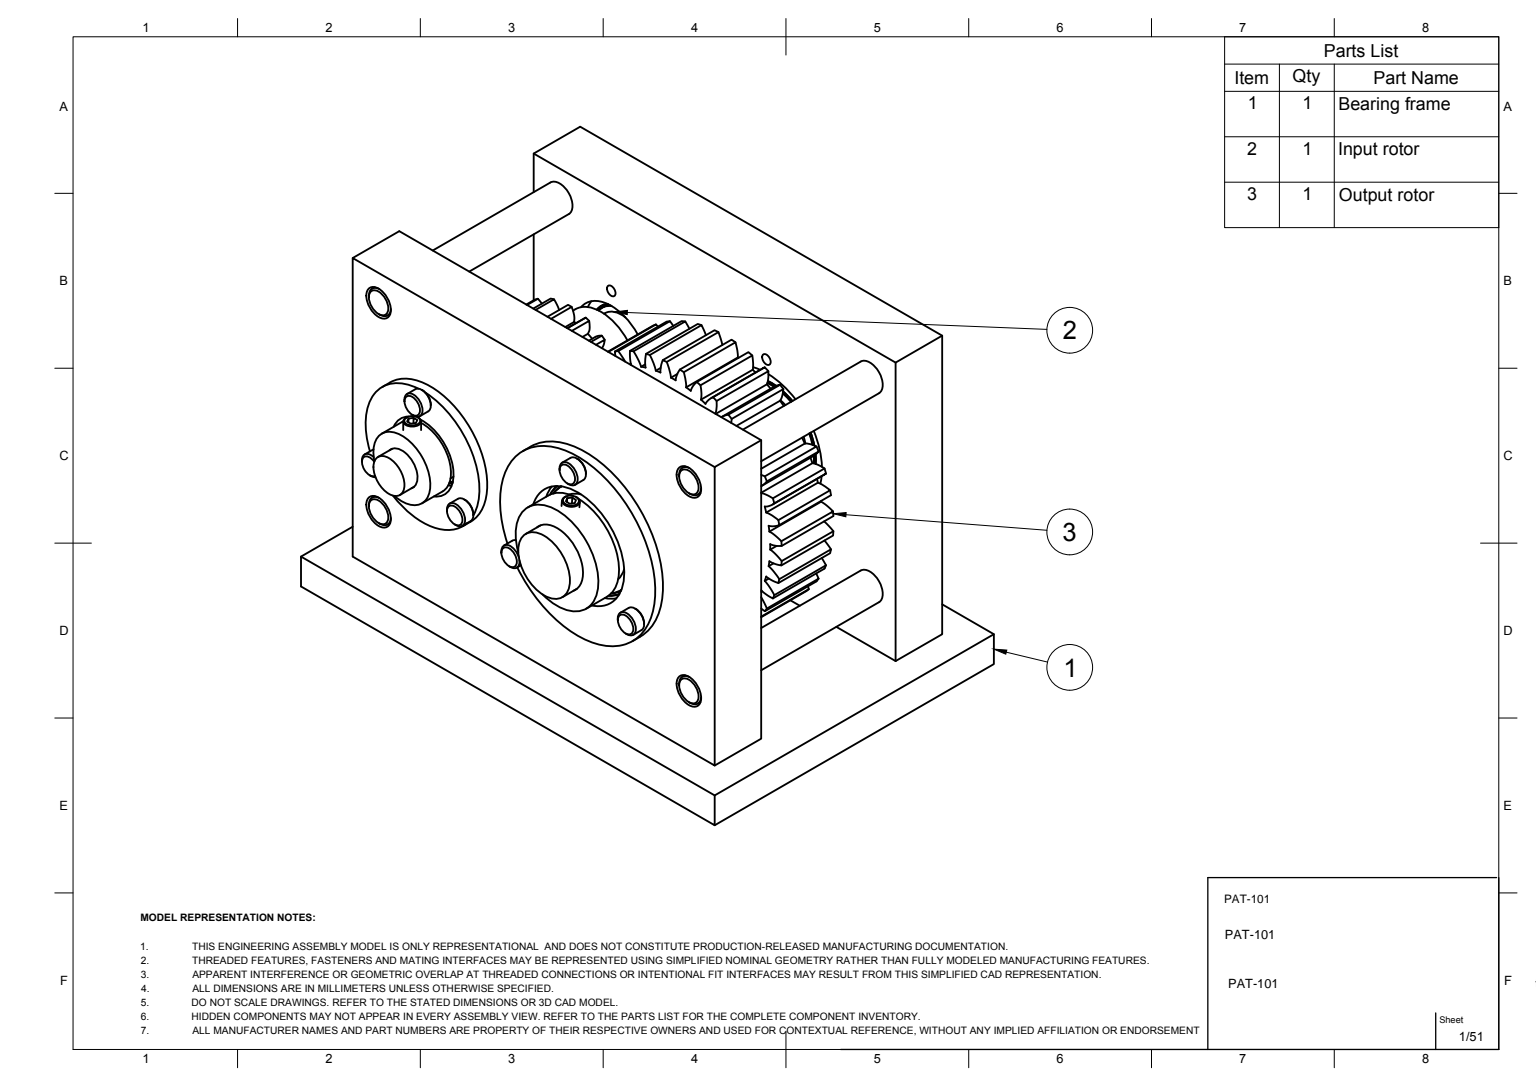
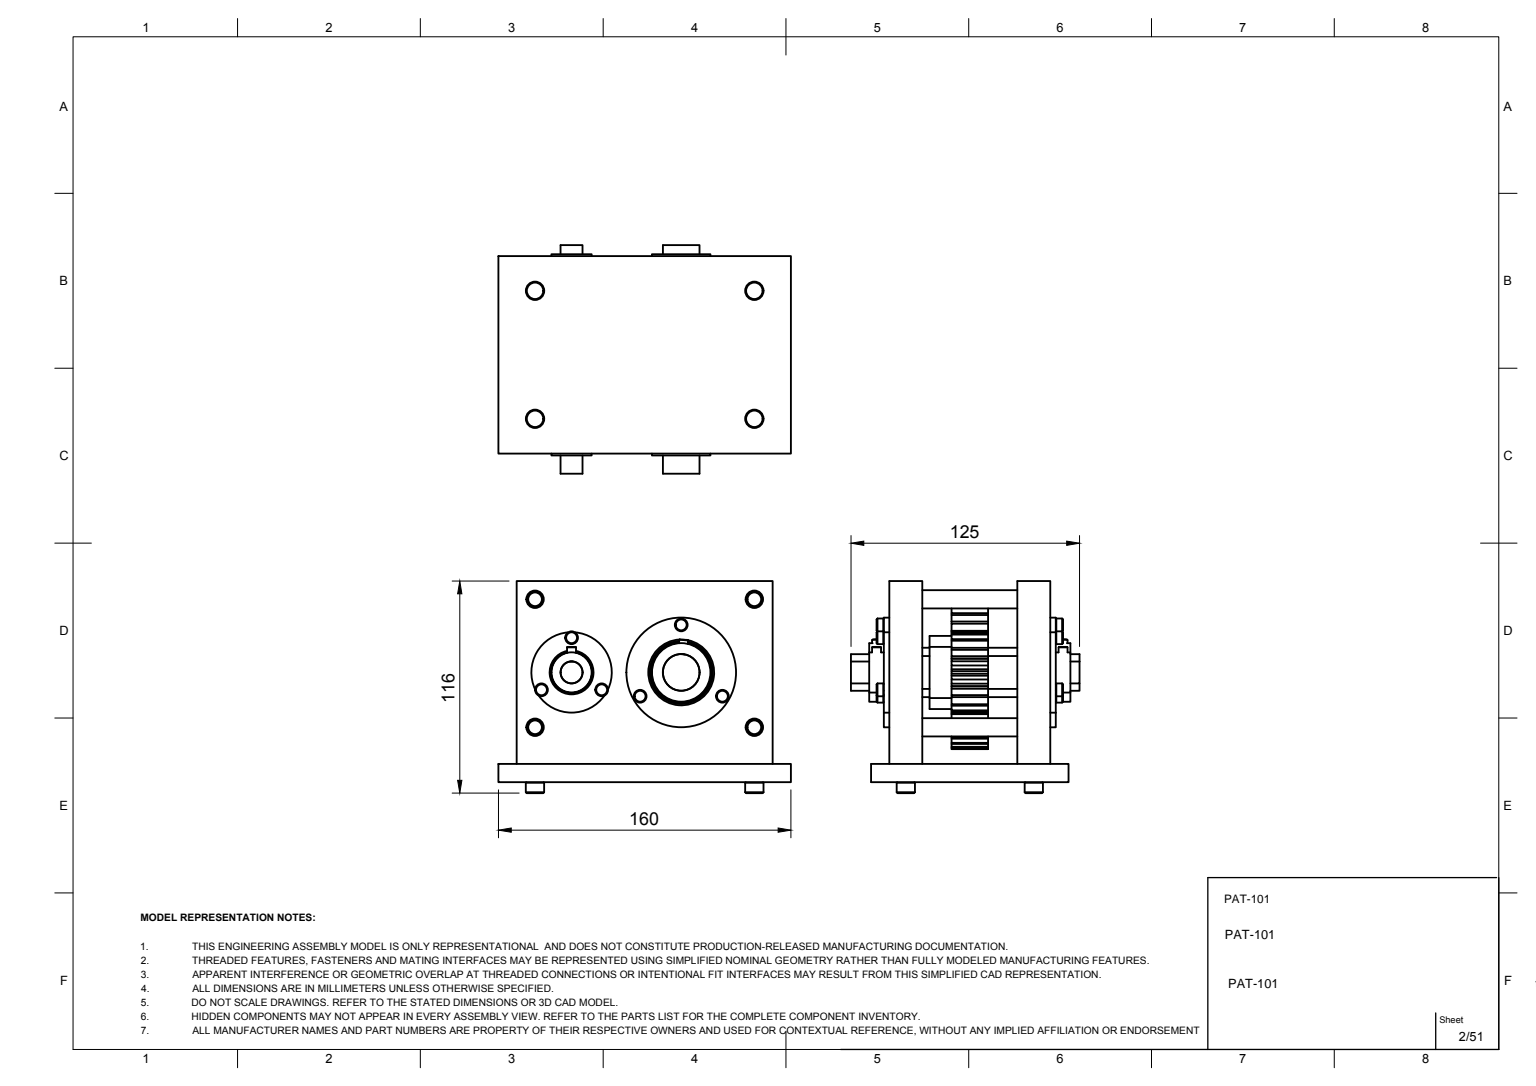
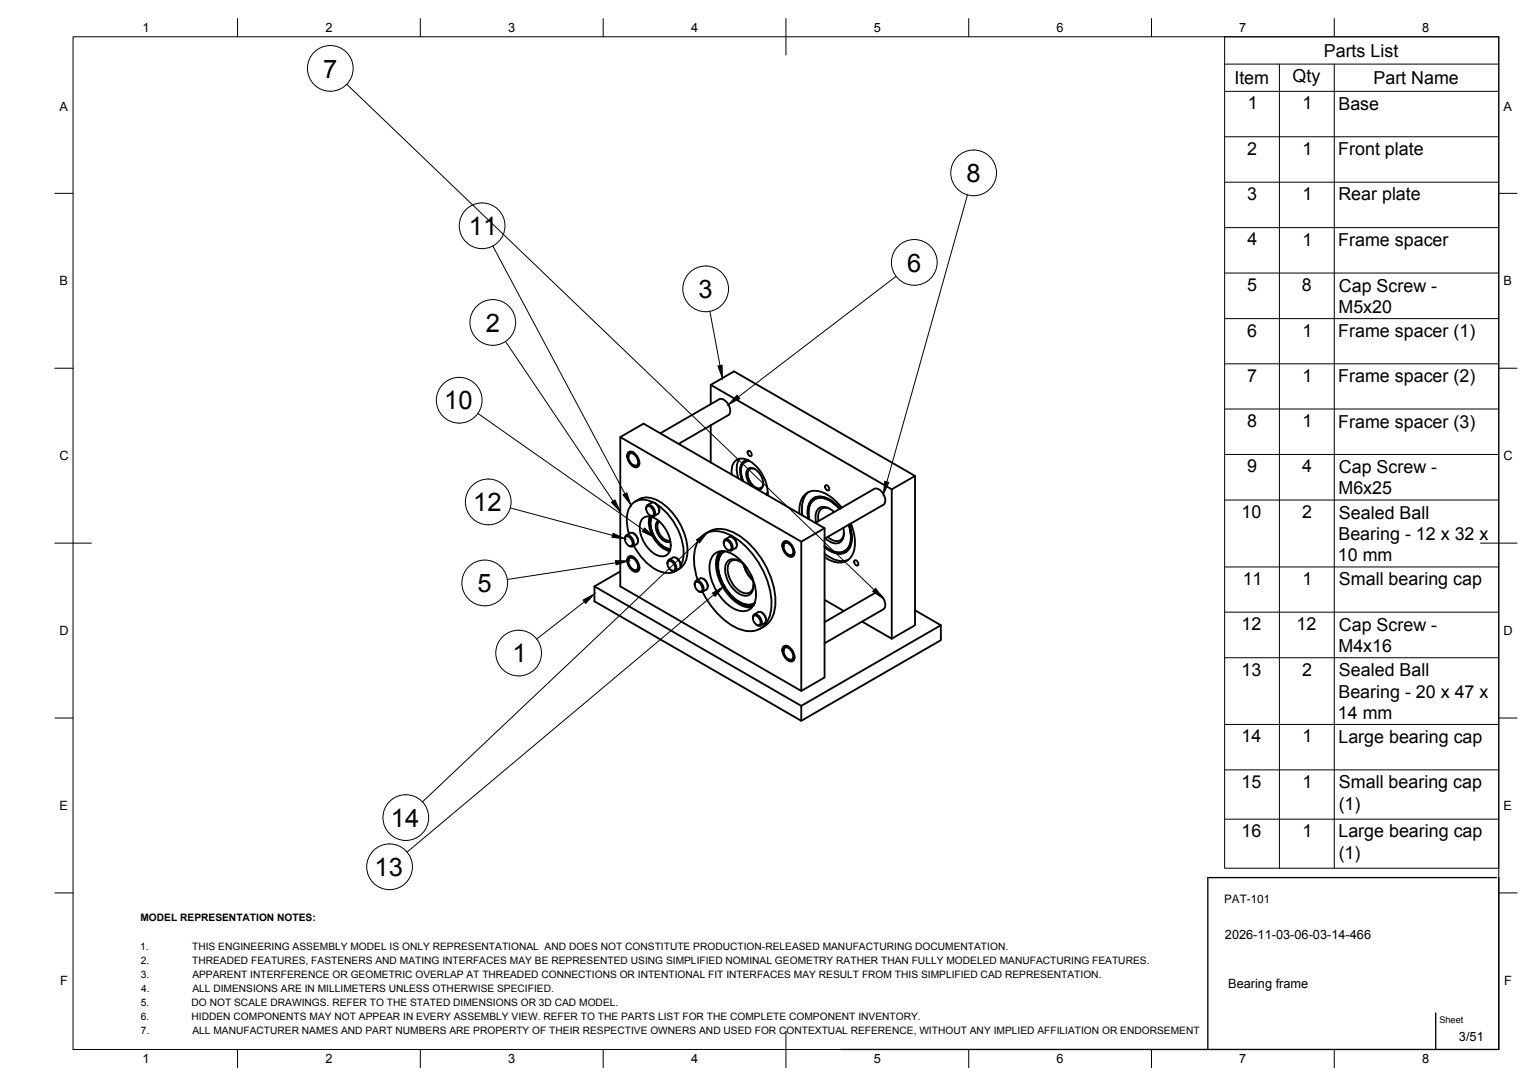
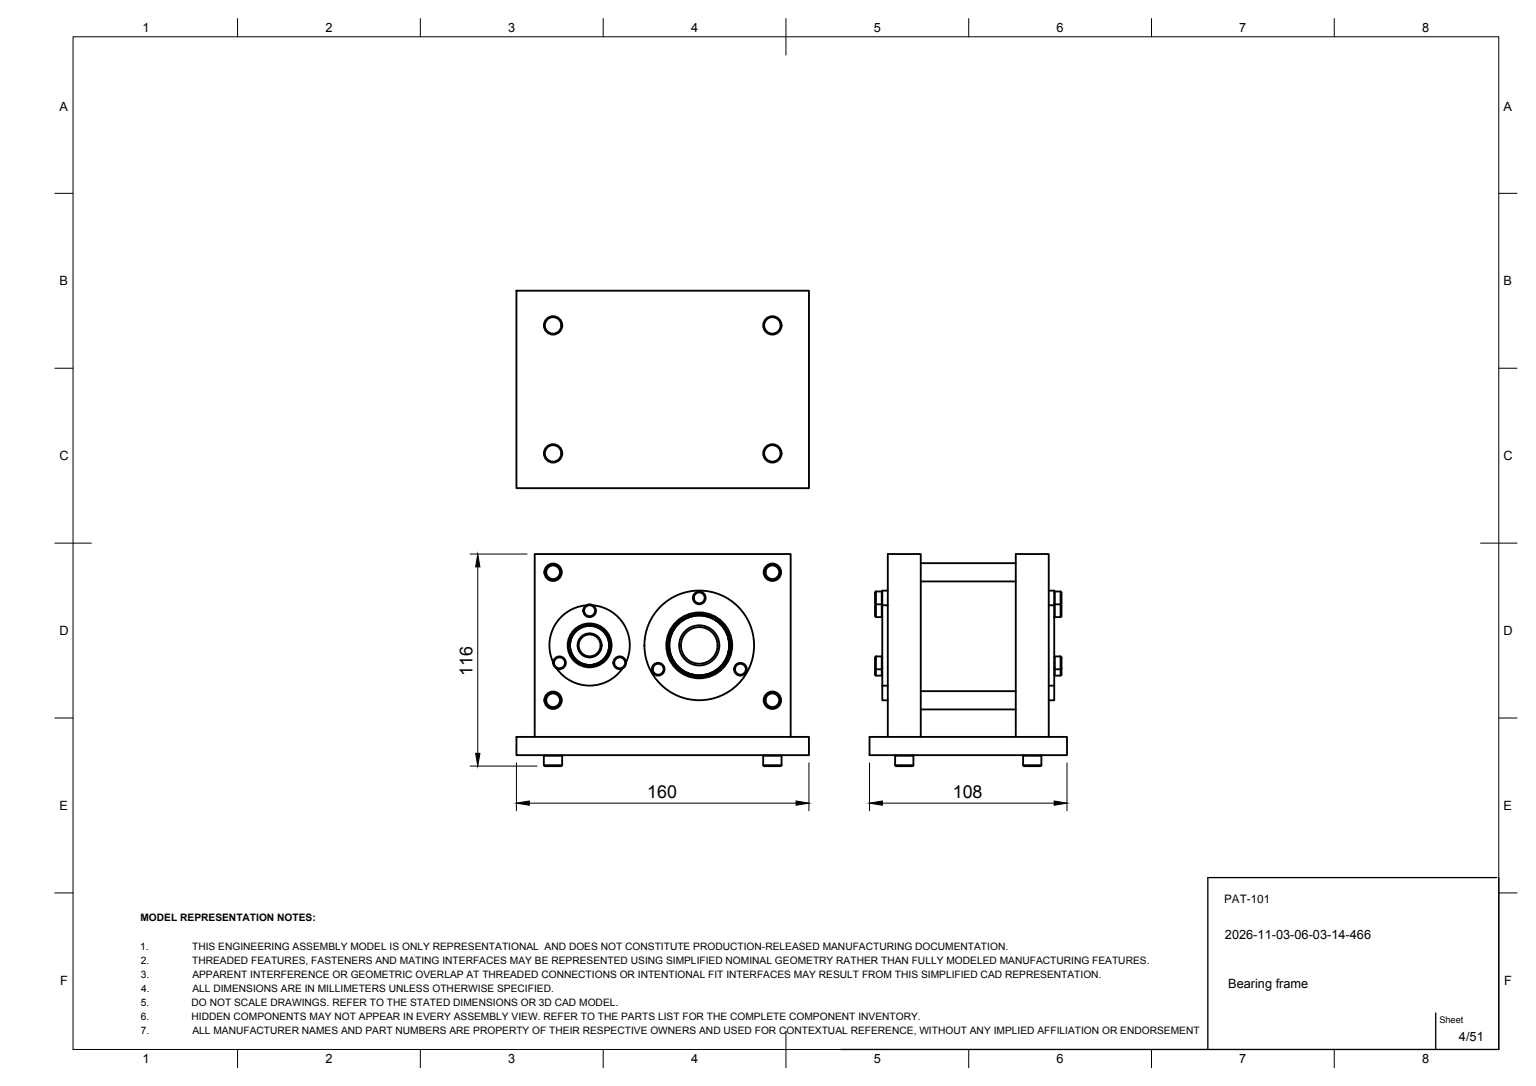
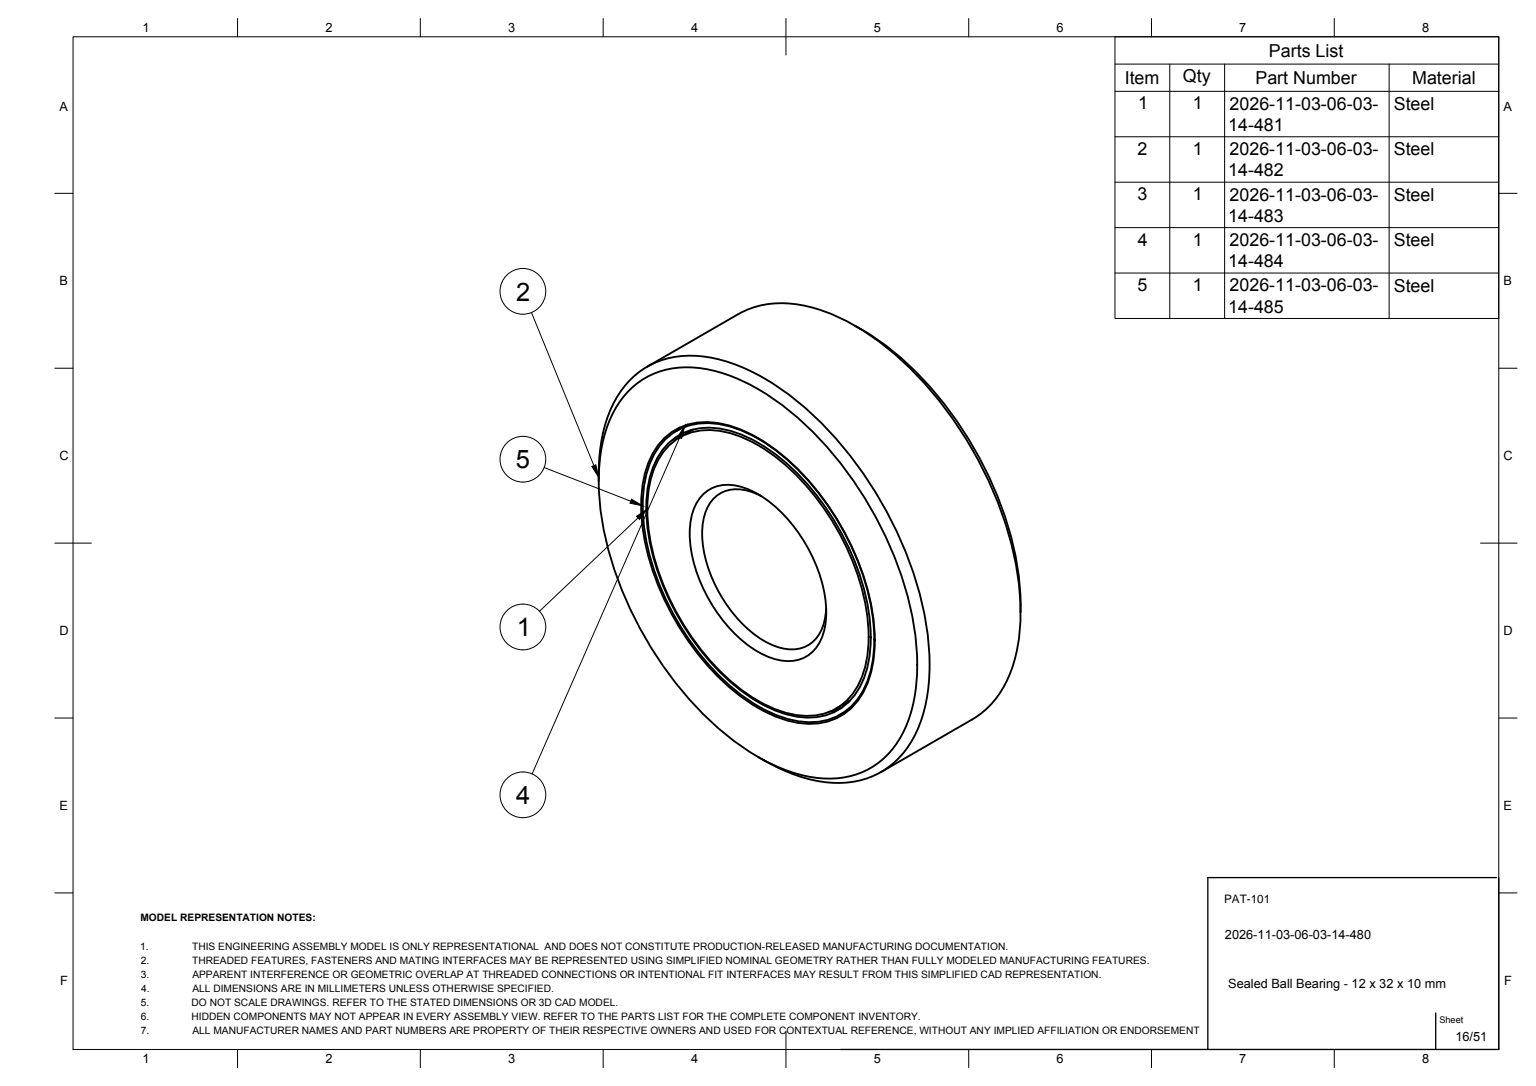
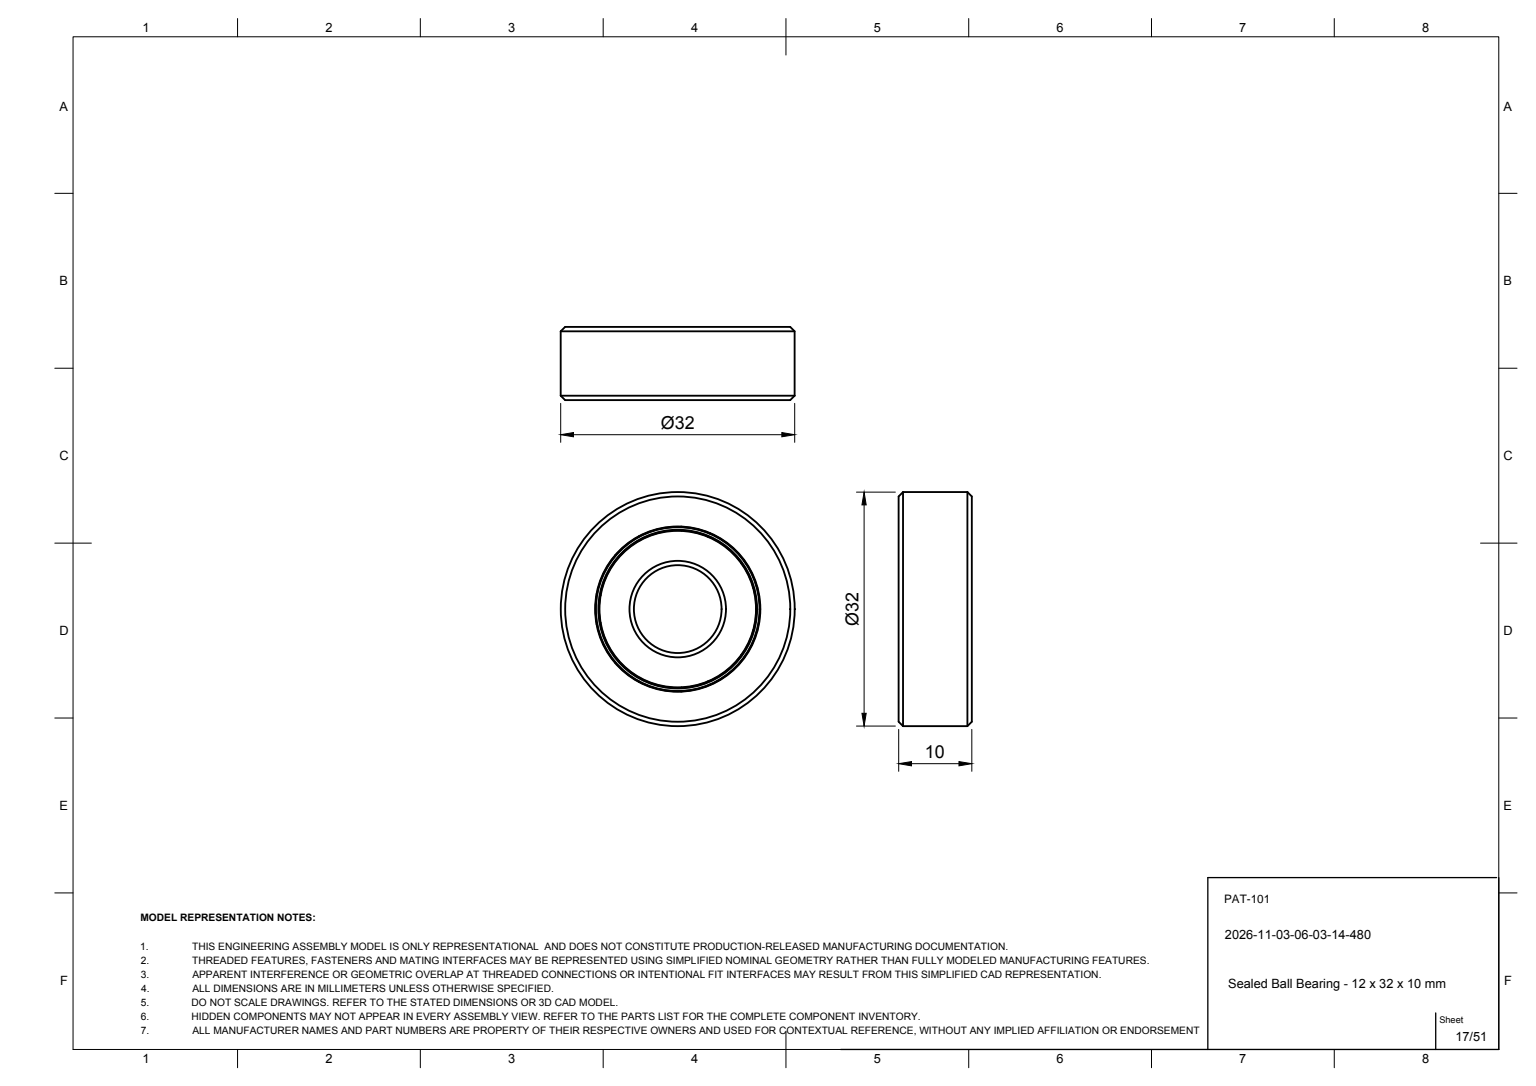
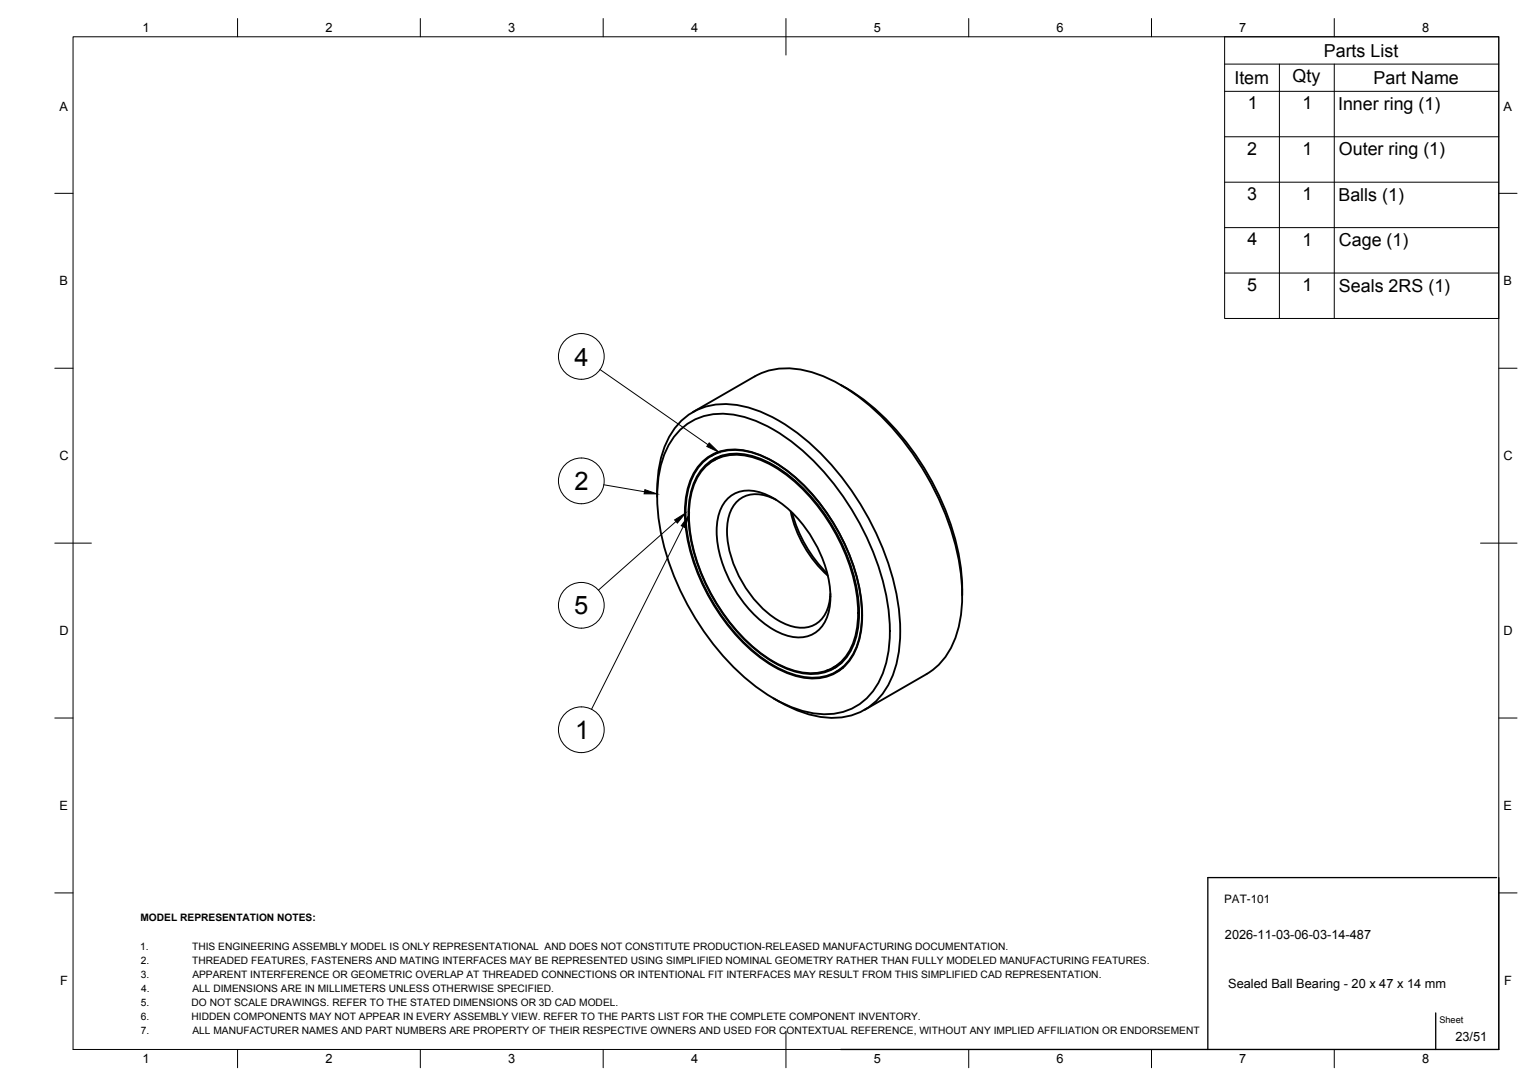
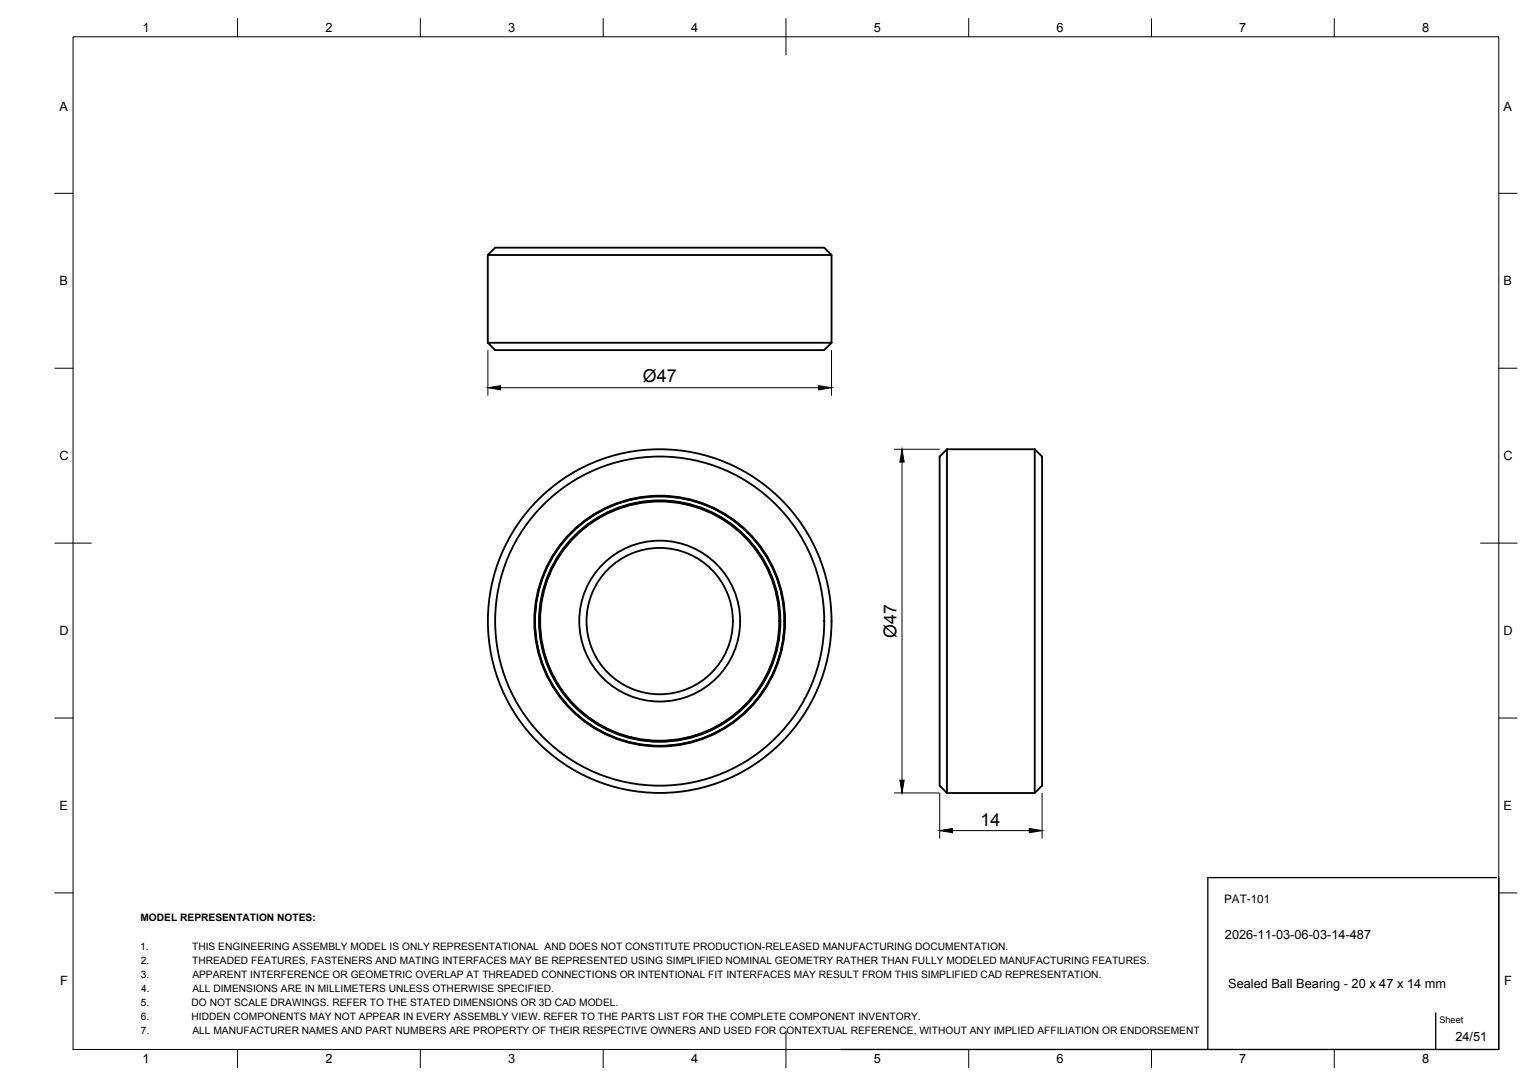
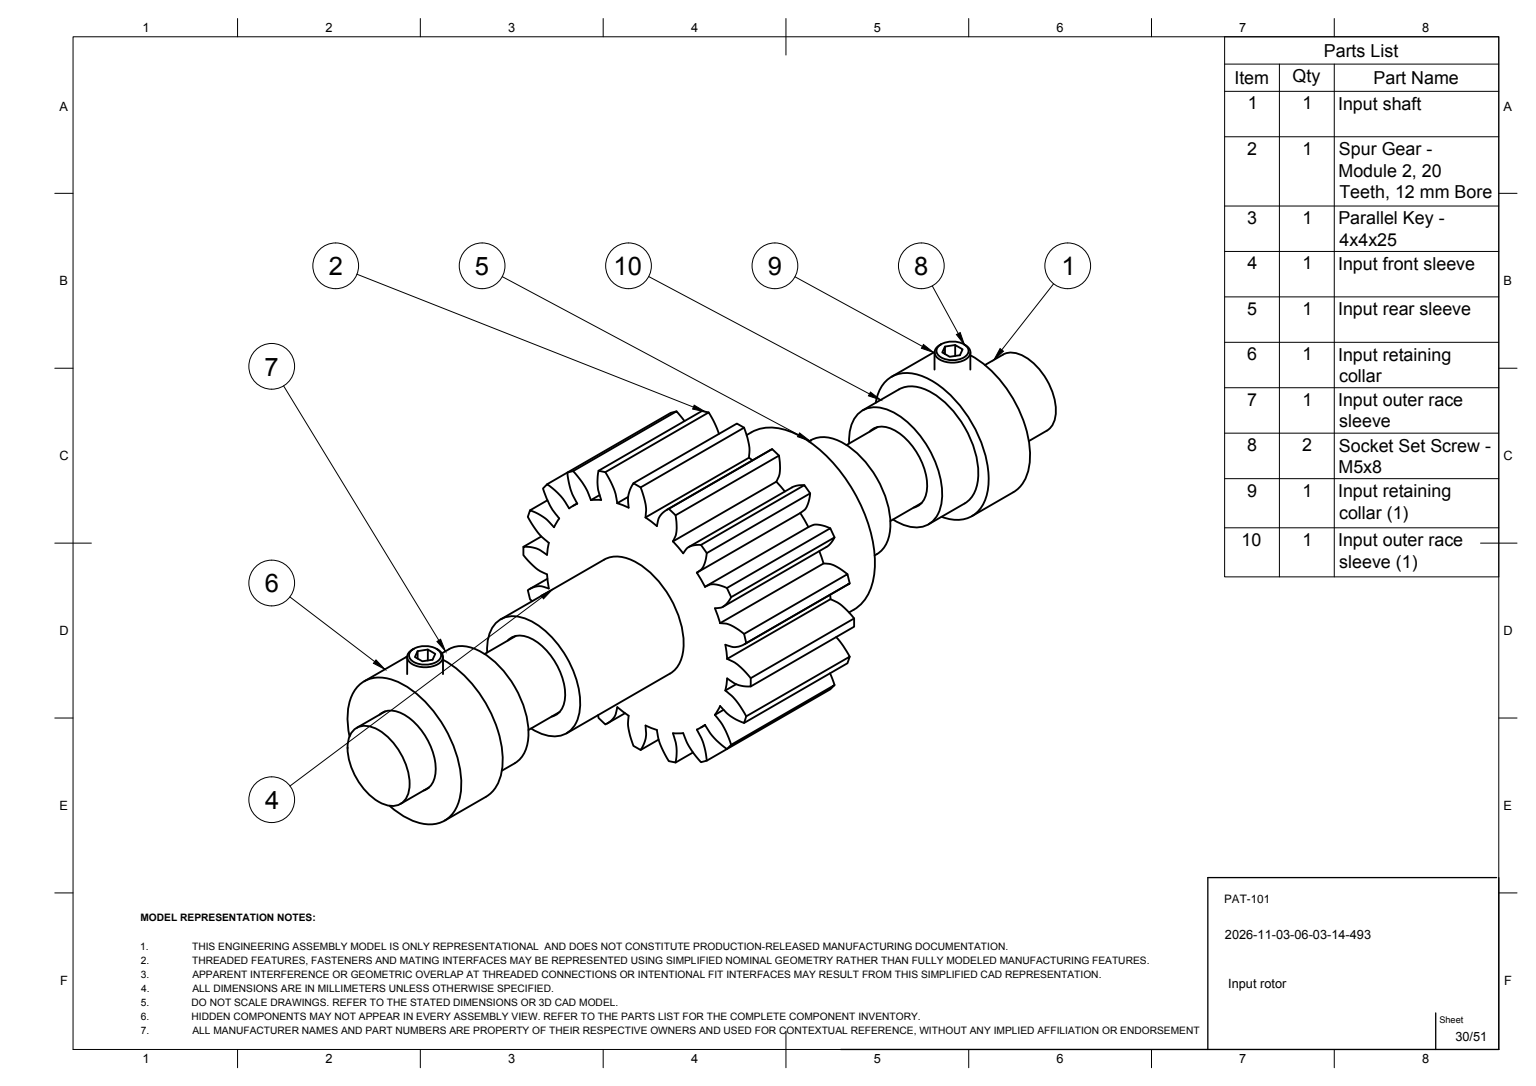
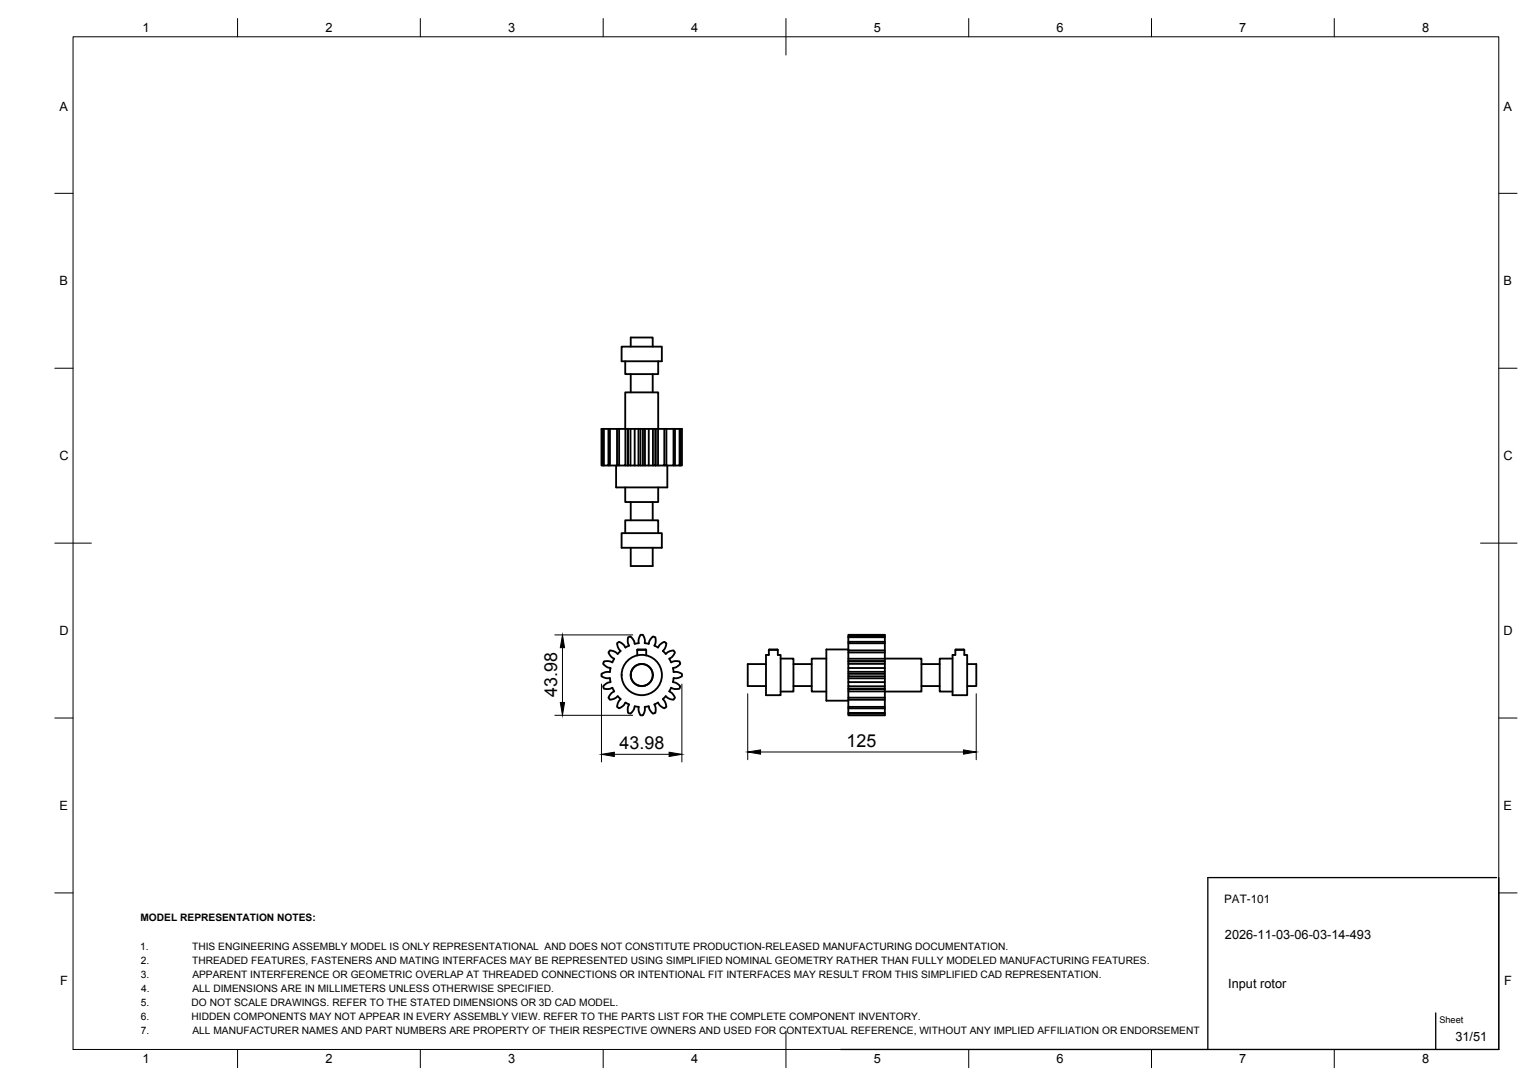
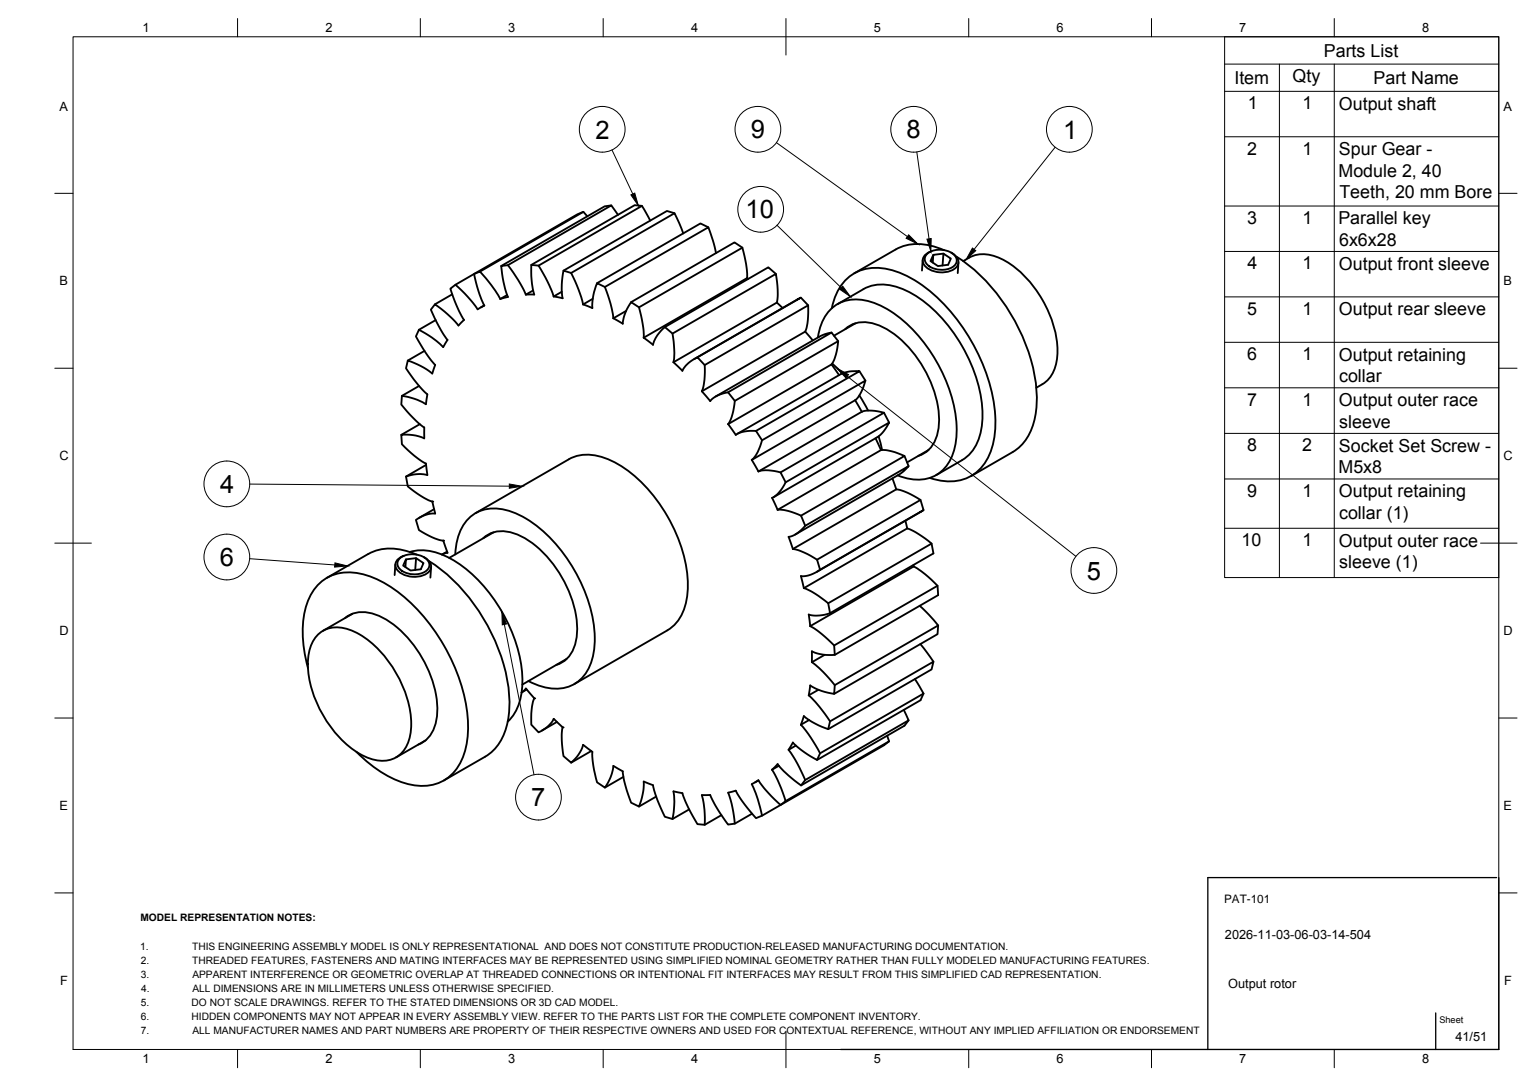
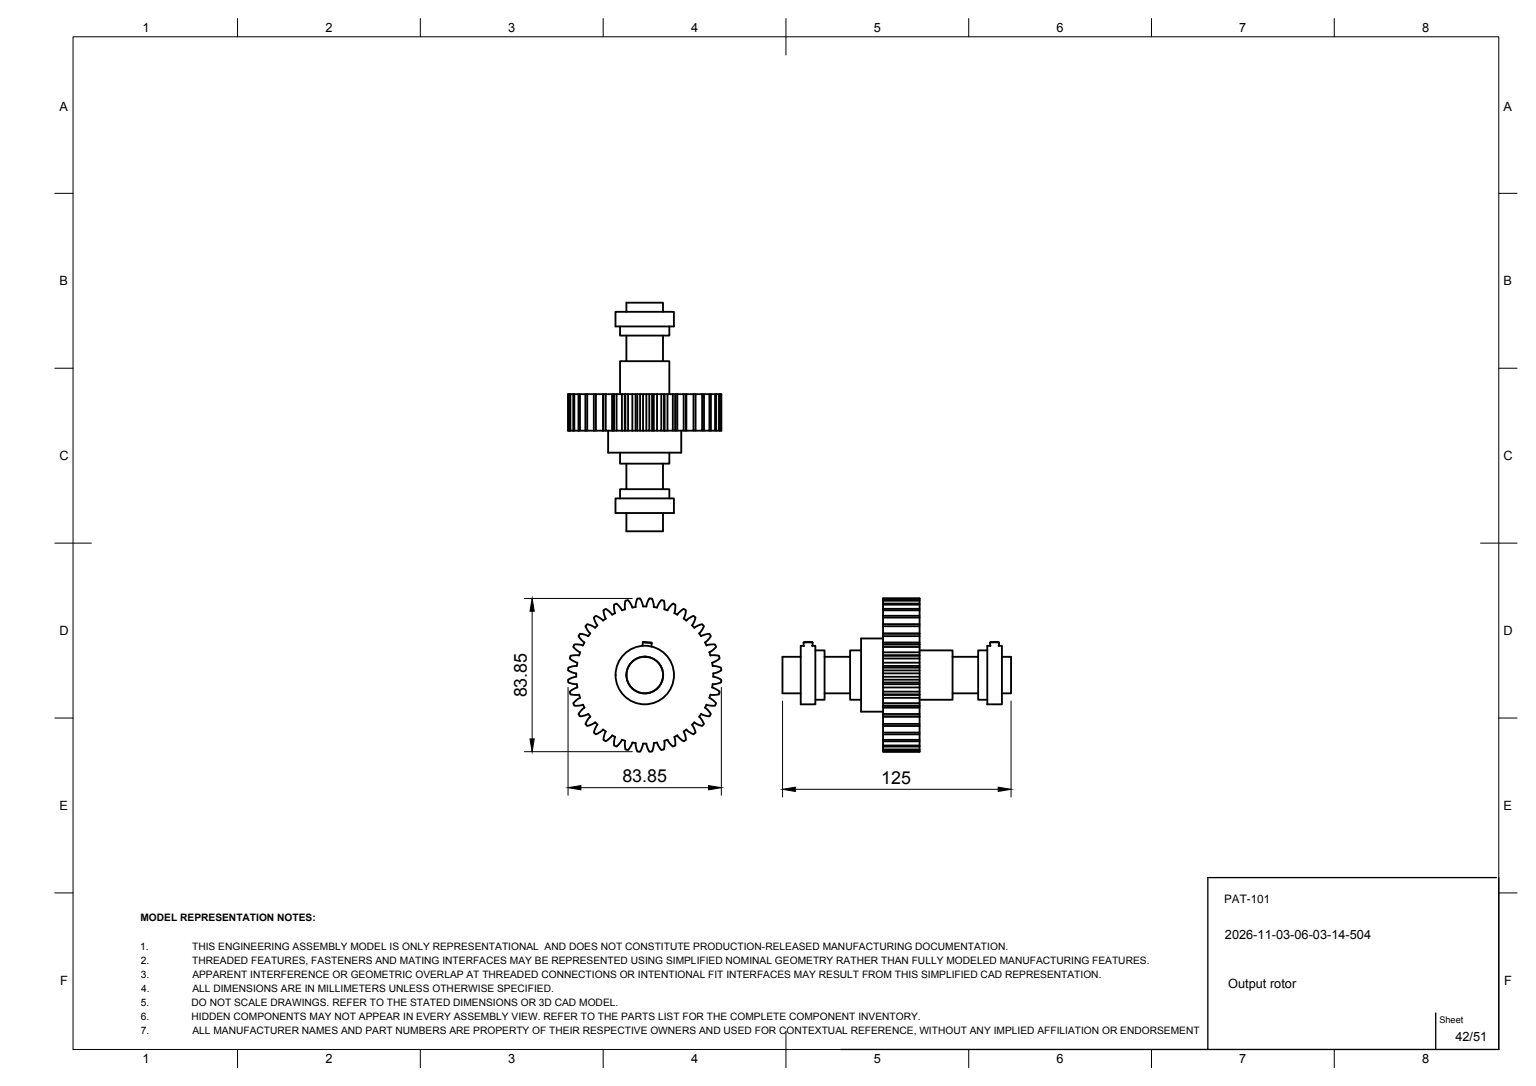
ISO-10303-21;
HEADER;
/* Generated by software containing ST-Developer
 * from STEP Tools, Inc. (www.steptools.com) 
 */

FILE_DESCRIPTION(
/* description */ ('Spur gear reduction stage 2-1 on bearing plates'),
/* implementation_level */ '2;1');

FILE_NAME(
/* name */ 'PAT-101',
/* time_stamp */ '2026-10-28T03:22:07-07:00',
/* author */ (''),
/* organization */ (''),
/* preprocessor_version */ 'ST-DEVELOPER v20.2',
/* originating_system */ 'Autodesk Translation Framework v15.17.0.0',
/* authorisation */ '');

FILE_SCHEMA (('AUTOMOTIVE_DESIGN { 1 0 10303 214 3 1 1 }'));
ENDSEC;

DATA;
#10=MECHANICAL_DESIGN_GEOMETRIC_PRESENTATION_REPRESENTATION('',(#947,#948,
#949,#950,#951,#952,#953,#954,#955,#956,#957,#958,#959,#960,#961,#962,#963,
#964,#965,#966,#967,#968,#969,#970,#971,#972,#973,#974,#975,#976,#977,#978,
#979,#980,#981,#982,#983,#984,#985,#986,#987,#988,#989,#990,#991,#992,#993,
#994,#995,#996,#997,#998,#999,#1000,#1001,#1002,#1003,#1004),#53909);
#11=(
BOUNDED_SURFACE()
B_SPLINE_SURFACE(5,1,((#21141,#21142),(#21143,#21144),(#21145,#21146),(#21147,
#21148),(#21149,#21150),(#21151,#21152),(#21153,#21154),(#21155,#21156),
(#21157,#21158),(#21159,#21160),(#21161,#21162),(#21163,#21164),(#21165,
#21166),(#21167,#21168),(#21169,#21170),(#21171,#21172),(#21173,#21174),
(#21175,#21176),(#21177,#21178),(#21179,#21180),(#21181,#21182),(#21183,
#21184),(#21185,#21186),(#21187,#21188),(#21189,#21190),(#21191,#21192),
(#21193,#21194),(#21195,#21196),(#21197,#21198),(#21199,#21200),(#21201,
#21202),(#21203,#21204),(#21205,#21206),(#21207,#21208),(#21209,#21210),
(#21211,#21212),(#21213,#21214),(#21215,#21216),(#21217,#21218),(#21219,
#21220),(#21221,#21222),(#21223,#21224),(#21225,#21226),(#21227,#21228),
(#21229,#21230),(#21231,#21232),(#21233,#21234),(#21235,#21236),(#21237,
#21238),(#21239,#21240),(#21241,#21242),(#21243,#21244),(#21245,#21246),
(#21247,#21248),(#21249,#21250),(#21251,#21252),(#21253,#21254),(#21255,
#21256),(#21257,#21258),(#21259,#21260),(#21261,#21262),(#21263,#21264),
(#21265,#21266),(#21267,#21268),(#21269,#21270),(#21271,#21272),(#21273,
#21274),(#21275,#21276),(#21277,#21278),(#21279,#21280)),.UNSPECIFIED.,
 .F.,.F.,.F.)
B_SPLINE_SURFACE_WITH_KNOTS((6,1,1,1,1,1,1,1,1,1,1,1,1,1,1,1,1,1,1,1,1,
1,1,1,1,1,1,1,1,1,1,1,1,1,1,1,1,1,1,1,1,1,1,1,1,1,1,1,1,1,1,1,1,1,1,1,1,
1,1,1,1,1,1,1,1,6),(2,2),(-1.,-0.984615384615383,-0.969230769230768,-0.953846153846152,
-0.938461538461537,-0.923076923076922,-0.907692307692306,-0.892307692307691,
-0.876923076923076,-0.86153846153846,-0.846153846153845,-0.83076923076923,
-0.815384615384614,-0.799999999999999,-0.784615384615384,-0.769230769230768,
-0.753846153846153,-0.738461538461538,-0.723076923076922,-0.707692307692307,
-0.692307692307692,-0.676923076923076,-0.661538461538461,-0.646153846153846,
-0.63076923076923,-0.615384615384615,-0.6,-0.584615384615384,-0.569230769230769,
-0.553846153846154,-0.538461538461538,-0.523076923076923,-0.507692307692308,
-0.492307692307692,-0.476923076923077,-0.461538461538462,-0.446153846153846,
-0.430769230769231,-0.415384615384615,-0.4,-0.384615384615385,-0.369230769230769,
-0.353846153846154,-0.338461538461538,-0.323076923076923,-0.307692307692308,
-0.292307692307692,-0.276923076923077,-0.261538461538462,-0.246153846153846,
-0.230769230769231,-0.215384615384615,-0.2,-0.184615384615385,-0.169230769230769,
-0.153846153846154,-0.138461538461538,-0.123076923076923,-0.107692307692308,
-0.0923076923076923,-0.0769230769230769,-0.0615384615384615,-0.0461538461538462,
-0.0307692307692308,-0.0153846153846154,0.),(-1.,1.),.UNSPECIFIED.)
GEOMETRIC_REPRESENTATION_ITEM()
RATIONAL_B_SPLINE_SURFACE(((1.,1.),(1.,1.),(1.,1.),(1.,1.),(1.,1.),(1.,
1.),(1.,1.),(1.,1.),(1.,1.),(1.,1.),(1.,1.),(1.,1.),(1.,1.),(1.,1.),(1.,
1.),(1.,1.),(1.,1.),(1.,1.),(1.,1.),(1.,1.),(1.,1.),(1.,1.),(1.,1.),(1.,
1.),(1.,1.),(1.,1.),(1.,1.),(1.,1.),(1.,1.),(1.,1.),(1.,1.),(1.,1.),(1.,
1.),(1.,1.),(1.,1.),(1.,1.),(1.,1.),(1.,1.),(1.,1.),(1.,1.),(1.,1.),(1.,
1.),(1.,1.),(1.,1.),(1.,1.),(1.,1.),(1.,1.),(1.,1.),(1.,1.),(1.,1.),(1.,
1.),(1.,1.),(1.,1.),(1.,1.),(1.,1.),(1.,1.),(1.,1.),(1.,1.),(1.,1.),(1.,
1.),(1.,1.),(1.,1.),(1.,1.),(1.,1.),(1.,1.),(1.,1.),(1.,1.),(1.,1.),(1.,
1.),(1.,1.)))
REPRESENTATION_ITEM('')
SURFACE()
);
#12=(
BOUNDED_SURFACE()
B_SPLINE_SURFACE(5,1,((#21359,#21360),(#21361,#21362),(#21363,#21364),(#21365,
#21366),(#21367,#21368),(#21369,#21370),(#21371,#21372),(#21373,#21374),
(#21375,#21376),(#21377,#21378),(#21379,#21380),(#21381,#21382),(#21383,
#21384),(#21385,#21386),(#21387,#21388),(#21389,#21390),(#21391,#21392),
(#21393,#21394),(#21395,#21396),(#21397,#21398),(#21399,#21400),(#21401,
#21402),(#21403,#21404),(#21405,#21406),(#21407,#21408),(#21409,#21410),
(#21411,#21412),(#21413,#21414),(#21415,#21416),(#21417,#21418),(#21419,
#21420),(#21421,#21422),(#21423,#21424),(#21425,#21426),(#21427,#21428),
(#21429,#21430),(#21431,#21432),(#21433,#21434),(#21435,#21436),(#21437,
#21438),(#21439,#21440),(#21441,#21442),(#21443,#21444),(#21445,#21446),
(#21447,#21448),(#21449,#21450),(#21451,#21452),(#21453,#21454),(#21455,
#21456),(#21457,#21458),(#21459,#21460),(#21461,#21462),(#21463,#21464),
(#21465,#21466),(#21467,#21468),(#21469,#21470),(#21471,#21472),(#21473,
#21474),(#21475,#21476),(#21477,#21478),(#21479,#21480),(#21481,#21482),
(#21483,#21484),(#21485,#21486),(#21487,#21488),(#21489,#21490),(#21491,
#21492),(#21493,#21494),(#21495,#21496),(#21497,#21498)),.UNSPECIFIED.,
 .F.,.F.,.F.)
B_SPLINE_SURFACE_WITH_KNOTS((6,1,1,1,1,1,1,1,1,1,1,1,1,1,1,1,1,1,1,1,1,
1,1,1,1,1,1,1,1,1,1,1,1,1,1,1,1,1,1,1,1,1,1,1,1,1,1,1,1,1,1,1,1,1,1,1,1,
1,1,1,1,1,1,1,1,6),(2,2),(-1.,-0.984615384615383,-0.969230769230768,-0.953846153846152,
-0.938461538461537,-0.923076923076922,-0.907692307692306,-0.892307692307691,
-0.876923076923076,-0.86153846153846,-0.846153846153845,-0.83076923076923,
-0.815384615384614,-0.799999999999999,-0.784615384615384,-0.769230769230768,
-0.753846153846153,-0.738461538461538,-0.723076923076922,-0.707692307692307,
-0.692307692307692,-0.676923076923076,-0.661538461538461,-0.646153846153846,
-0.63076923076923,-0.615384615384615,-0.6,-0.584615384615384,-0.569230769230769,
-0.553846153846154,-0.538461538461538,-0.523076923076923,-0.507692307692308,
-0.492307692307692,-0.476923076923077,-0.461538461538462,-0.446153846153846,
-0.430769230769231,-0.415384615384615,-0.4,-0.384615384615385,-0.369230769230769,
-0.353846153846154,-0.338461538461538,-0.323076923076923,-0.307692307692308,
-0.292307692307692,-0.276923076923077,-0.261538461538462,-0.246153846153846,
-0.230769230769231,-0.215384615384615,-0.2,-0.184615384615385,-0.169230769230769,
-0.153846153846154,-0.138461538461538,-0.123076923076923,-0.107692307692308,
-0.0923076923076923,-0.0769230769230769,-0.0615384615384615,-0.0461538461538462,
-0.0307692307692308,-0.0153846153846154,0.),(-1.,1.),.UNSPECIFIED.)
GEOMETRIC_REPRESENTATION_ITEM()
RATIONAL_B_SPLINE_SURFACE(((1.,1.),(1.,1.),(1.,1.),(1.,1.),(1.,1.),(1.,
1.),(1.,1.),(1.,1.),(1.,1.),(1.,1.),(1.,1.),(1.,1.),(1.,1.),(1.,1.),(1.,
1.),(1.,1.),(1.,1.),(1.,1.),(1.,1.),(1.,1.),(1.,1.),(1.,1.),(1.,1.),(1.,
1.),(1.,1.),(1.,1.),(1.,1.),(1.,1.),(1.,1.),(1.,1.),(1.,1.),(1.,1.),(1.,
1.),(1.,1.),(1.,1.),(1.,1.),(1.,1.),(1.,1.),(1.,1.),(1.,1.),(1.,1.),(1.,
1.),(1.,1.),(1.,1.),(1.,1.),(1.,1.),(1.,1.),(1.,1.),(1.,1.),(1.,1.),(1.,
1.),(1.,1.),(1.,1.),(1.,1.),(1.,1.),(1.,1.),(1.,1.),(1.,1.),(1.,1.),(1.,
1.),(1.,1.),(1.,1.),(1.,1.),(1.,1.),(1.,1.),(1.,1.),(1.,1.),(1.,1.),(1.,
1.),(1.,1.)))
REPRESENTATION_ITEM('')
SURFACE()
);
#13=(
BOUNDED_SURFACE()
B_SPLINE_SURFACE(5,1,((#21575,#21576),(#21577,#21578),(#21579,#21580),(#21581,
#21582),(#21583,#21584),(#21585,#21586),(#21587,#21588),(#21589,#21590),
(#21591,#21592),(#21593,#21594),(#21595,#21596),(#21597,#21598),(#21599,
#21600),(#21601,#21602),(#21603,#21604),(#21605,#21606),(#21607,#21608),
(#21609,#21610),(#21611,#21612),(#21613,#21614),(#21615,#21616),(#21617,
#21618),(#21619,#21620),(#21621,#21622),(#21623,#21624),(#21625,#21626),
(#21627,#21628),(#21629,#21630),(#21631,#21632),(#21633,#21634),(#21635,
#21636),(#21637,#21638),(#21639,#21640),(#21641,#21642),(#21643,#21644),
(#21645,#21646),(#21647,#21648),(#21649,#21650),(#21651,#21652),(#21653,
#21654),(#21655,#21656),(#21657,#21658),(#21659,#21660),(#21661,#21662),
(#21663,#21664),(#21665,#21666),(#21667,#21668),(#21669,#21670),(#21671,
#21672),(#21673,#21674),(#21675,#21676),(#21677,#21678),(#21679,#21680),
(#21681,#21682),(#21683,#21684),(#21685,#21686),(#21687,#21688),(#21689,
#21690),(#21691,#21692),(#21693,#21694),(#21695,#21696),(#21697,#21698),
(#21699,#21700),(#21701,#21702),(#21703,#21704),(#21705,#21706),(#21707,
#21708),(#21709,#21710),(#21711,#21712),(#21713,#21714)),.UNSPECIFIED.,
 .F.,.F.,.F.)
B_SPLINE_SURFACE_WITH_KNOTS((6,1,1,1,1,1,1,1,1,1,1,1,1,1,1,1,1,1,1,1,1,
1,1,1,1,1,1,1,1,1,1,1,1,1,1,1,1,1,1,1,1,1,1,1,1,1,1,1,1,1,1,1,1,1,1,1,1,
1,1,1,1,1,1,1,1,6),(2,2),(-1.,-0.984615384615383,-0.969230769230768,-0.953846153846152,
-0.938461538461537,-0.923076923076922,-0.907692307692306,-0.892307692307691,
-0.876923076923076,-0.86153846153846,-0.846153846153845,-0.83076923076923,
-0.815384615384614,-0.799999999999999,-0.784615384615384,-0.769230769230768,
-0.753846153846153,-0.738461538461538,-0.723076923076922,-0.707692307692307,
-0.692307692307692,-0.676923076923076,-0.661538461538461,-0.646153846153846,
-0.63076923076923,-0.615384615384615,-0.6,-0.584615384615384,-0.569230769230769,
-0.553846153846154,-0.538461538461538,-0.523076923076923,-0.507692307692308,
-0.492307692307692,-0.476923076923077,-0.461538461538462,-0.446153846153846,
-0.430769230769231,-0.415384615384615,-0.4,-0.384615384615385,-0.369230769230769,
-0.353846153846154,-0.338461538461538,-0.323076923076923,-0.307692307692308,
-0.292307692307692,-0.276923076923077,-0.261538461538462,-0.246153846153846,
-0.230769230769231,-0.215384615384615,-0.2,-0.184615384615385,-0.169230769230769,
-0.153846153846154,-0.138461538461538,-0.123076923076923,-0.107692307692308,
-0.0923076923076923,-0.0769230769230769,-0.0615384615384615,-0.0461538461538462,
-0.0307692307692308,-0.0153846153846154,0.),(-1.,1.),.UNSPECIFIED.)
GEOMETRIC_REPRESENTATION_ITEM()
RATIONAL_B_SPLINE_SURFACE(((1.,1.),(1.,1.),(1.,1.),(1.,1.),(1.,1.),(1.,
1.),(1.,1.),(1.,1.),(1.,1.),(1.,1.),(1.,1.),(1.,1.),(1.,1.),(1.,1.),(1.,
1.),(1.,1.),(1.,1.),(1.,1.),(1.,1.),(1.,1.),(1.,1.),(1.,1.),(1.,1.),(1.,
1.),(1.,1.),(1.,1.),(1.,1.),(1.,1.),(1.,1.),(1.,1.),(1.,1.),(1.,1.),(1.,
1.),(1.,1.),(1.,1.),(1.,1.),(1.,1.),(1.,1.),(1.,1.),(1.,1.),(1.,1.),(1.,
1.),(1.,1.),(1.,1.),(1.,1.),(1.,1.),(1.,1.),(1.,1.),(1.,1.),(1.,1.),(1.,
1.),(1.,1.),(1.,1.),(1.,1.),(1.,1.),(1.,1.),(1.,1.),(1.,1.),(1.,1.),(1.,
1.),(1.,1.),(1.,1.),(1.,1.),(1.,1.),(1.,1.),(1.,1.),(1.,1.),(1.,1.),(1.,
1.),(1.,1.)))
REPRESENTATION_ITEM('')
SURFACE()
);
#14=(
BOUNDED_SURFACE()
B_SPLINE_SURFACE(5,1,((#21791,#21792),(#21793,#21794),(#21795,#21796),(#21797,
#21798),(#21799,#21800),(#21801,#21802),(#21803,#21804),(#21805,#21806),
(#21807,#21808),(#21809,#21810),(#21811,#21812),(#21813,#21814),(#21815,
#21816),(#21817,#21818),(#21819,#21820),(#21821,#21822),(#21823,#21824),
(#21825,#21826),(#21827,#21828),(#21829,#21830),(#21831,#21832),(#21833,
#21834),(#21835,#21836),(#21837,#21838),(#21839,#21840),(#21841,#21842),
(#21843,#21844),(#21845,#21846),(#21847,#21848),(#21849,#21850),(#21851,
#21852),(#21853,#21854),(#21855,#21856),(#21857,#21858),(#21859,#21860),
(#21861,#21862),(#21863,#21864),(#21865,#21866),(#21867,#21868),(#21869,
#21870),(#21871,#21872),(#21873,#21874),(#21875,#21876),(#21877,#21878),
(#21879,#21880),(#21881,#21882),(#21883,#21884),(#21885,#21886),(#21887,
#21888),(#21889,#21890),(#21891,#21892),(#21893,#21894),(#21895,#21896),
(#21897,#21898),(#21899,#21900),(#21901,#21902),(#21903,#21904),(#21905,
#21906),(#21907,#21908),(#21909,#21910),(#21911,#21912),(#21913,#21914),
(#21915,#21916),(#21917,#21918),(#21919,#21920),(#21921,#21922),(#21923,
#21924),(#21925,#21926),(#21927,#21928),(#21929,#21930)),.UNSPECIFIED.,
 .F.,.F.,.F.)
B_SPLINE_SURFACE_WITH_KNOTS((6,1,1,1,1,1,1,1,1,1,1,1,1,1,1,1,1,1,1,1,1,
1,1,1,1,1,1,1,1,1,1,1,1,1,1,1,1,1,1,1,1,1,1,1,1,1,1,1,1,1,1,1,1,1,1,1,1,
1,1,1,1,1,1,1,1,6),(2,2),(-1.,-0.984615384615383,-0.969230769230768,-0.953846153846152,
-0.938461538461537,-0.923076923076922,-0.907692307692306,-0.892307692307691,
-0.876923076923076,-0.86153846153846,-0.846153846153845,-0.83076923076923,
-0.815384615384614,-0.799999999999999,-0.784615384615384,-0.769230769230768,
-0.753846153846153,-0.738461538461538,-0.723076923076922,-0.707692307692307,
-0.692307692307692,-0.676923076923076,-0.661538461538461,-0.646153846153846,
-0.63076923076923,-0.615384615384615,-0.6,-0.584615384615384,-0.569230769230769,
-0.553846153846154,-0.538461538461538,-0.523076923076923,-0.507692307692308,
-0.492307692307692,-0.476923076923077,-0.461538461538462,-0.446153846153846,
-0.430769230769231,-0.415384615384615,-0.4,-0.384615384615385,-0.369230769230769,
-0.353846153846154,-0.338461538461538,-0.323076923076923,-0.307692307692308,
-0.292307692307692,-0.276923076923077,-0.261538461538462,-0.246153846153846,
-0.230769230769231,-0.215384615384615,-0.2,-0.184615384615385,-0.169230769230769,
-0.153846153846154,-0.138461538461538,-0.123076923076923,-0.107692307692308,
-0.0923076923076923,-0.0769230769230769,-0.0615384615384615,-0.0461538461538462,
-0.0307692307692308,-0.0153846153846154,0.),(-1.,1.),.UNSPECIFIED.)
GEOMETRIC_REPRESENTATION_ITEM()
RATIONAL_B_SPLINE_SURFACE(((1.,1.),(1.,1.),(1.,1.),(1.,1.),(1.,1.),(1.,
1.),(1.,1.),(1.,1.),(1.,1.),(1.,1.),(1.,1.),(1.,1.),(1.,1.),(1.,1.),(1.,
1.),(1.,1.),(1.,1.),(1.,1.),(1.,1.),(1.,1.),(1.,1.),(1.,1.),(1.,1.),(1.,
1.),(1.,1.),(1.,1.),(1.,1.),(1.,1.),(1.,1.),(1.,1.),(1.,1.),(1.,1.),(1.,
1.),(1.,1.),(1.,1.),(1.,1.),(1.,1.),(1.,1.),(1.,1.),(1.,1.),(1.,1.),(1.,
1.),(1.,1.),(1.,1.),(1.,1.),(1.,1.),(1.,1.),(1.,1.),(1.,1.),(1.,1.),(1.,
1.),(1.,1.),(1.,1.),(1.,1.),(1.,1.),(1.,1.),(1.,1.),(1.,1.),(1.,1.),(1.,
1.),(1.,1.),(1.,1.),(1.,1.),(1.,1.),(1.,1.),(1.,1.),(1.,1.),(1.,1.),(1.,
1.),(1.,1.)))
REPRESENTATION_ITEM('')
SURFACE()
);
#15=(
BOUNDED_SURFACE()
B_SPLINE_SURFACE(5,1,((#22007,#22008),(#22009,#22010),(#22011,#22012),(#22013,
#22014),(#22015,#22016),(#22017,#22018),(#22019,#22020),(#22021,#22022),
(#22023,#22024),(#22025,#22026),(#22027,#22028),(#22029,#22030),(#22031,
#22032),(#22033,#22034),(#22035,#22036),(#22037,#22038),(#22039,#22040),
(#22041,#22042),(#22043,#22044),(#22045,#22046),(#22047,#22048),(#22049,
#22050),(#22051,#22052),(#22053,#22054),(#22055,#22056),(#22057,#22058),
(#22059,#22060),(#22061,#22062),(#22063,#22064),(#22065,#22066),(#22067,
#22068),(#22069,#22070),(#22071,#22072),(#22073,#22074),(#22075,#22076),
(#22077,#22078),(#22079,#22080),(#22081,#22082),(#22083,#22084),(#22085,
#22086),(#22087,#22088),(#22089,#22090),(#22091,#22092),(#22093,#22094),
(#22095,#22096),(#22097,#22098),(#22099,#22100),(#22101,#22102),(#22103,
#22104),(#22105,#22106),(#22107,#22108),(#22109,#22110),(#22111,#22112),
(#22113,#22114),(#22115,#22116),(#22117,#22118),(#22119,#22120),(#22121,
#22122),(#22123,#22124),(#22125,#22126),(#22127,#22128),(#22129,#22130),
(#22131,#22132),(#22133,#22134),(#22135,#22136),(#22137,#22138),(#22139,
#22140),(#22141,#22142),(#22143,#22144),(#22145,#22146)),.UNSPECIFIED.,
 .F.,.F.,.F.)
B_SPLINE_SURFACE_WITH_KNOTS((6,1,1,1,1,1,1,1,1,1,1,1,1,1,1,1,1,1,1,1,1,
1,1,1,1,1,1,1,1,1,1,1,1,1,1,1,1,1,1,1,1,1,1,1,1,1,1,1,1,1,1,1,1,1,1,1,1,
1,1,1,1,1,1,1,1,6),(2,2),(-1.,-0.984615384615383,-0.969230769230768,-0.953846153846152,
-0.938461538461537,-0.923076923076922,-0.907692307692306,-0.892307692307691,
-0.876923076923076,-0.86153846153846,-0.846153846153845,-0.83076923076923,
-0.815384615384614,-0.799999999999999,-0.784615384615384,-0.769230769230768,
-0.753846153846153,-0.738461538461538,-0.723076923076922,-0.707692307692307,
-0.692307692307692,-0.676923076923076,-0.661538461538461,-0.646153846153846,
-0.63076923076923,-0.615384615384615,-0.6,-0.584615384615384,-0.569230769230769,
-0.553846153846154,-0.538461538461538,-0.523076923076923,-0.507692307692308,
-0.492307692307692,-0.476923076923077,-0.461538461538462,-0.446153846153846,
-0.430769230769231,-0.415384615384615,-0.4,-0.384615384615385,-0.369230769230769,
-0.353846153846154,-0.338461538461538,-0.323076923076923,-0.307692307692308,
-0.292307692307692,-0.276923076923077,-0.261538461538462,-0.246153846153846,
-0.230769230769231,-0.215384615384615,-0.2,-0.184615384615385,-0.169230769230769,
-0.153846153846154,-0.138461538461538,-0.123076923076923,-0.107692307692308,
-0.0923076923076923,-0.0769230769230769,-0.0615384615384615,-0.0461538461538462,
-0.0307692307692308,-0.0153846153846154,0.),(-1.,1.),.UNSPECIFIED.)
GEOMETRIC_REPRESENTATION_ITEM()
RATIONAL_B_SPLINE_SURFACE(((1.,1.),(1.,1.),(1.,1.),(1.,1.),(1.,1.),(1.,
1.),(1.,1.),(1.,1.),(1.,1.),(1.,1.),(1.,1.),(1.,1.),(1.,1.),(1.,1.),(1.,
1.),(1.,1.),(1.,1.),(1.,1.),(1.,1.),(1.,1.),(1.,1.),(1.,1.),(1.,1.),(1.,
1.),(1.,1.),(1.,1.),(1.,1.),(1.,1.),(1.,1.),(1.,1.),(1.,1.),(1.,1.),(1.,
1.),(1.,1.),(1.,1.),(1.,1.),(1.,1.),(1.,1.),(1.,1.),(1.,1.),(1.,1.),(1.,
1.),(1.,1.),(1.,1.),(1.,1.),(1.,1.),(1.,1.),(1.,1.),(1.,1.),(1.,1.),(1.,
1.),(1.,1.),(1.,1.),(1.,1.),(1.,1.),(1.,1.),(1.,1.),(1.,1.),(1.,1.),(1.,
1.),(1.,1.),(1.,1.),(1.,1.),(1.,1.),(1.,1.),(1.,1.),(1.,1.),(1.,1.),(1.,
1.),(1.,1.)))
REPRESENTATION_ITEM('')
SURFACE()
);
#16=(
BOUNDED_SURFACE()
B_SPLINE_SURFACE(5,1,((#22223,#22224),(#22225,#22226),(#22227,#22228),(#22229,
#22230),(#22231,#22232),(#22233,#22234),(#22235,#22236),(#22237,#22238),
(#22239,#22240),(#22241,#22242),(#22243,#22244),(#22245,#22246),(#22247,
#22248),(#22249,#22250),(#22251,#22252),(#22253,#22254),(#22255,#22256),
(#22257,#22258),(#22259,#22260),(#22261,#22262),(#22263,#22264),(#22265,
#22266),(#22267,#22268),(#22269,#22270),(#22271,#22272),(#22273,#22274),
(#22275,#22276),(#22277,#22278),(#22279,#22280),(#22281,#22282),(#22283,
#22284),(#22285,#22286),(#22287,#22288),(#22289,#22290),(#22291,#22292),
(#22293,#22294),(#22295,#22296),(#22297,#22298),(#22299,#22300),(#22301,
#22302),(#22303,#22304),(#22305,#22306),(#22307,#22308),(#22309,#22310),
(#22311,#22312),(#22313,#22314),(#22315,#22316),(#22317,#22318),(#22319,
#22320),(#22321,#22322),(#22323,#22324),(#22325,#22326),(#22327,#22328),
(#22329,#22330),(#22331,#22332),(#22333,#22334),(#22335,#22336),(#22337,
#22338),(#22339,#22340),(#22341,#22342),(#22343,#22344),(#22345,#22346),
(#22347,#22348),(#22349,#22350),(#22351,#22352),(#22353,#22354),(#22355,
#22356),(#22357,#22358),(#22359,#22360),(#22361,#22362)),.UNSPECIFIED.,
 .F.,.F.,.F.)
B_SPLINE_SURFACE_WITH_KNOTS((6,1,1,1,1,1,1,1,1,1,1,1,1,1,1,1,1,1,1,1,1,
1,1,1,1,1,1,1,1,1,1,1,1,1,1,1,1,1,1,1,1,1,1,1,1,1,1,1,1,1,1,1,1,1,1,1,1,
1,1,1,1,1,1,1,1,6),(2,2),(-1.,-0.984615384615383,-0.969230769230768,-0.953846153846152,
-0.938461538461537,-0.923076923076922,-0.907692307692306,-0.892307692307691,
-0.876923076923076,-0.86153846153846,-0.846153846153845,-0.83076923076923,
-0.815384615384614,-0.799999999999999,-0.784615384615384,-0.769230769230768,
-0.753846153846153,-0.738461538461538,-0.723076923076922,-0.707692307692307,
-0.692307692307692,-0.676923076923076,-0.661538461538461,-0.646153846153846,
-0.63076923076923,-0.615384615384615,-0.6,-0.584615384615384,-0.569230769230769,
-0.553846153846154,-0.538461538461538,-0.523076923076923,-0.507692307692308,
-0.492307692307692,-0.476923076923077,-0.461538461538462,-0.446153846153846,
-0.430769230769231,-0.415384615384615,-0.4,-0.384615384615385,-0.369230769230769,
-0.353846153846154,-0.338461538461538,-0.323076923076923,-0.307692307692308,
-0.292307692307692,-0.276923076923077,-0.261538461538462,-0.246153846153846,
-0.230769230769231,-0.215384615384615,-0.2,-0.184615384615385,-0.169230769230769,
-0.153846153846154,-0.138461538461538,-0.123076923076923,-0.107692307692308,
-0.0923076923076923,-0.0769230769230769,-0.0615384615384615,-0.0461538461538462,
-0.0307692307692308,-0.0153846153846154,0.),(-1.,1.),.UNSPECIFIED.)
GEOMETRIC_REPRESENTATION_ITEM()
RATIONAL_B_SPLINE_SURFACE(((1.,1.),(1.,1.),(1.,1.),(1.,1.),(1.,1.),(1.,
1.),(1.,1.),(1.,1.),(1.,1.),(1.,1.),(1.,1.),(1.,1.),(1.,1.),(1.,1.),(1.,
1.),(1.,1.),(1.,1.),(1.,1.),(1.,1.),(1.,1.),(1.,1.),(1.,1.),(1.,1.),(1.,
1.),(1.,1.),(1.,1.),(1.,1.),(1.,1.),(1.,1.),(1.,1.),(1.,1.),(1.,1.),(1.,
1.),(1.,1.),(1.,1.),(1.,1.),(1.,1.),(1.,1.),(1.,1.),(1.,1.),(1.,1.),(1.,
1.),(1.,1.),(1.,1.),(1.,1.),(1.,1.),(1.,1.),(1.,1.),(1.,1.),(1.,1.),(1.,
1.),(1.,1.),(1.,1.),(1.,1.),(1.,1.),(1.,1.),(1.,1.),(1.,1.),(1.,1.),(1.,
1.),(1.,1.),(1.,1.),(1.,1.),(1.,1.),(1.,1.),(1.,1.),(1.,1.),(1.,1.),(1.,
1.),(1.,1.)))
REPRESENTATION_ITEM('')
SURFACE()
);
#17=(
BOUNDED_SURFACE()
B_SPLINE_SURFACE(5,1,((#22439,#22440),(#22441,#22442),(#22443,#22444),(#22445,
#22446),(#22447,#22448),(#22449,#22450),(#22451,#22452),(#22453,#22454),
(#22455,#22456),(#22457,#22458),(#22459,#22460),(#22461,#22462),(#22463,
#22464),(#22465,#22466),(#22467,#22468),(#22469,#22470),(#22471,#22472),
(#22473,#22474),(#22475,#22476),(#22477,#22478),(#22479,#22480),(#22481,
#22482),(#22483,#22484),(#22485,#22486),(#22487,#22488),(#22489,#22490),
(#22491,#22492),(#22493,#22494),(#22495,#22496),(#22497,#22498),(#22499,
#22500),(#22501,#22502),(#22503,#22504),(#22505,#22506),(#22507,#22508),
(#22509,#22510),(#22511,#22512),(#22513,#22514),(#22515,#22516),(#22517,
#22518),(#22519,#22520),(#22521,#22522),(#22523,#22524),(#22525,#22526),
(#22527,#22528),(#22529,#22530),(#22531,#22532),(#22533,#22534),(#22535,
#22536),(#22537,#22538),(#22539,#22540),(#22541,#22542),(#22543,#22544),
(#22545,#22546),(#22547,#22548),(#22549,#22550),(#22551,#22552),(#22553,
#22554),(#22555,#22556),(#22557,#22558),(#22559,#22560),(#22561,#22562),
(#22563,#22564),(#22565,#22566),(#22567,#22568),(#22569,#22570),(#22571,
#22572),(#22573,#22574),(#22575,#22576),(#22577,#22578)),.UNSPECIFIED.,
 .F.,.F.,.F.)
B_SPLINE_SURFACE_WITH_KNOTS((6,1,1,1,1,1,1,1,1,1,1,1,1,1,1,1,1,1,1,1,1,
1,1,1,1,1,1,1,1,1,1,1,1,1,1,1,1,1,1,1,1,1,1,1,1,1,1,1,1,1,1,1,1,1,1,1,1,
1,1,1,1,1,1,1,1,6),(2,2),(-1.,-0.984615384615383,-0.969230769230768,-0.953846153846152,
-0.938461538461537,-0.923076923076922,-0.907692307692306,-0.892307692307691,
-0.876923076923076,-0.86153846153846,-0.846153846153845,-0.83076923076923,
-0.815384615384614,-0.799999999999999,-0.784615384615384,-0.769230769230768,
-0.753846153846153,-0.738461538461538,-0.723076923076922,-0.707692307692307,
-0.692307692307692,-0.676923076923076,-0.661538461538461,-0.646153846153846,
-0.63076923076923,-0.615384615384615,-0.6,-0.584615384615384,-0.569230769230769,
-0.553846153846154,-0.538461538461538,-0.523076923076923,-0.507692307692308,
-0.492307692307692,-0.476923076923077,-0.461538461538462,-0.446153846153846,
-0.430769230769231,-0.415384615384615,-0.4,-0.384615384615385,-0.369230769230769,
-0.353846153846154,-0.338461538461538,-0.323076923076923,-0.307692307692308,
-0.292307692307692,-0.276923076923077,-0.261538461538462,-0.246153846153846,
-0.230769230769231,-0.215384615384615,-0.2,-0.184615384615385,-0.169230769230769,
-0.153846153846154,-0.138461538461538,-0.123076923076923,-0.107692307692308,
-0.0923076923076923,-0.0769230769230769,-0.0615384615384615,-0.0461538461538462,
-0.0307692307692308,-0.0153846153846154,0.),(-1.,1.),.UNSPECIFIED.)
GEOMETRIC_REPRESENTATION_ITEM()
RATIONAL_B_SPLINE_SURFACE(((1.,1.),(1.,1.),(1.,1.),(1.,1.),(1.,1.),(1.,
1.),(1.,1.),(1.,1.),(1.,1.),(1.,1.),(1.,1.),(1.,1.),(1.,1.),(1.,1.),(1.,
1.),(1.,1.),(1.,1.),(1.,1.),(1.,1.),(1.,1.),(1.,1.),(1.,1.),(1.,1.),(1.,
1.),(1.,1.),(1.,1.),(1.,1.),(1.,1.),(1.,1.),(1.,1.),(1.,1.),(1.,1.),(1.,
1.),(1.,1.),(1.,1.),(1.,1.),(1.,1.),(1.,1.),(1.,1.),(1.,1.),(1.,1.),(1.,
1.),(1.,1.),(1.,1.),(1.,1.),(1.,1.),(1.,1.),(1.,1.),(1.,1.),(1.,1.),(1.,
1.),(1.,1.),(1.,1.),(1.,1.),(1.,1.),(1.,1.),(1.,1.),(1.,1.),(1.,1.),(1.,
1.),(1.,1.),(1.,1.),(1.,1.),(1.,1.),(1.,1.),(1.,1.),(1.,1.),(1.,1.),(1.,
1.),(1.,1.)))
REPRESENTATION_ITEM('')
SURFACE()
);
#18=(
BOUNDED_SURFACE()
B_SPLINE_SURFACE(5,1,((#22655,#22656),(#22657,#22658),(#22659,#22660),(#22661,
#22662),(#22663,#22664),(#22665,#22666),(#22667,#22668),(#22669,#22670),
(#22671,#22672),(#22673,#22674),(#22675,#22676),(#22677,#22678),(#22679,
#22680),(#22681,#22682),(#22683,#22684),(#22685,#22686),(#22687,#22688),
(#22689,#22690),(#22691,#22692),(#22693,#22694),(#22695,#22696),(#22697,
#22698),(#22699,#22700),(#22701,#22702),(#22703,#22704),(#22705,#22706),
(#22707,#22708),(#22709,#22710),(#22711,#22712),(#22713,#22714),(#22715,
#22716),(#22717,#22718),(#22719,#22720),(#22721,#22722),(#22723,#22724),
(#22725,#22726),(#22727,#22728),(#22729,#22730),(#22731,#22732),(#22733,
#22734),(#22735,#22736),(#22737,#22738),(#22739,#22740),(#22741,#22742),
(#22743,#22744),(#22745,#22746),(#22747,#22748),(#22749,#22750),(#22751,
#22752),(#22753,#22754),(#22755,#22756),(#22757,#22758),(#22759,#22760),
(#22761,#22762),(#22763,#22764),(#22765,#22766),(#22767,#22768),(#22769,
#22770),(#22771,#22772),(#22773,#22774),(#22775,#22776),(#22777,#22778),
(#22779,#22780),(#22781,#22782),(#22783,#22784),(#22785,#22786),(#22787,
#22788),(#22789,#22790),(#22791,#22792),(#22793,#22794)),.UNSPECIFIED.,
 .F.,.F.,.F.)
B_SPLINE_SURFACE_WITH_KNOTS((6,1,1,1,1,1,1,1,1,1,1,1,1,1,1,1,1,1,1,1,1,
1,1,1,1,1,1,1,1,1,1,1,1,1,1,1,1,1,1,1,1,1,1,1,1,1,1,1,1,1,1,1,1,1,1,1,1,
1,1,1,1,1,1,1,1,6),(2,2),(-1.,-0.984615384615383,-0.969230769230768,-0.953846153846152,
-0.938461538461537,-0.923076923076922,-0.907692307692306,-0.892307692307691,
-0.876923076923076,-0.86153846153846,-0.846153846153845,-0.83076923076923,
-0.815384615384614,-0.799999999999999,-0.784615384615384,-0.769230769230768,
-0.753846153846153,-0.738461538461538,-0.723076923076922,-0.707692307692307,
-0.692307692307692,-0.676923076923076,-0.661538461538461,-0.646153846153846,
-0.63076923076923,-0.615384615384615,-0.6,-0.584615384615384,-0.569230769230769,
-0.553846153846154,-0.538461538461538,-0.523076923076923,-0.507692307692308,
-0.492307692307692,-0.476923076923077,-0.461538461538462,-0.446153846153846,
-0.430769230769231,-0.415384615384615,-0.4,-0.384615384615385,-0.369230769230769,
-0.353846153846154,-0.338461538461538,-0.323076923076923,-0.307692307692308,
-0.292307692307692,-0.276923076923077,-0.261538461538462,-0.246153846153846,
-0.230769230769231,-0.215384615384615,-0.2,-0.184615384615385,-0.169230769230769,
-0.153846153846154,-0.138461538461538,-0.123076923076923,-0.107692307692308,
-0.0923076923076923,-0.0769230769230769,-0.0615384615384615,-0.0461538461538462,
-0.0307692307692308,-0.0153846153846154,0.),(-1.,1.),.UNSPECIFIED.)
GEOMETRIC_REPRESENTATION_ITEM()
RATIONAL_B_SPLINE_SURFACE(((1.,1.),(1.,1.),(1.,1.),(1.,1.),(1.,1.),(1.,
1.),(1.,1.),(1.,1.),(1.,1.),(1.,1.),(1.,1.),(1.,1.),(1.,1.),(1.,1.),(1.,
1.),(1.,1.),(1.,1.),(1.,1.),(1.,1.),(1.,1.),(1.,1.),(1.,1.),(1.,1.),(1.,
1.),(1.,1.),(1.,1.),(1.,1.),(1.,1.),(1.,1.),(1.,1.),(1.,1.),(1.,1.),(1.,
1.),(1.,1.),(1.,1.),(1.,1.),(1.,1.),(1.,1.),(1.,1.),(1.,1.),(1.,1.),(1.,
1.),(1.,1.),(1.,1.),(1.,1.),(1.,1.),(1.,1.),(1.,1.),(1.,1.),(1.,1.),(1.,
1.),(1.,1.),(1.,1.),(1.,1.),(1.,1.),(1.,1.),(1.,1.),(1.,1.),(1.,1.),(1.,
1.),(1.,1.),(1.,1.),(1.,1.),(1.,1.),(1.,1.),(1.,1.),(1.,1.),(1.,1.),(1.,
1.),(1.,1.)))
REPRESENTATION_ITEM('')
SURFACE()
);
#19=(
BOUNDED_SURFACE()
B_SPLINE_SURFACE(5,1,((#22871,#22872),(#22873,#22874),(#22875,#22876),(#22877,
#22878),(#22879,#22880),(#22881,#22882),(#22883,#22884),(#22885,#22886),
(#22887,#22888),(#22889,#22890),(#22891,#22892),(#22893,#22894),(#22895,
#22896),(#22897,#22898),(#22899,#22900),(#22901,#22902),(#22903,#22904),
(#22905,#22906),(#22907,#22908),(#22909,#22910),(#22911,#22912),(#22913,
#22914),(#22915,#22916),(#22917,#22918),(#22919,#22920),(#22921,#22922),
(#22923,#22924),(#22925,#22926),(#22927,#22928),(#22929,#22930),(#22931,
#22932),(#22933,#22934),(#22935,#22936),(#22937,#22938),(#22939,#22940),
(#22941,#22942),(#22943,#22944),(#22945,#22946),(#22947,#22948),(#22949,
#22950),(#22951,#22952),(#22953,#22954),(#22955,#22956),(#22957,#22958),
(#22959,#22960),(#22961,#22962),(#22963,#22964),(#22965,#22966),(#22967,
#22968),(#22969,#22970),(#22971,#22972),(#22973,#22974),(#22975,#22976),
(#22977,#22978),(#22979,#22980),(#22981,#22982),(#22983,#22984),(#22985,
#22986),(#22987,#22988),(#22989,#22990),(#22991,#22992),(#22993,#22994),
(#22995,#22996),(#22997,#22998),(#22999,#23000),(#23001,#23002),(#23003,
#23004),(#23005,#23006),(#23007,#23008),(#23009,#23010)),.UNSPECIFIED.,
 .F.,.F.,.F.)
B_SPLINE_SURFACE_WITH_KNOTS((6,1,1,1,1,1,1,1,1,1,1,1,1,1,1,1,1,1,1,1,1,
1,1,1,1,1,1,1,1,1,1,1,1,1,1,1,1,1,1,1,1,1,1,1,1,1,1,1,1,1,1,1,1,1,1,1,1,
1,1,1,1,1,1,1,1,6),(2,2),(-1.,-0.984615384615383,-0.969230769230768,-0.953846153846152,
-0.938461538461537,-0.923076923076922,-0.907692307692306,-0.892307692307691,
-0.876923076923076,-0.86153846153846,-0.846153846153845,-0.83076923076923,
-0.815384615384614,-0.799999999999999,-0.784615384615384,-0.769230769230768,
-0.753846153846153,-0.738461538461538,-0.723076923076922,-0.707692307692307,
-0.692307692307692,-0.676923076923076,-0.661538461538461,-0.646153846153846,
-0.63076923076923,-0.615384615384615,-0.6,-0.584615384615384,-0.569230769230769,
-0.553846153846154,-0.538461538461538,-0.523076923076923,-0.507692307692308,
-0.492307692307692,-0.476923076923077,-0.461538461538462,-0.446153846153846,
-0.430769230769231,-0.415384615384615,-0.4,-0.384615384615385,-0.369230769230769,
-0.353846153846154,-0.338461538461538,-0.323076923076923,-0.307692307692308,
-0.292307692307692,-0.276923076923077,-0.261538461538462,-0.246153846153846,
-0.230769230769231,-0.215384615384615,-0.2,-0.184615384615385,-0.169230769230769,
-0.153846153846154,-0.138461538461538,-0.123076923076923,-0.107692307692308,
-0.0923076923076923,-0.0769230769230769,-0.0615384615384615,-0.0461538461538462,
-0.0307692307692308,-0.0153846153846154,0.),(-1.,1.),.UNSPECIFIED.)
GEOMETRIC_REPRESENTATION_ITEM()
RATIONAL_B_SPLINE_SURFACE(((1.,1.),(1.,1.),(1.,1.),(1.,1.),(1.,1.),(1.,
1.),(1.,1.),(1.,1.),(1.,1.),(1.,1.),(1.,1.),(1.,1.),(1.,1.),(1.,1.),(1.,
1.),(1.,1.),(1.,1.),(1.,1.),(1.,1.),(1.,1.),(1.,1.),(1.,1.),(1.,1.),(1.,
1.),(1.,1.),(1.,1.),(1.,1.),(1.,1.),(1.,1.),(1.,1.),(1.,1.),(1.,1.),(1.,
1.),(1.,1.),(1.,1.),(1.,1.),(1.,1.),(1.,1.),(1.,1.),(1.,1.),(1.,1.),(1.,
1.),(1.,1.),(1.,1.),(1.,1.),(1.,1.),(1.,1.),(1.,1.),(1.,1.),(1.,1.),(1.,
1.),(1.,1.),(1.,1.),(1.,1.),(1.,1.),(1.,1.),(1.,1.),(1.,1.),(1.,1.),(1.,
1.),(1.,1.),(1.,1.),(1.,1.),(1.,1.),(1.,1.),(1.,1.),(1.,1.),(1.,1.),(1.,
1.),(1.,1.)))
REPRESENTATION_ITEM('')
SURFACE()
);
#20=(
BOUNDED_SURFACE()
B_SPLINE_SURFACE(5,1,((#23087,#23088),(#23089,#23090),(#23091,#23092),(#23093,
#23094),(#23095,#23096),(#23097,#23098),(#23099,#23100),(#23101,#23102),
(#23103,#23104),(#23105,#23106),(#23107,#23108),(#23109,#23110),(#23111,
#23112),(#23113,#23114),(#23115,#23116),(#23117,#23118),(#23119,#23120),
(#23121,#23122),(#23123,#23124),(#23125,#23126),(#23127,#23128),(#23129,
#23130),(#23131,#23132),(#23133,#23134),(#23135,#23136),(#23137,#23138),
(#23139,#23140),(#23141,#23142),(#23143,#23144),(#23145,#23146),(#23147,
#23148),(#23149,#23150),(#23151,#23152),(#23153,#23154),(#23155,#23156),
(#23157,#23158),(#23159,#23160),(#23161,#23162),(#23163,#23164),(#23165,
#23166),(#23167,#23168),(#23169,#23170),(#23171,#23172),(#23173,#23174),
(#23175,#23176),(#23177,#23178),(#23179,#23180),(#23181,#23182),(#23183,
#23184),(#23185,#23186),(#23187,#23188),(#23189,#23190),(#23191,#23192),
(#23193,#23194),(#23195,#23196),(#23197,#23198),(#23199,#23200),(#23201,
#23202),(#23203,#23204),(#23205,#23206),(#23207,#23208),(#23209,#23210),
(#23211,#23212),(#23213,#23214),(#23215,#23216),(#23217,#23218),(#23219,
#23220),(#23221,#23222),(#23223,#23224),(#23225,#23226)),.UNSPECIFIED.,
 .F.,.F.,.F.)
B_SPLINE_SURFACE_WITH_KNOTS((6,1,1,1,1,1,1,1,1,1,1,1,1,1,1,1,1,1,1,1,1,
1,1,1,1,1,1,1,1,1,1,1,1,1,1,1,1,1,1,1,1,1,1,1,1,1,1,1,1,1,1,1,1,1,1,1,1,
1,1,1,1,1,1,1,1,6),(2,2),(-1.,-0.984615384615383,-0.969230769230768,-0.953846153846152,
-0.938461538461537,-0.923076923076922,-0.907692307692306,-0.892307692307691,
-0.876923076923076,-0.86153846153846,-0.846153846153845,-0.83076923076923,
-0.815384615384614,-0.799999999999999,-0.784615384615384,-0.769230769230768,
-0.753846153846153,-0.738461538461538,-0.723076923076922,-0.707692307692307,
-0.692307692307692,-0.676923076923076,-0.661538461538461,-0.646153846153846,
-0.63076923076923,-0.615384615384615,-0.6,-0.584615384615384,-0.569230769230769,
-0.553846153846154,-0.538461538461538,-0.523076923076923,-0.507692307692308,
-0.492307692307692,-0.476923076923077,-0.461538461538462,-0.446153846153846,
-0.430769230769231,-0.415384615384615,-0.4,-0.384615384615385,-0.369230769230769,
-0.353846153846154,-0.338461538461538,-0.323076923076923,-0.307692307692308,
-0.292307692307692,-0.276923076923077,-0.261538461538462,-0.246153846153846,
-0.230769230769231,-0.215384615384615,-0.2,-0.184615384615385,-0.169230769230769,
-0.153846153846154,-0.138461538461538,-0.123076923076923,-0.107692307692308,
-0.0923076923076923,-0.0769230769230769,-0.0615384615384615,-0.0461538461538462,
-0.0307692307692308,-0.0153846153846154,0.),(-1.,1.),.UNSPECIFIED.)
GEOMETRIC_REPRESENTATION_ITEM()
RATIONAL_B_SPLINE_SURFACE(((1.,1.),(1.,1.),(1.,1.),(1.,1.),(1.,1.),(1.,
1.),(1.,1.),(1.,1.),(1.,1.),(1.,1.),(1.,1.),(1.,1.),(1.,1.),(1.,1.),(1.,
1.),(1.,1.),(1.,1.),(1.,1.),(1.,1.),(1.,1.),(1.,1.),(1.,1.),(1.,1.),(1.,
1.),(1.,1.),(1.,1.),(1.,1.),(1.,1.),(1.,1.),(1.,1.),(1.,1.),(1.,1.),(1.,
1.),(1.,1.),(1.,1.),(1.,1.),(1.,1.),(1.,1.),(1.,1.),(1.,1.),(1.,1.),(1.,
1.),(1.,1.),(1.,1.),(1.,1.),(1.,1.),(1.,1.),(1.,1.),(1.,1.),(1.,1.),(1.,
1.),(1.,1.),(1.,1.),(1.,1.),(1.,1.),(1.,1.),(1.,1.),(1.,1.),(1.,1.),(1.,
1.),(1.,1.),(1.,1.),(1.,1.),(1.,1.),(1.,1.),(1.,1.),(1.,1.),(1.,1.),(1.,
1.),(1.,1.)))
REPRESENTATION_ITEM('')
SURFACE()
);
#21=(
BOUNDED_SURFACE()
B_SPLINE_SURFACE(5,1,((#23303,#23304),(#23305,#23306),(#23307,#23308),(#23309,
#23310),(#23311,#23312),(#23313,#23314),(#23315,#23316),(#23317,#23318),
(#23319,#23320),(#23321,#23322),(#23323,#23324),(#23325,#23326),(#23327,
#23328),(#23329,#23330),(#23331,#23332),(#23333,#23334),(#23335,#23336),
(#23337,#23338),(#23339,#23340),(#23341,#23342),(#23343,#23344),(#23345,
#23346),(#23347,#23348),(#23349,#23350),(#23351,#23352),(#23353,#23354),
(#23355,#23356),(#23357,#23358),(#23359,#23360),(#23361,#23362),(#23363,
#23364),(#23365,#23366),(#23367,#23368),(#23369,#23370),(#23371,#23372),
(#23373,#23374),(#23375,#23376),(#23377,#23378),(#23379,#23380),(#23381,
#23382),(#23383,#23384),(#23385,#23386),(#23387,#23388),(#23389,#23390),
(#23391,#23392),(#23393,#23394),(#23395,#23396),(#23397,#23398),(#23399,
#23400),(#23401,#23402),(#23403,#23404),(#23405,#23406),(#23407,#23408),
(#23409,#23410),(#23411,#23412),(#23413,#23414),(#23415,#23416),(#23417,
#23418),(#23419,#23420),(#23421,#23422),(#23423,#23424),(#23425,#23426),
(#23427,#23428),(#23429,#23430),(#23431,#23432),(#23433,#23434),(#23435,
#23436),(#23437,#23438),(#23439,#23440),(#23441,#23442)),.UNSPECIFIED.,
 .F.,.F.,.F.)
B_SPLINE_SURFACE_WITH_KNOTS((6,1,1,1,1,1,1,1,1,1,1,1,1,1,1,1,1,1,1,1,1,
1,1,1,1,1,1,1,1,1,1,1,1,1,1,1,1,1,1,1,1,1,1,1,1,1,1,1,1,1,1,1,1,1,1,1,1,
1,1,1,1,1,1,1,1,6),(2,2),(-1.,-0.984615384615383,-0.969230769230768,-0.953846153846152,
-0.938461538461537,-0.923076923076922,-0.907692307692306,-0.892307692307691,
-0.876923076923076,-0.86153846153846,-0.846153846153845,-0.83076923076923,
-0.815384615384614,-0.799999999999999,-0.784615384615384,-0.769230769230768,
-0.753846153846153,-0.738461538461538,-0.723076923076922,-0.707692307692307,
-0.692307692307692,-0.676923076923076,-0.661538461538461,-0.646153846153846,
-0.63076923076923,-0.615384615384615,-0.6,-0.584615384615384,-0.569230769230769,
-0.553846153846154,-0.538461538461538,-0.523076923076923,-0.507692307692308,
-0.492307692307692,-0.476923076923077,-0.461538461538462,-0.446153846153846,
-0.430769230769231,-0.415384615384615,-0.4,-0.384615384615385,-0.369230769230769,
-0.353846153846154,-0.338461538461538,-0.323076923076923,-0.307692307692308,
-0.292307692307692,-0.276923076923077,-0.261538461538462,-0.246153846153846,
-0.230769230769231,-0.215384615384615,-0.2,-0.184615384615385,-0.169230769230769,
-0.153846153846154,-0.138461538461538,-0.123076923076923,-0.107692307692308,
-0.0923076923076923,-0.0769230769230769,-0.0615384615384615,-0.0461538461538462,
-0.0307692307692308,-0.0153846153846154,0.),(-1.,1.),.UNSPECIFIED.)
GEOMETRIC_REPRESENTATION_ITEM()
RATIONAL_B_SPLINE_SURFACE(((1.,1.),(1.,1.),(1.,1.),(1.,1.),(1.,1.),(1.,
1.),(1.,1.),(1.,1.),(1.,1.),(1.,1.),(1.,1.),(1.,1.),(1.,1.),(1.,1.),(1.,
1.),(1.,1.),(1.,1.),(1.,1.),(1.,1.),(1.,1.),(1.,1.),(1.,1.),(1.,1.),(1.,
1.),(1.,1.),(1.,1.),(1.,1.),(1.,1.),(1.,1.),(1.,1.),(1.,1.),(1.,1.),(1.,
1.),(1.,1.),(1.,1.),(1.,1.),(1.,1.),(1.,1.),(1.,1.),(1.,1.),(1.,1.),(1.,
1.),(1.,1.),(1.,1.),(1.,1.),(1.,1.),(1.,1.),(1.,1.),(1.,1.),(1.,1.),(1.,
1.),(1.,1.),(1.,1.),(1.,1.),(1.,1.),(1.,1.),(1.,1.),(1.,1.),(1.,1.),(1.,
1.),(1.,1.),(1.,1.),(1.,1.),(1.,1.),(1.,1.),(1.,1.),(1.,1.),(1.,1.),(1.,
1.),(1.,1.)))
REPRESENTATION_ITEM('')
SURFACE()
);
#22=(
BOUNDED_SURFACE()
B_SPLINE_SURFACE(5,1,((#23519,#23520),(#23521,#23522),(#23523,#23524),(#23525,
#23526),(#23527,#23528),(#23529,#23530),(#23531,#23532),(#23533,#23534),
(#23535,#23536),(#23537,#23538),(#23539,#23540),(#23541,#23542),(#23543,
#23544),(#23545,#23546),(#23547,#23548),(#23549,#23550),(#23551,#23552),
(#23553,#23554),(#23555,#23556),(#23557,#23558),(#23559,#23560),(#23561,
#23562),(#23563,#23564),(#23565,#23566),(#23567,#23568),(#23569,#23570),
(#23571,#23572),(#23573,#23574),(#23575,#23576),(#23577,#23578),(#23579,
#23580),(#23581,#23582),(#23583,#23584),(#23585,#23586),(#23587,#23588),
(#23589,#23590),(#23591,#23592),(#23593,#23594),(#23595,#23596),(#23597,
#23598),(#23599,#23600),(#23601,#23602),(#23603,#23604),(#23605,#23606),
(#23607,#23608),(#23609,#23610),(#23611,#23612),(#23613,#23614),(#23615,
#23616),(#23617,#23618),(#23619,#23620),(#23621,#23622),(#23623,#23624),
(#23625,#23626),(#23627,#23628),(#23629,#23630),(#23631,#23632),(#23633,
#23634),(#23635,#23636),(#23637,#23638),(#23639,#23640),(#23641,#23642),
(#23643,#23644),(#23645,#23646),(#23647,#23648),(#23649,#23650),(#23651,
#23652),(#23653,#23654),(#23655,#23656),(#23657,#23658)),.UNSPECIFIED.,
 .F.,.F.,.F.)
B_SPLINE_SURFACE_WITH_KNOTS((6,1,1,1,1,1,1,1,1,1,1,1,1,1,1,1,1,1,1,1,1,
1,1,1,1,1,1,1,1,1,1,1,1,1,1,1,1,1,1,1,1,1,1,1,1,1,1,1,1,1,1,1,1,1,1,1,1,
1,1,1,1,1,1,1,1,6),(2,2),(-1.,-0.984615384615383,-0.969230769230768,-0.953846153846152,
-0.938461538461537,-0.923076923076922,-0.907692307692306,-0.892307692307691,
-0.876923076923076,-0.86153846153846,-0.846153846153845,-0.83076923076923,
-0.815384615384614,-0.799999999999999,-0.784615384615384,-0.769230769230768,
-0.753846153846153,-0.738461538461538,-0.723076923076922,-0.707692307692307,
-0.692307692307692,-0.676923076923076,-0.661538461538461,-0.646153846153846,
-0.63076923076923,-0.615384615384615,-0.6,-0.584615384615384,-0.569230769230769,
-0.553846153846154,-0.538461538461538,-0.523076923076923,-0.507692307692308,
-0.492307692307692,-0.476923076923077,-0.461538461538462,-0.446153846153846,
-0.430769230769231,-0.415384615384615,-0.4,-0.384615384615385,-0.369230769230769,
-0.353846153846154,-0.338461538461538,-0.323076923076923,-0.307692307692308,
-0.292307692307692,-0.276923076923077,-0.261538461538462,-0.246153846153846,
-0.230769230769231,-0.215384615384615,-0.2,-0.184615384615385,-0.169230769230769,
-0.153846153846154,-0.138461538461538,-0.123076923076923,-0.107692307692308,
-0.0923076923076923,-0.0769230769230769,-0.0615384615384615,-0.0461538461538462,
-0.0307692307692308,-0.0153846153846154,0.),(-1.,1.),.UNSPECIFIED.)
GEOMETRIC_REPRESENTATION_ITEM()
RATIONAL_B_SPLINE_SURFACE(((1.,1.),(1.,1.),(1.,1.),(1.,1.),(1.,1.),(1.,
1.),(1.,1.),(1.,1.),(1.,1.),(1.,1.),(1.,1.),(1.,1.),(1.,1.),(1.,1.),(1.,
1.),(1.,1.),(1.,1.),(1.,1.),(1.,1.),(1.,1.),(1.,1.),(1.,1.),(1.,1.),(1.,
1.),(1.,1.),(1.,1.),(1.,1.),(1.,1.),(1.,1.),(1.,1.),(1.,1.),(1.,1.),(1.,
1.),(1.,1.),(1.,1.),(1.,1.),(1.,1.),(1.,1.),(1.,1.),(1.,1.),(1.,1.),(1.,
1.),(1.,1.),(1.,1.),(1.,1.),(1.,1.),(1.,1.),(1.,1.),(1.,1.),(1.,1.),(1.,
1.),(1.,1.),(1.,1.),(1.,1.),(1.,1.),(1.,1.),(1.,1.),(1.,1.),(1.,1.),(1.,
1.),(1.,1.),(1.,1.),(1.,1.),(1.,1.),(1.,1.),(1.,1.),(1.,1.),(1.,1.),(1.,
1.),(1.,1.)))
REPRESENTATION_ITEM('')
SURFACE()
);
#23=(
BOUNDED_SURFACE()
B_SPLINE_SURFACE(5,1,((#23735,#23736),(#23737,#23738),(#23739,#23740),(#23741,
#23742),(#23743,#23744),(#23745,#23746),(#23747,#23748),(#23749,#23750),
(#23751,#23752),(#23753,#23754),(#23755,#23756),(#23757,#23758),(#23759,
#23760),(#23761,#23762),(#23763,#23764),(#23765,#23766),(#23767,#23768),
(#23769,#23770),(#23771,#23772),(#23773,#23774),(#23775,#23776),(#23777,
#23778),(#23779,#23780),(#23781,#23782),(#23783,#23784),(#23785,#23786),
(#23787,#23788),(#23789,#23790),(#23791,#23792),(#23793,#23794),(#23795,
#23796),(#23797,#23798),(#23799,#23800),(#23801,#23802),(#23803,#23804),
(#23805,#23806),(#23807,#23808),(#23809,#23810),(#23811,#23812),(#23813,
#23814),(#23815,#23816),(#23817,#23818),(#23819,#23820),(#23821,#23822),
(#23823,#23824),(#23825,#23826),(#23827,#23828),(#23829,#23830),(#23831,
#23832),(#23833,#23834),(#23835,#23836),(#23837,#23838),(#23839,#23840),
(#23841,#23842),(#23843,#23844),(#23845,#23846),(#23847,#23848),(#23849,
#23850),(#23851,#23852),(#23853,#23854),(#23855,#23856),(#23857,#23858),
(#23859,#23860),(#23861,#23862),(#23863,#23864),(#23865,#23866),(#23867,
#23868),(#23869,#23870),(#23871,#23872),(#23873,#23874)),.UNSPECIFIED.,
 .F.,.F.,.F.)
B_SPLINE_SURFACE_WITH_KNOTS((6,1,1,1,1,1,1,1,1,1,1,1,1,1,1,1,1,1,1,1,1,
1,1,1,1,1,1,1,1,1,1,1,1,1,1,1,1,1,1,1,1,1,1,1,1,1,1,1,1,1,1,1,1,1,1,1,1,
1,1,1,1,1,1,1,1,6),(2,2),(-1.,-0.984615384615383,-0.969230769230768,-0.953846153846152,
-0.938461538461537,-0.923076923076922,-0.907692307692306,-0.892307692307691,
-0.876923076923076,-0.86153846153846,-0.846153846153845,-0.83076923076923,
-0.815384615384614,-0.799999999999999,-0.784615384615384,-0.769230769230768,
-0.753846153846153,-0.738461538461538,-0.723076923076922,-0.707692307692307,
-0.692307692307692,-0.676923076923076,-0.661538461538461,-0.646153846153846,
-0.63076923076923,-0.615384615384615,-0.6,-0.584615384615384,-0.569230769230769,
-0.553846153846154,-0.538461538461538,-0.523076923076923,-0.507692307692308,
-0.492307692307692,-0.476923076923077,-0.461538461538462,-0.446153846153846,
-0.430769230769231,-0.415384615384615,-0.4,-0.384615384615385,-0.369230769230769,
-0.353846153846154,-0.338461538461538,-0.323076923076923,-0.307692307692308,
-0.292307692307692,-0.276923076923077,-0.261538461538462,-0.246153846153846,
-0.230769230769231,-0.215384615384615,-0.2,-0.184615384615385,-0.169230769230769,
-0.153846153846154,-0.138461538461538,-0.123076923076923,-0.107692307692308,
-0.0923076923076923,-0.0769230769230769,-0.0615384615384615,-0.0461538461538462,
-0.0307692307692308,-0.0153846153846154,0.),(-1.,1.),.UNSPECIFIED.)
GEOMETRIC_REPRESENTATION_ITEM()
RATIONAL_B_SPLINE_SURFACE(((1.,1.),(1.,1.),(1.,1.),(1.,1.),(1.,1.),(1.,
1.),(1.,1.),(1.,1.),(1.,1.),(1.,1.),(1.,1.),(1.,1.),(1.,1.),(1.,1.),(1.,
1.),(1.,1.),(1.,1.),(1.,1.),(1.,1.),(1.,1.),(1.,1.),(1.,1.),(1.,1.),(1.,
1.),(1.,1.),(1.,1.),(1.,1.),(1.,1.),(1.,1.),(1.,1.),(1.,1.),(1.,1.),(1.,
1.),(1.,1.),(1.,1.),(1.,1.),(1.,1.),(1.,1.),(1.,1.),(1.,1.),(1.,1.),(1.,
1.),(1.,1.),(1.,1.),(1.,1.),(1.,1.),(1.,1.),(1.,1.),(1.,1.),(1.,1.),(1.,
1.),(1.,1.),(1.,1.),(1.,1.),(1.,1.),(1.,1.),(1.,1.),(1.,1.),(1.,1.),(1.,
1.),(1.,1.),(1.,1.),(1.,1.),(1.,1.),(1.,1.),(1.,1.),(1.,1.),(1.,1.),(1.,
1.),(1.,1.)))
REPRESENTATION_ITEM('')
SURFACE()
);
#24=(
BOUNDED_SURFACE()
B_SPLINE_SURFACE(5,1,((#23951,#23952),(#23953,#23954),(#23955,#23956),(#23957,
#23958),(#23959,#23960),(#23961,#23962),(#23963,#23964),(#23965,#23966),
(#23967,#23968),(#23969,#23970),(#23971,#23972),(#23973,#23974),(#23975,
#23976),(#23977,#23978),(#23979,#23980),(#23981,#23982),(#23983,#23984),
(#23985,#23986),(#23987,#23988),(#23989,#23990),(#23991,#23992),(#23993,
#23994),(#23995,#23996),(#23997,#23998),(#23999,#24000),(#24001,#24002),
(#24003,#24004),(#24005,#24006),(#24007,#24008),(#24009,#24010),(#24011,
#24012),(#24013,#24014),(#24015,#24016),(#24017,#24018),(#24019,#24020),
(#24021,#24022),(#24023,#24024),(#24025,#24026),(#24027,#24028),(#24029,
#24030),(#24031,#24032),(#24033,#24034),(#24035,#24036),(#24037,#24038),
(#24039,#24040),(#24041,#24042),(#24043,#24044),(#24045,#24046),(#24047,
#24048),(#24049,#24050),(#24051,#24052),(#24053,#24054),(#24055,#24056),
(#24057,#24058),(#24059,#24060),(#24061,#24062),(#24063,#24064),(#24065,
#24066),(#24067,#24068),(#24069,#24070),(#24071,#24072),(#24073,#24074),
(#24075,#24076),(#24077,#24078),(#24079,#24080),(#24081,#24082),(#24083,
#24084),(#24085,#24086),(#24087,#24088),(#24089,#24090)),.UNSPECIFIED.,
 .F.,.F.,.F.)
B_SPLINE_SURFACE_WITH_KNOTS((6,1,1,1,1,1,1,1,1,1,1,1,1,1,1,1,1,1,1,1,1,
1,1,1,1,1,1,1,1,1,1,1,1,1,1,1,1,1,1,1,1,1,1,1,1,1,1,1,1,1,1,1,1,1,1,1,1,
1,1,1,1,1,1,1,1,6),(2,2),(-1.,-0.984615384615383,-0.969230769230768,-0.953846153846152,
-0.938461538461537,-0.923076923076922,-0.907692307692306,-0.892307692307691,
-0.876923076923076,-0.86153846153846,-0.846153846153845,-0.83076923076923,
-0.815384615384614,-0.799999999999999,-0.784615384615384,-0.769230769230768,
-0.753846153846153,-0.738461538461538,-0.723076923076922,-0.707692307692307,
-0.692307692307692,-0.676923076923076,-0.661538461538461,-0.646153846153846,
-0.63076923076923,-0.615384615384615,-0.6,-0.584615384615384,-0.569230769230769,
-0.553846153846154,-0.538461538461538,-0.523076923076923,-0.507692307692308,
-0.492307692307692,-0.476923076923077,-0.461538461538462,-0.446153846153846,
-0.430769230769231,-0.415384615384615,-0.4,-0.384615384615385,-0.369230769230769,
-0.353846153846154,-0.338461538461538,-0.323076923076923,-0.307692307692308,
-0.292307692307692,-0.276923076923077,-0.261538461538462,-0.246153846153846,
-0.230769230769231,-0.215384615384615,-0.2,-0.184615384615385,-0.169230769230769,
-0.153846153846154,-0.138461538461538,-0.123076923076923,-0.107692307692308,
-0.0923076923076923,-0.0769230769230769,-0.0615384615384615,-0.0461538461538462,
-0.0307692307692308,-0.0153846153846154,0.),(-1.,1.),.UNSPECIFIED.)
GEOMETRIC_REPRESENTATION_ITEM()
RATIONAL_B_SPLINE_SURFACE(((1.,1.),(1.,1.),(1.,1.),(1.,1.),(1.,1.),(1.,
1.),(1.,1.),(1.,1.),(1.,1.),(1.,1.),(1.,1.),(1.,1.),(1.,1.),(1.,1.),(1.,
1.),(1.,1.),(1.,1.),(1.,1.),(1.,1.),(1.,1.),(1.,1.),(1.,1.),(1.,1.),(1.,
1.),(1.,1.),(1.,1.),(1.,1.),(1.,1.),(1.,1.),(1.,1.),(1.,1.),(1.,1.),(1.,
1.),(1.,1.),(1.,1.),(1.,1.),(1.,1.),(1.,1.),(1.,1.),(1.,1.),(1.,1.),(1.,
1.),(1.,1.),(1.,1.),(1.,1.),(1.,1.),(1.,1.),(1.,1.),(1.,1.),(1.,1.),(1.,
1.),(1.,1.),(1.,1.),(1.,1.),(1.,1.),(1.,1.),(1.,1.),(1.,1.),(1.,1.),(1.,
1.),(1.,1.),(1.,1.),(1.,1.),(1.,1.),(1.,1.),(1.,1.),(1.,1.),(1.,1.),(1.,
1.),(1.,1.)))
REPRESENTATION_ITEM('')
SURFACE()
);
#25=(
BOUNDED_SURFACE()
B_SPLINE_SURFACE(5,1,((#24167,#24168),(#24169,#24170),(#24171,#24172),(#24173,
#24174),(#24175,#24176),(#24177,#24178),(#24179,#24180),(#24181,#24182),
(#24183,#24184),(#24185,#24186),(#24187,#24188),(#24189,#24190),(#24191,
#24192),(#24193,#24194),(#24195,#24196),(#24197,#24198),(#24199,#24200),
(#24201,#24202),(#24203,#24204),(#24205,#24206),(#24207,#24208),(#24209,
#24210),(#24211,#24212),(#24213,#24214),(#24215,#24216),(#24217,#24218),
(#24219,#24220),(#24221,#24222),(#24223,#24224),(#24225,#24226),(#24227,
#24228),(#24229,#24230),(#24231,#24232),(#24233,#24234),(#24235,#24236),
(#24237,#24238),(#24239,#24240),(#24241,#24242),(#24243,#24244),(#24245,
#24246),(#24247,#24248),(#24249,#24250),(#24251,#24252),(#24253,#24254),
(#24255,#24256),(#24257,#24258),(#24259,#24260),(#24261,#24262),(#24263,
#24264),(#24265,#24266),(#24267,#24268),(#24269,#24270),(#24271,#24272),
(#24273,#24274),(#24275,#24276),(#24277,#24278),(#24279,#24280),(#24281,
#24282),(#24283,#24284),(#24285,#24286),(#24287,#24288),(#24289,#24290),
(#24291,#24292),(#24293,#24294),(#24295,#24296),(#24297,#24298),(#24299,
#24300),(#24301,#24302),(#24303,#24304),(#24305,#24306)),.UNSPECIFIED.,
 .F.,.F.,.F.)
B_SPLINE_SURFACE_WITH_KNOTS((6,1,1,1,1,1,1,1,1,1,1,1,1,1,1,1,1,1,1,1,1,
1,1,1,1,1,1,1,1,1,1,1,1,1,1,1,1,1,1,1,1,1,1,1,1,1,1,1,1,1,1,1,1,1,1,1,1,
1,1,1,1,1,1,1,1,6),(2,2),(-1.,-0.984615384615383,-0.969230769230768,-0.953846153846152,
-0.938461538461537,-0.923076923076922,-0.907692307692306,-0.892307692307691,
-0.876923076923076,-0.86153846153846,-0.846153846153845,-0.83076923076923,
-0.815384615384614,-0.799999999999999,-0.784615384615384,-0.769230769230768,
-0.753846153846153,-0.738461538461538,-0.723076923076922,-0.707692307692307,
-0.692307692307692,-0.676923076923076,-0.661538461538461,-0.646153846153846,
-0.63076923076923,-0.615384615384615,-0.6,-0.584615384615384,-0.569230769230769,
-0.553846153846154,-0.538461538461538,-0.523076923076923,-0.507692307692308,
-0.492307692307692,-0.476923076923077,-0.461538461538462,-0.446153846153846,
-0.430769230769231,-0.415384615384615,-0.4,-0.384615384615385,-0.369230769230769,
-0.353846153846154,-0.338461538461538,-0.323076923076923,-0.307692307692308,
-0.292307692307692,-0.276923076923077,-0.261538461538462,-0.246153846153846,
-0.230769230769231,-0.215384615384615,-0.2,-0.184615384615385,-0.169230769230769,
-0.153846153846154,-0.138461538461538,-0.123076923076923,-0.107692307692308,
-0.0923076923076923,-0.0769230769230769,-0.0615384615384615,-0.0461538461538462,
-0.0307692307692308,-0.0153846153846154,0.),(-1.,1.),.UNSPECIFIED.)
GEOMETRIC_REPRESENTATION_ITEM()
RATIONAL_B_SPLINE_SURFACE(((1.,1.),(1.,1.),(1.,1.),(1.,1.),(1.,1.),(1.,
1.),(1.,1.),(1.,1.),(1.,1.),(1.,1.),(1.,1.),(1.,1.),(1.,1.),(1.,1.),(1.,
1.),(1.,1.),(1.,1.),(1.,1.),(1.,1.),(1.,1.),(1.,1.),(1.,1.),(1.,1.),(1.,
1.),(1.,1.),(1.,1.),(1.,1.),(1.,1.),(1.,1.),(1.,1.),(1.,1.),(1.,1.),(1.,
1.),(1.,1.),(1.,1.),(1.,1.),(1.,1.),(1.,1.),(1.,1.),(1.,1.),(1.,1.),(1.,
1.),(1.,1.),(1.,1.),(1.,1.),(1.,1.),(1.,1.),(1.,1.),(1.,1.),(1.,1.),(1.,
1.),(1.,1.),(1.,1.),(1.,1.),(1.,1.),(1.,1.),(1.,1.),(1.,1.),(1.,1.),(1.,
1.),(1.,1.),(1.,1.),(1.,1.),(1.,1.),(1.,1.),(1.,1.),(1.,1.),(1.,1.),(1.,
1.),(1.,1.)))
REPRESENTATION_ITEM('')
SURFACE()
);
#26=(
BOUNDED_SURFACE()
B_SPLINE_SURFACE(5,1,((#24383,#24384),(#24385,#24386),(#24387,#24388),(#24389,
#24390),(#24391,#24392),(#24393,#24394),(#24395,#24396),(#24397,#24398),
(#24399,#24400),(#24401,#24402),(#24403,#24404),(#24405,#24406),(#24407,
#24408),(#24409,#24410),(#24411,#24412),(#24413,#24414),(#24415,#24416),
(#24417,#24418),(#24419,#24420),(#24421,#24422),(#24423,#24424),(#24425,
#24426),(#24427,#24428),(#24429,#24430),(#24431,#24432),(#24433,#24434),
(#24435,#24436),(#24437,#24438),(#24439,#24440),(#24441,#24442),(#24443,
#24444),(#24445,#24446),(#24447,#24448),(#24449,#24450),(#24451,#24452),
(#24453,#24454),(#24455,#24456),(#24457,#24458),(#24459,#24460),(#24461,
#24462),(#24463,#24464),(#24465,#24466),(#24467,#24468),(#24469,#24470),
(#24471,#24472),(#24473,#24474),(#24475,#24476),(#24477,#24478),(#24479,
#24480),(#24481,#24482),(#24483,#24484),(#24485,#24486),(#24487,#24488),
(#24489,#24490),(#24491,#24492),(#24493,#24494),(#24495,#24496),(#24497,
#24498),(#24499,#24500),(#24501,#24502),(#24503,#24504),(#24505,#24506),
(#24507,#24508),(#24509,#24510),(#24511,#24512),(#24513,#24514),(#24515,
#24516),(#24517,#24518),(#24519,#24520),(#24521,#24522)),.UNSPECIFIED.,
 .F.,.F.,.F.)
B_SPLINE_SURFACE_WITH_KNOTS((6,1,1,1,1,1,1,1,1,1,1,1,1,1,1,1,1,1,1,1,1,
1,1,1,1,1,1,1,1,1,1,1,1,1,1,1,1,1,1,1,1,1,1,1,1,1,1,1,1,1,1,1,1,1,1,1,1,
1,1,1,1,1,1,1,1,6),(2,2),(-1.,-0.984615384615383,-0.969230769230768,-0.953846153846152,
-0.938461538461537,-0.923076923076922,-0.907692307692306,-0.892307692307691,
-0.876923076923076,-0.86153846153846,-0.846153846153845,-0.83076923076923,
-0.815384615384614,-0.799999999999999,-0.784615384615384,-0.769230769230768,
-0.753846153846153,-0.738461538461538,-0.723076923076922,-0.707692307692307,
-0.692307692307692,-0.676923076923076,-0.661538461538461,-0.646153846153846,
-0.63076923076923,-0.615384615384615,-0.6,-0.584615384615384,-0.569230769230769,
-0.553846153846154,-0.538461538461538,-0.523076923076923,-0.507692307692308,
-0.492307692307692,-0.476923076923077,-0.461538461538462,-0.446153846153846,
-0.430769230769231,-0.415384615384615,-0.4,-0.384615384615385,-0.369230769230769,
-0.353846153846154,-0.338461538461538,-0.323076923076923,-0.307692307692308,
-0.292307692307692,-0.276923076923077,-0.261538461538462,-0.246153846153846,
-0.230769230769231,-0.215384615384615,-0.2,-0.184615384615385,-0.169230769230769,
-0.153846153846154,-0.138461538461538,-0.123076923076923,-0.107692307692308,
-0.0923076923076923,-0.0769230769230769,-0.0615384615384615,-0.0461538461538462,
-0.0307692307692308,-0.0153846153846154,0.),(-1.,1.),.UNSPECIFIED.)
GEOMETRIC_REPRESENTATION_ITEM()
RATIONAL_B_SPLINE_SURFACE(((1.,1.),(1.,1.),(1.,1.),(1.,1.),(1.,1.),(1.,
1.),(1.,1.),(1.,1.),(1.,1.),(1.,1.),(1.,1.),(1.,1.),(1.,1.),(1.,1.),(1.,
1.),(1.,1.),(1.,1.),(1.,1.),(1.,1.),(1.,1.),(1.,1.),(1.,1.),(1.,1.),(1.,
1.),(1.,1.),(1.,1.),(1.,1.),(1.,1.),(1.,1.),(1.,1.),(1.,1.),(1.,1.),(1.,
1.),(1.,1.),(1.,1.),(1.,1.),(1.,1.),(1.,1.),(1.,1.),(1.,1.),(1.,1.),(1.,
1.),(1.,1.),(1.,1.),(1.,1.),(1.,1.),(1.,1.),(1.,1.),(1.,1.),(1.,1.),(1.,
1.),(1.,1.),(1.,1.),(1.,1.),(1.,1.),(1.,1.),(1.,1.),(1.,1.),(1.,1.),(1.,
1.),(1.,1.),(1.,1.),(1.,1.),(1.,1.),(1.,1.),(1.,1.),(1.,1.),(1.,1.),(1.,
1.),(1.,1.)))
REPRESENTATION_ITEM('')
SURFACE()
);
#27=(
BOUNDED_SURFACE()
B_SPLINE_SURFACE(5,1,((#24599,#24600),(#24601,#24602),(#24603,#24604),(#24605,
#24606),(#24607,#24608),(#24609,#24610),(#24611,#24612),(#24613,#24614),
(#24615,#24616),(#24617,#24618),(#24619,#24620),(#24621,#24622),(#24623,
#24624),(#24625,#24626),(#24627,#24628),(#24629,#24630),(#24631,#24632),
(#24633,#24634),(#24635,#24636),(#24637,#24638),(#24639,#24640),(#24641,
#24642),(#24643,#24644),(#24645,#24646),(#24647,#24648),(#24649,#24650),
(#24651,#24652),(#24653,#24654),(#24655,#24656),(#24657,#24658),(#24659,
#24660),(#24661,#24662),(#24663,#24664),(#24665,#24666),(#24667,#24668),
(#24669,#24670),(#24671,#24672),(#24673,#24674),(#24675,#24676),(#24677,
#24678),(#24679,#24680),(#24681,#24682),(#24683,#24684),(#24685,#24686),
(#24687,#24688),(#24689,#24690),(#24691,#24692),(#24693,#24694),(#24695,
#24696),(#24697,#24698),(#24699,#24700),(#24701,#24702),(#24703,#24704),
(#24705,#24706),(#24707,#24708),(#24709,#24710),(#24711,#24712),(#24713,
#24714),(#24715,#24716),(#24717,#24718),(#24719,#24720),(#24721,#24722),
(#24723,#24724),(#24725,#24726),(#24727,#24728),(#24729,#24730),(#24731,
#24732),(#24733,#24734),(#24735,#24736),(#24737,#24738)),.UNSPECIFIED.,
 .F.,.F.,.F.)
B_SPLINE_SURFACE_WITH_KNOTS((6,1,1,1,1,1,1,1,1,1,1,1,1,1,1,1,1,1,1,1,1,
1,1,1,1,1,1,1,1,1,1,1,1,1,1,1,1,1,1,1,1,1,1,1,1,1,1,1,1,1,1,1,1,1,1,1,1,
1,1,1,1,1,1,1,1,6),(2,2),(-1.,-0.984615384615383,-0.969230769230768,-0.953846153846152,
-0.938461538461537,-0.923076923076922,-0.907692307692306,-0.892307692307691,
-0.876923076923076,-0.86153846153846,-0.846153846153845,-0.83076923076923,
-0.815384615384614,-0.799999999999999,-0.784615384615384,-0.769230769230768,
-0.753846153846153,-0.738461538461538,-0.723076923076922,-0.707692307692307,
-0.692307692307692,-0.676923076923076,-0.661538461538461,-0.646153846153846,
-0.63076923076923,-0.615384615384615,-0.6,-0.584615384615384,-0.569230769230769,
-0.553846153846154,-0.538461538461538,-0.523076923076923,-0.507692307692308,
-0.492307692307692,-0.476923076923077,-0.461538461538462,-0.446153846153846,
-0.430769230769231,-0.415384615384615,-0.4,-0.384615384615385,-0.369230769230769,
-0.353846153846154,-0.338461538461538,-0.323076923076923,-0.307692307692308,
-0.292307692307692,-0.276923076923077,-0.261538461538462,-0.246153846153846,
-0.230769230769231,-0.215384615384615,-0.2,-0.184615384615385,-0.169230769230769,
-0.153846153846154,-0.138461538461538,-0.123076923076923,-0.107692307692308,
-0.0923076923076923,-0.0769230769230769,-0.0615384615384615,-0.0461538461538462,
-0.0307692307692308,-0.0153846153846154,0.),(-1.,1.),.UNSPECIFIED.)
GEOMETRIC_REPRESENTATION_ITEM()
RATIONAL_B_SPLINE_SURFACE(((1.,1.),(1.,1.),(1.,1.),(1.,1.),(1.,1.),(1.,
1.),(1.,1.),(1.,1.),(1.,1.),(1.,1.),(1.,1.),(1.,1.),(1.,1.),(1.,1.),(1.,
1.),(1.,1.),(1.,1.),(1.,1.),(1.,1.),(1.,1.),(1.,1.),(1.,1.),(1.,1.),(1.,
1.),(1.,1.),(1.,1.),(1.,1.),(1.,1.),(1.,1.),(1.,1.),(1.,1.),(1.,1.),(1.,
1.),(1.,1.),(1.,1.),(1.,1.),(1.,1.),(1.,1.),(1.,1.),(1.,1.),(1.,1.),(1.,
1.),(1.,1.),(1.,1.),(1.,1.),(1.,1.),(1.,1.),(1.,1.),(1.,1.),(1.,1.),(1.,
1.),(1.,1.),(1.,1.),(1.,1.),(1.,1.),(1.,1.),(1.,1.),(1.,1.),(1.,1.),(1.,
1.),(1.,1.),(1.,1.),(1.,1.),(1.,1.),(1.,1.),(1.,1.),(1.,1.),(1.,1.),(1.,
1.),(1.,1.)))
REPRESENTATION_ITEM('')
SURFACE()
);
#28=(
BOUNDED_SURFACE()
B_SPLINE_SURFACE(5,1,((#24815,#24816),(#24817,#24818),(#24819,#24820),(#24821,
#24822),(#24823,#24824),(#24825,#24826),(#24827,#24828),(#24829,#24830),
(#24831,#24832),(#24833,#24834),(#24835,#24836),(#24837,#24838),(#24839,
#24840),(#24841,#24842),(#24843,#24844),(#24845,#24846),(#24847,#24848),
(#24849,#24850),(#24851,#24852),(#24853,#24854),(#24855,#24856),(#24857,
#24858),(#24859,#24860),(#24861,#24862),(#24863,#24864),(#24865,#24866),
(#24867,#24868),(#24869,#24870),(#24871,#24872),(#24873,#24874),(#24875,
#24876),(#24877,#24878),(#24879,#24880),(#24881,#24882),(#24883,#24884),
(#24885,#24886),(#24887,#24888),(#24889,#24890),(#24891,#24892),(#24893,
#24894),(#24895,#24896),(#24897,#24898),(#24899,#24900),(#24901,#24902),
(#24903,#24904),(#24905,#24906),(#24907,#24908),(#24909,#24910),(#24911,
#24912),(#24913,#24914),(#24915,#24916),(#24917,#24918),(#24919,#24920),
(#24921,#24922),(#24923,#24924),(#24925,#24926),(#24927,#24928),(#24929,
#24930),(#24931,#24932),(#24933,#24934),(#24935,#24936),(#24937,#24938),
(#24939,#24940),(#24941,#24942),(#24943,#24944),(#24945,#24946),(#24947,
#24948),(#24949,#24950),(#24951,#24952),(#24953,#24954)),.UNSPECIFIED.,
 .F.,.F.,.F.)
B_SPLINE_SURFACE_WITH_KNOTS((6,1,1,1,1,1,1,1,1,1,1,1,1,1,1,1,1,1,1,1,1,
1,1,1,1,1,1,1,1,1,1,1,1,1,1,1,1,1,1,1,1,1,1,1,1,1,1,1,1,1,1,1,1,1,1,1,1,
1,1,1,1,1,1,1,1,6),(2,2),(-1.,-0.984615384615383,-0.969230769230768,-0.953846153846152,
-0.938461538461537,-0.923076923076922,-0.907692307692306,-0.892307692307691,
-0.876923076923076,-0.86153846153846,-0.846153846153845,-0.83076923076923,
-0.815384615384614,-0.799999999999999,-0.784615384615384,-0.769230769230768,
-0.753846153846153,-0.738461538461538,-0.723076923076922,-0.707692307692307,
-0.692307692307692,-0.676923076923076,-0.661538461538461,-0.646153846153846,
-0.63076923076923,-0.615384615384615,-0.6,-0.584615384615384,-0.569230769230769,
-0.553846153846154,-0.538461538461538,-0.523076923076923,-0.507692307692308,
-0.492307692307692,-0.476923076923077,-0.461538461538462,-0.446153846153846,
-0.430769230769231,-0.415384615384615,-0.4,-0.384615384615385,-0.369230769230769,
-0.353846153846154,-0.338461538461538,-0.323076923076923,-0.307692307692308,
-0.292307692307692,-0.276923076923077,-0.261538461538462,-0.246153846153846,
-0.230769230769231,-0.215384615384615,-0.2,-0.184615384615385,-0.169230769230769,
-0.153846153846154,-0.138461538461538,-0.123076923076923,-0.107692307692308,
-0.0923076923076923,-0.0769230769230769,-0.0615384615384615,-0.0461538461538462,
-0.0307692307692308,-0.0153846153846154,0.),(-1.,1.),.UNSPECIFIED.)
GEOMETRIC_REPRESENTATION_ITEM()
RATIONAL_B_SPLINE_SURFACE(((1.,1.),(1.,1.),(1.,1.),(1.,1.),(1.,1.),(1.,
1.),(1.,1.),(1.,1.),(1.,1.),(1.,1.),(1.,1.),(1.,1.),(1.,1.),(1.,1.),(1.,
1.),(1.,1.),(1.,1.),(1.,1.),(1.,1.),(1.,1.),(1.,1.),(1.,1.),(1.,1.),(1.,
1.),(1.,1.),(1.,1.),(1.,1.),(1.,1.),(1.,1.),(1.,1.),(1.,1.),(1.,1.),(1.,
1.),(1.,1.),(1.,1.),(1.,1.),(1.,1.),(1.,1.),(1.,1.),(1.,1.),(1.,1.),(1.,
1.),(1.,1.),(1.,1.),(1.,1.),(1.,1.),(1.,1.),(1.,1.),(1.,1.),(1.,1.),(1.,
1.),(1.,1.),(1.,1.),(1.,1.),(1.,1.),(1.,1.),(1.,1.),(1.,1.),(1.,1.),(1.,
1.),(1.,1.),(1.,1.),(1.,1.),(1.,1.),(1.,1.),(1.,1.),(1.,1.),(1.,1.),(1.,
1.),(1.,1.)))
REPRESENTATION_ITEM('')
SURFACE()
);
#29=(
BOUNDED_SURFACE()
B_SPLINE_SURFACE(5,1,((#25031,#25032),(#25033,#25034),(#25035,#25036),(#25037,
#25038),(#25039,#25040),(#25041,#25042),(#25043,#25044),(#25045,#25046),
(#25047,#25048),(#25049,#25050),(#25051,#25052),(#25053,#25054),(#25055,
#25056),(#25057,#25058),(#25059,#25060),(#25061,#25062),(#25063,#25064),
(#25065,#25066),(#25067,#25068),(#25069,#25070),(#25071,#25072),(#25073,
#25074),(#25075,#25076),(#25077,#25078),(#25079,#25080),(#25081,#25082),
(#25083,#25084),(#25085,#25086),(#25087,#25088),(#25089,#25090),(#25091,
#25092),(#25093,#25094),(#25095,#25096),(#25097,#25098),(#25099,#25100),
(#25101,#25102),(#25103,#25104),(#25105,#25106),(#25107,#25108),(#25109,
#25110),(#25111,#25112),(#25113,#25114),(#25115,#25116),(#25117,#25118),
(#25119,#25120),(#25121,#25122),(#25123,#25124),(#25125,#25126),(#25127,
#25128),(#25129,#25130),(#25131,#25132),(#25133,#25134),(#25135,#25136),
(#25137,#25138),(#25139,#25140),(#25141,#25142),(#25143,#25144),(#25145,
#25146),(#25147,#25148),(#25149,#25150),(#25151,#25152),(#25153,#25154),
(#25155,#25156),(#25157,#25158),(#25159,#25160),(#25161,#25162),(#25163,
#25164),(#25165,#25166),(#25167,#25168),(#25169,#25170)),.UNSPECIFIED.,
 .F.,.F.,.F.)
B_SPLINE_SURFACE_WITH_KNOTS((6,1,1,1,1,1,1,1,1,1,1,1,1,1,1,1,1,1,1,1,1,
1,1,1,1,1,1,1,1,1,1,1,1,1,1,1,1,1,1,1,1,1,1,1,1,1,1,1,1,1,1,1,1,1,1,1,1,
1,1,1,1,1,1,1,1,6),(2,2),(-1.,-0.984615384615383,-0.969230769230768,-0.953846153846152,
-0.938461538461537,-0.923076923076922,-0.907692307692306,-0.892307692307691,
-0.876923076923076,-0.86153846153846,-0.846153846153845,-0.83076923076923,
-0.815384615384614,-0.799999999999999,-0.784615384615384,-0.769230769230768,
-0.753846153846153,-0.738461538461538,-0.723076923076922,-0.707692307692307,
-0.692307692307692,-0.676923076923076,-0.661538461538461,-0.646153846153846,
-0.63076923076923,-0.615384615384615,-0.6,-0.584615384615384,-0.569230769230769,
-0.553846153846154,-0.538461538461538,-0.523076923076923,-0.507692307692308,
-0.492307692307692,-0.476923076923077,-0.461538461538462,-0.446153846153846,
-0.430769230769231,-0.415384615384615,-0.4,-0.384615384615385,-0.369230769230769,
-0.353846153846154,-0.338461538461538,-0.323076923076923,-0.307692307692308,
-0.292307692307692,-0.276923076923077,-0.261538461538462,-0.246153846153846,
-0.230769230769231,-0.215384615384615,-0.2,-0.184615384615385,-0.169230769230769,
-0.153846153846154,-0.138461538461538,-0.123076923076923,-0.107692307692308,
-0.0923076923076923,-0.0769230769230769,-0.0615384615384615,-0.0461538461538462,
-0.0307692307692308,-0.0153846153846154,0.),(-1.,1.),.UNSPECIFIED.)
GEOMETRIC_REPRESENTATION_ITEM()
RATIONAL_B_SPLINE_SURFACE(((1.,1.),(1.,1.),(1.,1.),(1.,1.),(1.,1.),(1.,
1.),(1.,1.),(1.,1.),(1.,1.),(1.,1.),(1.,1.),(1.,1.),(1.,1.),(1.,1.),(1.,
1.),(1.,1.),(1.,1.),(1.,1.),(1.,1.),(1.,1.),(1.,1.),(1.,1.),(1.,1.),(1.,
1.),(1.,1.),(1.,1.),(1.,1.),(1.,1.),(1.,1.),(1.,1.),(1.,1.),(1.,1.),(1.,
1.),(1.,1.),(1.,1.),(1.,1.),(1.,1.),(1.,1.),(1.,1.),(1.,1.),(1.,1.),(1.,
1.),(1.,1.),(1.,1.),(1.,1.),(1.,1.),(1.,1.),(1.,1.),(1.,1.),(1.,1.),(1.,
1.),(1.,1.),(1.,1.),(1.,1.),(1.,1.),(1.,1.),(1.,1.),(1.,1.),(1.,1.),(1.,
1.),(1.,1.),(1.,1.),(1.,1.),(1.,1.),(1.,1.),(1.,1.),(1.,1.),(1.,1.),(1.,
1.),(1.,1.)))
REPRESENTATION_ITEM('')
SURFACE()
);
#30=(
BOUNDED_SURFACE()
B_SPLINE_SURFACE(5,1,((#25247,#25248),(#25249,#25250),(#25251,#25252),(#25253,
#25254),(#25255,#25256),(#25257,#25258),(#25259,#25260),(#25261,#25262),
(#25263,#25264),(#25265,#25266),(#25267,#25268),(#25269,#25270),(#25271,
#25272),(#25273,#25274),(#25275,#25276),(#25277,#25278),(#25279,#25280),
(#25281,#25282),(#25283,#25284),(#25285,#25286),(#25287,#25288),(#25289,
#25290),(#25291,#25292),(#25293,#25294),(#25295,#25296),(#25297,#25298),
(#25299,#25300),(#25301,#25302),(#25303,#25304),(#25305,#25306),(#25307,
#25308),(#25309,#25310),(#25311,#25312),(#25313,#25314),(#25315,#25316),
(#25317,#25318),(#25319,#25320),(#25321,#25322),(#25323,#25324),(#25325,
#25326),(#25327,#25328),(#25329,#25330),(#25331,#25332),(#25333,#25334),
(#25335,#25336),(#25337,#25338),(#25339,#25340),(#25341,#25342),(#25343,
#25344),(#25345,#25346),(#25347,#25348),(#25349,#25350),(#25351,#25352),
(#25353,#25354),(#25355,#25356),(#25357,#25358),(#25359,#25360),(#25361,
#25362),(#25363,#25364),(#25365,#25366),(#25367,#25368),(#25369,#25370),
(#25371,#25372),(#25373,#25374),(#25375,#25376),(#25377,#25378),(#25379,
#25380),(#25381,#25382),(#25383,#25384),(#25385,#25386)),.UNSPECIFIED.,
 .F.,.F.,.F.)
B_SPLINE_SURFACE_WITH_KNOTS((6,1,1,1,1,1,1,1,1,1,1,1,1,1,1,1,1,1,1,1,1,
1,1,1,1,1,1,1,1,1,1,1,1,1,1,1,1,1,1,1,1,1,1,1,1,1,1,1,1,1,1,1,1,1,1,1,1,
1,1,1,1,1,1,1,1,6),(2,2),(-1.,-0.984615384615383,-0.969230769230768,-0.953846153846152,
-0.938461538461537,-0.923076923076922,-0.907692307692306,-0.892307692307691,
-0.876923076923076,-0.86153846153846,-0.846153846153845,-0.83076923076923,
-0.815384615384614,-0.799999999999999,-0.784615384615384,-0.769230769230768,
-0.753846153846153,-0.738461538461538,-0.723076923076922,-0.707692307692307,
-0.692307692307692,-0.676923076923076,-0.661538461538461,-0.646153846153846,
-0.63076923076923,-0.615384615384615,-0.6,-0.584615384615384,-0.569230769230769,
-0.553846153846154,-0.538461538461538,-0.523076923076923,-0.507692307692308,
-0.492307692307692,-0.476923076923077,-0.461538461538462,-0.446153846153846,
-0.430769230769231,-0.415384615384615,-0.4,-0.384615384615385,-0.369230769230769,
-0.353846153846154,-0.338461538461538,-0.323076923076923,-0.307692307692308,
-0.292307692307692,-0.276923076923077,-0.261538461538462,-0.246153846153846,
-0.230769230769231,-0.215384615384615,-0.2,-0.184615384615385,-0.169230769230769,
-0.153846153846154,-0.138461538461538,-0.123076923076923,-0.107692307692308,
-0.0923076923076923,-0.0769230769230769,-0.0615384615384615,-0.0461538461538462,
-0.0307692307692308,-0.0153846153846154,0.),(-1.,1.),.UNSPECIFIED.)
GEOMETRIC_REPRESENTATION_ITEM()
RATIONAL_B_SPLINE_SURFACE(((1.,1.),(1.,1.),(1.,1.),(1.,1.),(1.,1.),(1.,
1.),(1.,1.),(1.,1.),(1.,1.),(1.,1.),(1.,1.),(1.,1.),(1.,1.),(1.,1.),(1.,
1.),(1.,1.),(1.,1.),(1.,1.),(1.,1.),(1.,1.),(1.,1.),(1.,1.),(1.,1.),(1.,
1.),(1.,1.),(1.,1.),(1.,1.),(1.,1.),(1.,1.),(1.,1.),(1.,1.),(1.,1.),(1.,
1.),(1.,1.),(1.,1.),(1.,1.),(1.,1.),(1.,1.),(1.,1.),(1.,1.),(1.,1.),(1.,
1.),(1.,1.),(1.,1.),(1.,1.),(1.,1.),(1.,1.),(1.,1.),(1.,1.),(1.,1.),(1.,
1.),(1.,1.),(1.,1.),(1.,1.),(1.,1.),(1.,1.),(1.,1.),(1.,1.),(1.,1.),(1.,
1.),(1.,1.),(1.,1.),(1.,1.),(1.,1.),(1.,1.),(1.,1.),(1.,1.),(1.,1.),(1.,
1.),(1.,1.)))
REPRESENTATION_ITEM('')
SURFACE()
);
#31=(
BOUNDED_SURFACE()
B_SPLINE_SURFACE(5,1,((#25463,#25464),(#25465,#25466),(#25467,#25468),(#25469,
#25470),(#25471,#25472),(#25473,#25474),(#25475,#25476),(#25477,#25478),
(#25479,#25480),(#25481,#25482),(#25483,#25484),(#25485,#25486),(#25487,
#25488),(#25489,#25490),(#25491,#25492),(#25493,#25494),(#25495,#25496),
(#25497,#25498),(#25499,#25500),(#25501,#25502),(#25503,#25504),(#25505,
#25506),(#25507,#25508),(#25509,#25510),(#25511,#25512),(#25513,#25514),
(#25515,#25516),(#25517,#25518),(#25519,#25520),(#25521,#25522),(#25523,
#25524),(#25525,#25526),(#25527,#25528),(#25529,#25530),(#25531,#25532),
(#25533,#25534),(#25535,#25536),(#25537,#25538),(#25539,#25540),(#25541,
#25542),(#25543,#25544),(#25545,#25546),(#25547,#25548),(#25549,#25550),
(#25551,#25552),(#25553,#25554),(#25555,#25556),(#25557,#25558),(#25559,
#25560),(#25561,#25562),(#25563,#25564),(#25565,#25566),(#25567,#25568),
(#25569,#25570),(#25571,#25572),(#25573,#25574),(#25575,#25576),(#25577,
#25578),(#25579,#25580),(#25581,#25582),(#25583,#25584),(#25585,#25586),
(#25587,#25588),(#25589,#25590),(#25591,#25592),(#25593,#25594),(#25595,
#25596),(#25597,#25598),(#25599,#25600),(#25601,#25602)),.UNSPECIFIED.,
 .F.,.F.,.F.)
B_SPLINE_SURFACE_WITH_KNOTS((6,1,1,1,1,1,1,1,1,1,1,1,1,1,1,1,1,1,1,1,1,
1,1,1,1,1,1,1,1,1,1,1,1,1,1,1,1,1,1,1,1,1,1,1,1,1,1,1,1,1,1,1,1,1,1,1,1,
1,1,1,1,1,1,1,1,6),(2,2),(-1.,-0.984615384615383,-0.969230769230768,-0.953846153846152,
-0.938461538461537,-0.923076923076922,-0.907692307692306,-0.892307692307691,
-0.876923076923076,-0.86153846153846,-0.846153846153845,-0.83076923076923,
-0.815384615384614,-0.799999999999999,-0.784615384615384,-0.769230769230768,
-0.753846153846153,-0.738461538461538,-0.723076923076922,-0.707692307692307,
-0.692307692307692,-0.676923076923076,-0.661538461538461,-0.646153846153846,
-0.63076923076923,-0.615384615384615,-0.6,-0.584615384615384,-0.569230769230769,
-0.553846153846154,-0.538461538461538,-0.523076923076923,-0.507692307692308,
-0.492307692307692,-0.476923076923077,-0.461538461538462,-0.446153846153846,
-0.430769230769231,-0.415384615384615,-0.4,-0.384615384615385,-0.369230769230769,
-0.353846153846154,-0.338461538461538,-0.323076923076923,-0.307692307692308,
-0.292307692307692,-0.276923076923077,-0.261538461538462,-0.246153846153846,
-0.230769230769231,-0.215384615384615,-0.2,-0.184615384615385,-0.169230769230769,
-0.153846153846154,-0.138461538461538,-0.123076923076923,-0.107692307692308,
-0.0923076923076923,-0.0769230769230769,-0.0615384615384615,-0.0461538461538462,
-0.0307692307692308,-0.0153846153846154,0.),(-1.,1.),.UNSPECIFIED.)
GEOMETRIC_REPRESENTATION_ITEM()
RATIONAL_B_SPLINE_SURFACE(((1.,1.),(1.,1.),(1.,1.),(1.,1.),(1.,1.),(1.,
1.),(1.,1.),(1.,1.),(1.,1.),(1.,1.),(1.,1.),(1.,1.),(1.,1.),(1.,1.),(1.,
1.),(1.,1.),(1.,1.),(1.,1.),(1.,1.),(1.,1.),(1.,1.),(1.,1.),(1.,1.),(1.,
1.),(1.,1.),(1.,1.),(1.,1.),(1.,1.),(1.,1.),(1.,1.),(1.,1.),(1.,1.),(1.,
1.),(1.,1.),(1.,1.),(1.,1.),(1.,1.),(1.,1.),(1.,1.),(1.,1.),(1.,1.),(1.,
1.),(1.,1.),(1.,1.),(1.,1.),(1.,1.),(1.,1.),(1.,1.),(1.,1.),(1.,1.),(1.,
1.),(1.,1.),(1.,1.),(1.,1.),(1.,1.),(1.,1.),(1.,1.),(1.,1.),(1.,1.),(1.,
1.),(1.,1.),(1.,1.),(1.,1.),(1.,1.),(1.,1.),(1.,1.),(1.,1.),(1.,1.),(1.,
1.),(1.,1.)))
REPRESENTATION_ITEM('')
SURFACE()
);
#32=(
BOUNDED_SURFACE()
B_SPLINE_SURFACE(5,1,((#25679,#25680),(#25681,#25682),(#25683,#25684),(#25685,
#25686),(#25687,#25688),(#25689,#25690),(#25691,#25692),(#25693,#25694),
(#25695,#25696),(#25697,#25698),(#25699,#25700),(#25701,#25702),(#25703,
#25704),(#25705,#25706),(#25707,#25708),(#25709,#25710),(#25711,#25712),
(#25713,#25714),(#25715,#25716),(#25717,#25718),(#25719,#25720),(#25721,
#25722),(#25723,#25724),(#25725,#25726),(#25727,#25728),(#25729,#25730),
(#25731,#25732),(#25733,#25734),(#25735,#25736),(#25737,#25738),(#25739,
#25740),(#25741,#25742),(#25743,#25744),(#25745,#25746),(#25747,#25748),
(#25749,#25750),(#25751,#25752),(#25753,#25754),(#25755,#25756),(#25757,
#25758),(#25759,#25760),(#25761,#25762),(#25763,#25764),(#25765,#25766),
(#25767,#25768),(#25769,#25770),(#25771,#25772),(#25773,#25774),(#25775,
#25776),(#25777,#25778),(#25779,#25780),(#25781,#25782),(#25783,#25784),
(#25785,#25786),(#25787,#25788),(#25789,#25790),(#25791,#25792),(#25793,
#25794),(#25795,#25796),(#25797,#25798),(#25799,#25800),(#25801,#25802),
(#25803,#25804),(#25805,#25806),(#25807,#25808),(#25809,#25810),(#25811,
#25812),(#25813,#25814),(#25815,#25816),(#25817,#25818)),.UNSPECIFIED.,
 .F.,.F.,.F.)
B_SPLINE_SURFACE_WITH_KNOTS((6,1,1,1,1,1,1,1,1,1,1,1,1,1,1,1,1,1,1,1,1,
1,1,1,1,1,1,1,1,1,1,1,1,1,1,1,1,1,1,1,1,1,1,1,1,1,1,1,1,1,1,1,1,1,1,1,1,
1,1,1,1,1,1,1,1,6),(2,2),(-1.,-0.984615384615383,-0.969230769230768,-0.953846153846152,
-0.938461538461537,-0.923076923076922,-0.907692307692306,-0.892307692307691,
-0.876923076923076,-0.86153846153846,-0.846153846153845,-0.83076923076923,
-0.815384615384614,-0.799999999999999,-0.784615384615384,-0.769230769230768,
-0.753846153846153,-0.738461538461538,-0.723076923076922,-0.707692307692307,
-0.692307692307692,-0.676923076923076,-0.661538461538461,-0.646153846153846,
-0.63076923076923,-0.615384615384615,-0.6,-0.584615384615384,-0.569230769230769,
-0.553846153846154,-0.538461538461538,-0.523076923076923,-0.507692307692308,
-0.492307692307692,-0.476923076923077,-0.461538461538462,-0.446153846153846,
-0.430769230769231,-0.415384615384615,-0.4,-0.384615384615385,-0.369230769230769,
-0.353846153846154,-0.338461538461538,-0.323076923076923,-0.307692307692308,
-0.292307692307692,-0.276923076923077,-0.261538461538462,-0.246153846153846,
-0.230769230769231,-0.215384615384615,-0.2,-0.184615384615385,-0.169230769230769,
-0.153846153846154,-0.138461538461538,-0.123076923076923,-0.107692307692308,
-0.0923076923076923,-0.0769230769230769,-0.0615384615384615,-0.0461538461538462,
-0.0307692307692308,-0.0153846153846154,0.),(-1.,1.),.UNSPECIFIED.)
GEOMETRIC_REPRESENTATION_ITEM()
RATIONAL_B_SPLINE_SURFACE(((1.,1.),(1.,1.),(1.,1.),(1.,1.),(1.,1.),(1.,
1.),(1.,1.),(1.,1.),(1.,1.),(1.,1.),(1.,1.),(1.,1.),(1.,1.),(1.,1.),(1.,
1.),(1.,1.),(1.,1.),(1.,1.),(1.,1.),(1.,1.),(1.,1.),(1.,1.),(1.,1.),(1.,
1.),(1.,1.),(1.,1.),(1.,1.),(1.,1.),(1.,1.),(1.,1.),(1.,1.),(1.,1.),(1.,
1.),(1.,1.),(1.,1.),(1.,1.),(1.,1.),(1.,1.),(1.,1.),(1.,1.),(1.,1.),(1.,
1.),(1.,1.),(1.,1.),(1.,1.),(1.,1.),(1.,1.),(1.,1.),(1.,1.),(1.,1.),(1.,
1.),(1.,1.),(1.,1.),(1.,1.),(1.,1.),(1.,1.),(1.,1.),(1.,1.),(1.,1.),(1.,
1.),(1.,1.),(1.,1.),(1.,1.),(1.,1.),(1.,1.),(1.,1.),(1.,1.),(1.,1.),(1.,
1.),(1.,1.)))
REPRESENTATION_ITEM('')
SURFACE()
);
#33=(
BOUNDED_SURFACE()
B_SPLINE_SURFACE(5,1,((#25895,#25896),(#25897,#25898),(#25899,#25900),(#25901,
#25902),(#25903,#25904),(#25905,#25906),(#25907,#25908),(#25909,#25910),
(#25911,#25912),(#25913,#25914),(#25915,#25916),(#25917,#25918),(#25919,
#25920),(#25921,#25922),(#25923,#25924),(#25925,#25926),(#25927,#25928),
(#25929,#25930),(#25931,#25932),(#25933,#25934),(#25935,#25936),(#25937,
#25938),(#25939,#25940),(#25941,#25942),(#25943,#25944),(#25945,#25946),
(#25947,#25948),(#25949,#25950),(#25951,#25952),(#25953,#25954),(#25955,
#25956),(#25957,#25958),(#25959,#25960),(#25961,#25962),(#25963,#25964),
(#25965,#25966),(#25967,#25968),(#25969,#25970),(#25971,#25972),(#25973,
#25974),(#25975,#25976),(#25977,#25978),(#25979,#25980),(#25981,#25982),
(#25983,#25984),(#25985,#25986),(#25987,#25988),(#25989,#25990),(#25991,
#25992),(#25993,#25994),(#25995,#25996),(#25997,#25998),(#25999,#26000),
(#26001,#26002),(#26003,#26004),(#26005,#26006),(#26007,#26008),(#26009,
#26010),(#26011,#26012),(#26013,#26014),(#26015,#26016),(#26017,#26018),
(#26019,#26020),(#26021,#26022),(#26023,#26024),(#26025,#26026),(#26027,
#26028),(#26029,#26030),(#26031,#26032),(#26033,#26034)),.UNSPECIFIED.,
 .F.,.F.,.F.)
B_SPLINE_SURFACE_WITH_KNOTS((6,1,1,1,1,1,1,1,1,1,1,1,1,1,1,1,1,1,1,1,1,
1,1,1,1,1,1,1,1,1,1,1,1,1,1,1,1,1,1,1,1,1,1,1,1,1,1,1,1,1,1,1,1,1,1,1,1,
1,1,1,1,1,1,1,1,6),(2,2),(-1.,-0.984615384615383,-0.969230769230768,-0.953846153846152,
-0.938461538461537,-0.923076923076922,-0.907692307692306,-0.892307692307691,
-0.876923076923076,-0.86153846153846,-0.846153846153845,-0.83076923076923,
-0.815384615384614,-0.799999999999999,-0.784615384615384,-0.769230769230768,
-0.753846153846153,-0.738461538461538,-0.723076923076922,-0.707692307692307,
-0.692307692307692,-0.676923076923076,-0.661538461538461,-0.646153846153846,
-0.63076923076923,-0.615384615384615,-0.6,-0.584615384615384,-0.569230769230769,
-0.553846153846154,-0.538461538461538,-0.523076923076923,-0.507692307692308,
-0.492307692307692,-0.476923076923077,-0.461538461538462,-0.446153846153846,
-0.430769230769231,-0.415384615384615,-0.4,-0.384615384615385,-0.369230769230769,
-0.353846153846154,-0.338461538461538,-0.323076923076923,-0.307692307692308,
-0.292307692307692,-0.276923076923077,-0.261538461538462,-0.246153846153846,
-0.230769230769231,-0.215384615384615,-0.2,-0.184615384615385,-0.169230769230769,
-0.153846153846154,-0.138461538461538,-0.123076923076923,-0.107692307692308,
-0.0923076923076923,-0.0769230769230769,-0.0615384615384615,-0.0461538461538462,
-0.0307692307692308,-0.0153846153846154,0.),(-1.,1.),.UNSPECIFIED.)
GEOMETRIC_REPRESENTATION_ITEM()
RATIONAL_B_SPLINE_SURFACE(((1.,1.),(1.,1.),(1.,1.),(1.,1.),(1.,1.),(1.,
1.),(1.,1.),(1.,1.),(1.,1.),(1.,1.),(1.,1.),(1.,1.),(1.,1.),(1.,1.),(1.,
1.),(1.,1.),(1.,1.),(1.,1.),(1.,1.),(1.,1.),(1.,1.),(1.,1.),(1.,1.),(1.,
1.),(1.,1.),(1.,1.),(1.,1.),(1.,1.),(1.,1.),(1.,1.),(1.,1.),(1.,1.),(1.,
1.),(1.,1.),(1.,1.),(1.,1.),(1.,1.),(1.,1.),(1.,1.),(1.,1.),(1.,1.),(1.,
1.),(1.,1.),(1.,1.),(1.,1.),(1.,1.),(1.,1.),(1.,1.),(1.,1.),(1.,1.),(1.,
1.),(1.,1.),(1.,1.),(1.,1.),(1.,1.),(1.,1.),(1.,1.),(1.,1.),(1.,1.),(1.,
1.),(1.,1.),(1.,1.),(1.,1.),(1.,1.),(1.,1.),(1.,1.),(1.,1.),(1.,1.),(1.,
1.),(1.,1.)))
REPRESENTATION_ITEM('')
SURFACE()
);
#34=(
BOUNDED_SURFACE()
B_SPLINE_SURFACE(5,1,((#26111,#26112),(#26113,#26114),(#26115,#26116),(#26117,
#26118),(#26119,#26120),(#26121,#26122),(#26123,#26124),(#26125,#26126),
(#26127,#26128),(#26129,#26130),(#26131,#26132),(#26133,#26134),(#26135,
#26136),(#26137,#26138),(#26139,#26140),(#26141,#26142),(#26143,#26144),
(#26145,#26146),(#26147,#26148),(#26149,#26150),(#26151,#26152),(#26153,
#26154),(#26155,#26156),(#26157,#26158),(#26159,#26160),(#26161,#26162),
(#26163,#26164),(#26165,#26166),(#26167,#26168),(#26169,#26170),(#26171,
#26172),(#26173,#26174),(#26175,#26176),(#26177,#26178),(#26179,#26180),
(#26181,#26182),(#26183,#26184),(#26185,#26186),(#26187,#26188),(#26189,
#26190),(#26191,#26192),(#26193,#26194),(#26195,#26196),(#26197,#26198),
(#26199,#26200),(#26201,#26202),(#26203,#26204),(#26205,#26206),(#26207,
#26208),(#26209,#26210),(#26211,#26212),(#26213,#26214),(#26215,#26216),
(#26217,#26218),(#26219,#26220),(#26221,#26222),(#26223,#26224),(#26225,
#26226),(#26227,#26228),(#26229,#26230),(#26231,#26232),(#26233,#26234),
(#26235,#26236),(#26237,#26238),(#26239,#26240),(#26241,#26242),(#26243,
#26244),(#26245,#26246),(#26247,#26248),(#26249,#26250)),.UNSPECIFIED.,
 .F.,.F.,.F.)
B_SPLINE_SURFACE_WITH_KNOTS((6,1,1,1,1,1,1,1,1,1,1,1,1,1,1,1,1,1,1,1,1,
1,1,1,1,1,1,1,1,1,1,1,1,1,1,1,1,1,1,1,1,1,1,1,1,1,1,1,1,1,1,1,1,1,1,1,1,
1,1,1,1,1,1,1,1,6),(2,2),(-1.,-0.984615384615383,-0.969230769230768,-0.953846153846152,
-0.938461538461537,-0.923076923076922,-0.907692307692306,-0.892307692307691,
-0.876923076923076,-0.86153846153846,-0.846153846153845,-0.83076923076923,
-0.815384615384614,-0.799999999999999,-0.784615384615384,-0.769230769230768,
-0.753846153846153,-0.738461538461538,-0.723076923076922,-0.707692307692307,
-0.692307692307692,-0.676923076923076,-0.661538461538461,-0.646153846153846,
-0.63076923076923,-0.615384615384615,-0.6,-0.584615384615384,-0.569230769230769,
-0.553846153846154,-0.538461538461538,-0.523076923076923,-0.507692307692308,
-0.492307692307692,-0.476923076923077,-0.461538461538462,-0.446153846153846,
-0.430769230769231,-0.415384615384615,-0.4,-0.384615384615385,-0.369230769230769,
-0.353846153846154,-0.338461538461538,-0.323076923076923,-0.307692307692308,
-0.292307692307692,-0.276923076923077,-0.261538461538462,-0.246153846153846,
-0.230769230769231,-0.215384615384615,-0.2,-0.184615384615385,-0.169230769230769,
-0.153846153846154,-0.138461538461538,-0.123076923076923,-0.107692307692308,
-0.0923076923076923,-0.0769230769230769,-0.0615384615384615,-0.0461538461538462,
-0.0307692307692308,-0.0153846153846154,0.),(-1.,1.),.UNSPECIFIED.)
GEOMETRIC_REPRESENTATION_ITEM()
RATIONAL_B_SPLINE_SURFACE(((1.,1.),(1.,1.),(1.,1.),(1.,1.),(1.,1.),(1.,
1.),(1.,1.),(1.,1.),(1.,1.),(1.,1.),(1.,1.),(1.,1.),(1.,1.),(1.,1.),(1.,
1.),(1.,1.),(1.,1.),(1.,1.),(1.,1.),(1.,1.),(1.,1.),(1.,1.),(1.,1.),(1.,
1.),(1.,1.),(1.,1.),(1.,1.),(1.,1.),(1.,1.),(1.,1.),(1.,1.),(1.,1.),(1.,
1.),(1.,1.),(1.,1.),(1.,1.),(1.,1.),(1.,1.),(1.,1.),(1.,1.),(1.,1.),(1.,
1.),(1.,1.),(1.,1.),(1.,1.),(1.,1.),(1.,1.),(1.,1.),(1.,1.),(1.,1.),(1.,
1.),(1.,1.),(1.,1.),(1.,1.),(1.,1.),(1.,1.),(1.,1.),(1.,1.),(1.,1.),(1.,
1.),(1.,1.),(1.,1.),(1.,1.),(1.,1.),(1.,1.),(1.,1.),(1.,1.),(1.,1.),(1.,
1.),(1.,1.)))
REPRESENTATION_ITEM('')
SURFACE()
);
#35=(
BOUNDED_SURFACE()
B_SPLINE_SURFACE(5,1,((#26327,#26328),(#26329,#26330),(#26331,#26332),(#26333,
#26334),(#26335,#26336),(#26337,#26338),(#26339,#26340),(#26341,#26342),
(#26343,#26344),(#26345,#26346),(#26347,#26348),(#26349,#26350),(#26351,
#26352),(#26353,#26354),(#26355,#26356),(#26357,#26358),(#26359,#26360),
(#26361,#26362),(#26363,#26364),(#26365,#26366),(#26367,#26368),(#26369,
#26370),(#26371,#26372),(#26373,#26374),(#26375,#26376),(#26377,#26378),
(#26379,#26380),(#26381,#26382),(#26383,#26384),(#26385,#26386),(#26387,
#26388),(#26389,#26390),(#26391,#26392),(#26393,#26394),(#26395,#26396),
(#26397,#26398),(#26399,#26400),(#26401,#26402),(#26403,#26404),(#26405,
#26406),(#26407,#26408),(#26409,#26410),(#26411,#26412),(#26413,#26414),
(#26415,#26416),(#26417,#26418),(#26419,#26420),(#26421,#26422),(#26423,
#26424),(#26425,#26426),(#26427,#26428),(#26429,#26430),(#26431,#26432),
(#26433,#26434),(#26435,#26436),(#26437,#26438),(#26439,#26440),(#26441,
#26442),(#26443,#26444),(#26445,#26446),(#26447,#26448),(#26449,#26450),
(#26451,#26452),(#26453,#26454),(#26455,#26456),(#26457,#26458),(#26459,
#26460),(#26461,#26462),(#26463,#26464),(#26465,#26466)),.UNSPECIFIED.,
 .F.,.F.,.F.)
B_SPLINE_SURFACE_WITH_KNOTS((6,1,1,1,1,1,1,1,1,1,1,1,1,1,1,1,1,1,1,1,1,
1,1,1,1,1,1,1,1,1,1,1,1,1,1,1,1,1,1,1,1,1,1,1,1,1,1,1,1,1,1,1,1,1,1,1,1,
1,1,1,1,1,1,1,1,6),(2,2),(-1.,-0.984615384615383,-0.969230769230768,-0.953846153846152,
-0.938461538461537,-0.923076923076922,-0.907692307692306,-0.892307692307691,
-0.876923076923076,-0.86153846153846,-0.846153846153845,-0.83076923076923,
-0.815384615384614,-0.799999999999999,-0.784615384615384,-0.769230769230768,
-0.753846153846153,-0.738461538461538,-0.723076923076922,-0.707692307692307,
-0.692307692307692,-0.676923076923076,-0.661538461538461,-0.646153846153846,
-0.63076923076923,-0.615384615384615,-0.6,-0.584615384615384,-0.569230769230769,
-0.553846153846154,-0.538461538461538,-0.523076923076923,-0.507692307692308,
-0.492307692307692,-0.476923076923077,-0.461538461538462,-0.446153846153846,
-0.430769230769231,-0.415384615384615,-0.4,-0.384615384615385,-0.369230769230769,
-0.353846153846154,-0.338461538461538,-0.323076923076923,-0.307692307692308,
-0.292307692307692,-0.276923076923077,-0.261538461538462,-0.246153846153846,
-0.230769230769231,-0.215384615384615,-0.2,-0.184615384615385,-0.169230769230769,
-0.153846153846154,-0.138461538461538,-0.123076923076923,-0.107692307692308,
-0.0923076923076923,-0.0769230769230769,-0.0615384615384615,-0.0461538461538462,
-0.0307692307692308,-0.0153846153846154,0.),(-1.,1.),.UNSPECIFIED.)
GEOMETRIC_REPRESENTATION_ITEM()
RATIONAL_B_SPLINE_SURFACE(((1.,1.),(1.,1.),(1.,1.),(1.,1.),(1.,1.),(1.,
1.),(1.,1.),(1.,1.),(1.,1.),(1.,1.),(1.,1.),(1.,1.),(1.,1.),(1.,1.),(1.,
1.),(1.,1.),(1.,1.),(1.,1.),(1.,1.),(1.,1.),(1.,1.),(1.,1.),(1.,1.),(1.,
1.),(1.,1.),(1.,1.),(1.,1.),(1.,1.),(1.,1.),(1.,1.),(1.,1.),(1.,1.),(1.,
1.),(1.,1.),(1.,1.),(1.,1.),(1.,1.),(1.,1.),(1.,1.),(1.,1.),(1.,1.),(1.,
1.),(1.,1.),(1.,1.),(1.,1.),(1.,1.),(1.,1.),(1.,1.),(1.,1.),(1.,1.),(1.,
1.),(1.,1.),(1.,1.),(1.,1.),(1.,1.),(1.,1.),(1.,1.),(1.,1.),(1.,1.),(1.,
1.),(1.,1.),(1.,1.),(1.,1.),(1.,1.),(1.,1.),(1.,1.),(1.,1.),(1.,1.),(1.,
1.),(1.,1.)))
REPRESENTATION_ITEM('')
SURFACE()
);
#36=(
BOUNDED_SURFACE()
B_SPLINE_SURFACE(5,1,((#26543,#26544),(#26545,#26546),(#26547,#26548),(#26549,
#26550),(#26551,#26552),(#26553,#26554),(#26555,#26556),(#26557,#26558),
(#26559,#26560),(#26561,#26562),(#26563,#26564),(#26565,#26566),(#26567,
#26568),(#26569,#26570),(#26571,#26572),(#26573,#26574),(#26575,#26576),
(#26577,#26578),(#26579,#26580),(#26581,#26582),(#26583,#26584),(#26585,
#26586),(#26587,#26588),(#26589,#26590),(#26591,#26592),(#26593,#26594),
(#26595,#26596),(#26597,#26598),(#26599,#26600),(#26601,#26602),(#26603,
#26604),(#26605,#26606),(#26607,#26608),(#26609,#26610),(#26611,#26612),
(#26613,#26614),(#26615,#26616),(#26617,#26618),(#26619,#26620),(#26621,
#26622),(#26623,#26624),(#26625,#26626),(#26627,#26628),(#26629,#26630),
(#26631,#26632),(#26633,#26634),(#26635,#26636),(#26637,#26638),(#26639,
#26640),(#26641,#26642),(#26643,#26644),(#26645,#26646),(#26647,#26648),
(#26649,#26650),(#26651,#26652),(#26653,#26654),(#26655,#26656),(#26657,
#26658),(#26659,#26660),(#26661,#26662),(#26663,#26664),(#26665,#26666),
(#26667,#26668),(#26669,#26670),(#26671,#26672),(#26673,#26674),(#26675,
#26676),(#26677,#26678),(#26679,#26680),(#26681,#26682)),.UNSPECIFIED.,
 .F.,.F.,.F.)
B_SPLINE_SURFACE_WITH_KNOTS((6,1,1,1,1,1,1,1,1,1,1,1,1,1,1,1,1,1,1,1,1,
1,1,1,1,1,1,1,1,1,1,1,1,1,1,1,1,1,1,1,1,1,1,1,1,1,1,1,1,1,1,1,1,1,1,1,1,
1,1,1,1,1,1,1,1,6),(2,2),(-1.,-0.984615384615383,-0.969230769230768,-0.953846153846152,
-0.938461538461537,-0.923076923076922,-0.907692307692306,-0.892307692307691,
-0.876923076923076,-0.86153846153846,-0.846153846153845,-0.83076923076923,
-0.815384615384614,-0.799999999999999,-0.784615384615384,-0.769230769230768,
-0.753846153846153,-0.738461538461538,-0.723076923076922,-0.707692307692307,
-0.692307692307692,-0.676923076923076,-0.661538461538461,-0.646153846153846,
-0.63076923076923,-0.615384615384615,-0.6,-0.584615384615384,-0.569230769230769,
-0.553846153846154,-0.538461538461538,-0.523076923076923,-0.507692307692308,
-0.492307692307692,-0.476923076923077,-0.461538461538462,-0.446153846153846,
-0.430769230769231,-0.415384615384615,-0.4,-0.384615384615385,-0.369230769230769,
-0.353846153846154,-0.338461538461538,-0.323076923076923,-0.307692307692308,
-0.292307692307692,-0.276923076923077,-0.261538461538462,-0.246153846153846,
-0.230769230769231,-0.215384615384615,-0.2,-0.184615384615385,-0.169230769230769,
-0.153846153846154,-0.138461538461538,-0.123076923076923,-0.107692307692308,
-0.0923076923076923,-0.0769230769230769,-0.0615384615384615,-0.0461538461538462,
-0.0307692307692308,-0.0153846153846154,0.),(-1.,1.),.UNSPECIFIED.)
GEOMETRIC_REPRESENTATION_ITEM()
RATIONAL_B_SPLINE_SURFACE(((1.,1.),(1.,1.),(1.,1.),(1.,1.),(1.,1.),(1.,
1.),(1.,1.),(1.,1.),(1.,1.),(1.,1.),(1.,1.),(1.,1.),(1.,1.),(1.,1.),(1.,
1.),(1.,1.),(1.,1.),(1.,1.),(1.,1.),(1.,1.),(1.,1.),(1.,1.),(1.,1.),(1.,
1.),(1.,1.),(1.,1.),(1.,1.),(1.,1.),(1.,1.),(1.,1.),(1.,1.),(1.,1.),(1.,
1.),(1.,1.),(1.,1.),(1.,1.),(1.,1.),(1.,1.),(1.,1.),(1.,1.),(1.,1.),(1.,
1.),(1.,1.),(1.,1.),(1.,1.),(1.,1.),(1.,1.),(1.,1.),(1.,1.),(1.,1.),(1.,
1.),(1.,1.),(1.,1.),(1.,1.),(1.,1.),(1.,1.),(1.,1.),(1.,1.),(1.,1.),(1.,
1.),(1.,1.),(1.,1.),(1.,1.),(1.,1.),(1.,1.),(1.,1.),(1.,1.),(1.,1.),(1.,
1.),(1.,1.)))
REPRESENTATION_ITEM('')
SURFACE()
);
#37=(
BOUNDED_SURFACE()
B_SPLINE_SURFACE(5,1,((#26759,#26760),(#26761,#26762),(#26763,#26764),(#26765,
#26766),(#26767,#26768),(#26769,#26770),(#26771,#26772),(#26773,#26774),
(#26775,#26776),(#26777,#26778),(#26779,#26780),(#26781,#26782),(#26783,
#26784),(#26785,#26786),(#26787,#26788),(#26789,#26790),(#26791,#26792),
(#26793,#26794),(#26795,#26796),(#26797,#26798),(#26799,#26800),(#26801,
#26802),(#26803,#26804),(#26805,#26806),(#26807,#26808),(#26809,#26810),
(#26811,#26812),(#26813,#26814),(#26815,#26816),(#26817,#26818),(#26819,
#26820),(#26821,#26822),(#26823,#26824),(#26825,#26826),(#26827,#26828),
(#26829,#26830),(#26831,#26832),(#26833,#26834),(#26835,#26836),(#26837,
#26838),(#26839,#26840),(#26841,#26842),(#26843,#26844),(#26845,#26846),
(#26847,#26848),(#26849,#26850),(#26851,#26852),(#26853,#26854),(#26855,
#26856),(#26857,#26858),(#26859,#26860),(#26861,#26862),(#26863,#26864),
(#26865,#26866),(#26867,#26868),(#26869,#26870),(#26871,#26872),(#26873,
#26874),(#26875,#26876),(#26877,#26878),(#26879,#26880),(#26881,#26882),
(#26883,#26884),(#26885,#26886),(#26887,#26888),(#26889,#26890),(#26891,
#26892),(#26893,#26894),(#26895,#26896),(#26897,#26898)),.UNSPECIFIED.,
 .F.,.F.,.F.)
B_SPLINE_SURFACE_WITH_KNOTS((6,1,1,1,1,1,1,1,1,1,1,1,1,1,1,1,1,1,1,1,1,
1,1,1,1,1,1,1,1,1,1,1,1,1,1,1,1,1,1,1,1,1,1,1,1,1,1,1,1,1,1,1,1,1,1,1,1,
1,1,1,1,1,1,1,1,6),(2,2),(-1.,-0.984615384615383,-0.969230769230768,-0.953846153846152,
-0.938461538461537,-0.923076923076922,-0.907692307692306,-0.892307692307691,
-0.876923076923076,-0.86153846153846,-0.846153846153845,-0.83076923076923,
-0.815384615384614,-0.799999999999999,-0.784615384615384,-0.769230769230768,
-0.753846153846153,-0.738461538461538,-0.723076923076922,-0.707692307692307,
-0.692307692307692,-0.676923076923076,-0.661538461538461,-0.646153846153846,
-0.63076923076923,-0.615384615384615,-0.6,-0.584615384615384,-0.569230769230769,
-0.553846153846154,-0.538461538461538,-0.523076923076923,-0.507692307692308,
-0.492307692307692,-0.476923076923077,-0.461538461538462,-0.446153846153846,
-0.430769230769231,-0.415384615384615,-0.4,-0.384615384615385,-0.369230769230769,
-0.353846153846154,-0.338461538461538,-0.323076923076923,-0.307692307692308,
-0.292307692307692,-0.276923076923077,-0.261538461538462,-0.246153846153846,
-0.230769230769231,-0.215384615384615,-0.2,-0.184615384615385,-0.169230769230769,
-0.153846153846154,-0.138461538461538,-0.123076923076923,-0.107692307692308,
-0.0923076923076923,-0.0769230769230769,-0.0615384615384615,-0.0461538461538462,
-0.0307692307692308,-0.0153846153846154,0.),(-1.,1.),.UNSPECIFIED.)
GEOMETRIC_REPRESENTATION_ITEM()
RATIONAL_B_SPLINE_SURFACE(((1.,1.),(1.,1.),(1.,1.),(1.,1.),(1.,1.),(1.,
1.),(1.,1.),(1.,1.),(1.,1.),(1.,1.),(1.,1.),(1.,1.),(1.,1.),(1.,1.),(1.,
1.),(1.,1.),(1.,1.),(1.,1.),(1.,1.),(1.,1.),(1.,1.),(1.,1.),(1.,1.),(1.,
1.),(1.,1.),(1.,1.),(1.,1.),(1.,1.),(1.,1.),(1.,1.),(1.,1.),(1.,1.),(1.,
1.),(1.,1.),(1.,1.),(1.,1.),(1.,1.),(1.,1.),(1.,1.),(1.,1.),(1.,1.),(1.,
1.),(1.,1.),(1.,1.),(1.,1.),(1.,1.),(1.,1.),(1.,1.),(1.,1.),(1.,1.),(1.,
1.),(1.,1.),(1.,1.),(1.,1.),(1.,1.),(1.,1.),(1.,1.),(1.,1.),(1.,1.),(1.,
1.),(1.,1.),(1.,1.),(1.,1.),(1.,1.),(1.,1.),(1.,1.),(1.,1.),(1.,1.),(1.,
1.),(1.,1.)))
REPRESENTATION_ITEM('')
SURFACE()
);
#38=(
BOUNDED_SURFACE()
B_SPLINE_SURFACE(5,1,((#26975,#26976),(#26977,#26978),(#26979,#26980),(#26981,
#26982),(#26983,#26984),(#26985,#26986),(#26987,#26988),(#26989,#26990),
(#26991,#26992),(#26993,#26994),(#26995,#26996),(#26997,#26998),(#26999,
#27000),(#27001,#27002),(#27003,#27004),(#27005,#27006),(#27007,#27008),
(#27009,#27010),(#27011,#27012),(#27013,#27014),(#27015,#27016),(#27017,
#27018),(#27019,#27020),(#27021,#27022),(#27023,#27024),(#27025,#27026),
(#27027,#27028),(#27029,#27030),(#27031,#27032),(#27033,#27034),(#27035,
#27036),(#27037,#27038),(#27039,#27040),(#27041,#27042),(#27043,#27044),
(#27045,#27046),(#27047,#27048),(#27049,#27050),(#27051,#27052),(#27053,
#27054),(#27055,#27056),(#27057,#27058),(#27059,#27060),(#27061,#27062),
(#27063,#27064),(#27065,#27066),(#27067,#27068),(#27069,#27070),(#27071,
#27072),(#27073,#27074),(#27075,#27076),(#27077,#27078),(#27079,#27080),
(#27081,#27082),(#27083,#27084),(#27085,#27086),(#27087,#27088),(#27089,
#27090),(#27091,#27092),(#27093,#27094),(#27095,#27096),(#27097,#27098),
(#27099,#27100),(#27101,#27102),(#27103,#27104),(#27105,#27106),(#27107,
#27108),(#27109,#27110),(#27111,#27112),(#27113,#27114)),.UNSPECIFIED.,
 .F.,.F.,.F.)
B_SPLINE_SURFACE_WITH_KNOTS((6,1,1,1,1,1,1,1,1,1,1,1,1,1,1,1,1,1,1,1,1,
1,1,1,1,1,1,1,1,1,1,1,1,1,1,1,1,1,1,1,1,1,1,1,1,1,1,1,1,1,1,1,1,1,1,1,1,
1,1,1,1,1,1,1,1,6),(2,2),(-1.,-0.984615384615383,-0.969230769230768,-0.953846153846152,
-0.938461538461537,-0.923076923076922,-0.907692307692306,-0.892307692307691,
-0.876923076923076,-0.86153846153846,-0.846153846153845,-0.83076923076923,
-0.815384615384614,-0.799999999999999,-0.784615384615384,-0.769230769230768,
-0.753846153846153,-0.738461538461538,-0.723076923076922,-0.707692307692307,
-0.692307692307692,-0.676923076923076,-0.661538461538461,-0.646153846153846,
-0.63076923076923,-0.615384615384615,-0.6,-0.584615384615384,-0.569230769230769,
-0.553846153846154,-0.538461538461538,-0.523076923076923,-0.507692307692308,
-0.492307692307692,-0.476923076923077,-0.461538461538462,-0.446153846153846,
-0.430769230769231,-0.415384615384615,-0.4,-0.384615384615385,-0.369230769230769,
-0.353846153846154,-0.338461538461538,-0.323076923076923,-0.307692307692308,
-0.292307692307692,-0.276923076923077,-0.261538461538462,-0.246153846153846,
-0.230769230769231,-0.215384615384615,-0.2,-0.184615384615385,-0.169230769230769,
-0.153846153846154,-0.138461538461538,-0.123076923076923,-0.107692307692308,
-0.0923076923076923,-0.0769230769230769,-0.0615384615384615,-0.0461538461538462,
-0.0307692307692308,-0.0153846153846154,0.),(-1.,1.),.UNSPECIFIED.)
GEOMETRIC_REPRESENTATION_ITEM()
RATIONAL_B_SPLINE_SURFACE(((1.,1.),(1.,1.),(1.,1.),(1.,1.),(1.,1.),(1.,
1.),(1.,1.),(1.,1.),(1.,1.),(1.,1.),(1.,1.),(1.,1.),(1.,1.),(1.,1.),(1.,
1.),(1.,1.),(1.,1.),(1.,1.),(1.,1.),(1.,1.),(1.,1.),(1.,1.),(1.,1.),(1.,
1.),(1.,1.),(1.,1.),(1.,1.),(1.,1.),(1.,1.),(1.,1.),(1.,1.),(1.,1.),(1.,
1.),(1.,1.),(1.,1.),(1.,1.),(1.,1.),(1.,1.),(1.,1.),(1.,1.),(1.,1.),(1.,
1.),(1.,1.),(1.,1.),(1.,1.),(1.,1.),(1.,1.),(1.,1.),(1.,1.),(1.,1.),(1.,
1.),(1.,1.),(1.,1.),(1.,1.),(1.,1.),(1.,1.),(1.,1.),(1.,1.),(1.,1.),(1.,
1.),(1.,1.),(1.,1.),(1.,1.),(1.,1.),(1.,1.),(1.,1.),(1.,1.),(1.,1.),(1.,
1.),(1.,1.)))
REPRESENTATION_ITEM('')
SURFACE()
);
#39=(
BOUNDED_SURFACE()
B_SPLINE_SURFACE(5,1,((#27191,#27192),(#27193,#27194),(#27195,#27196),(#27197,
#27198),(#27199,#27200),(#27201,#27202),(#27203,#27204),(#27205,#27206),
(#27207,#27208),(#27209,#27210),(#27211,#27212),(#27213,#27214),(#27215,
#27216),(#27217,#27218),(#27219,#27220),(#27221,#27222),(#27223,#27224),
(#27225,#27226),(#27227,#27228),(#27229,#27230),(#27231,#27232),(#27233,
#27234),(#27235,#27236),(#27237,#27238),(#27239,#27240),(#27241,#27242),
(#27243,#27244),(#27245,#27246),(#27247,#27248),(#27249,#27250),(#27251,
#27252),(#27253,#27254),(#27255,#27256),(#27257,#27258),(#27259,#27260),
(#27261,#27262),(#27263,#27264),(#27265,#27266),(#27267,#27268),(#27269,
#27270),(#27271,#27272),(#27273,#27274),(#27275,#27276),(#27277,#27278),
(#27279,#27280),(#27281,#27282),(#27283,#27284),(#27285,#27286),(#27287,
#27288),(#27289,#27290),(#27291,#27292),(#27293,#27294),(#27295,#27296),
(#27297,#27298),(#27299,#27300),(#27301,#27302),(#27303,#27304),(#27305,
#27306),(#27307,#27308),(#27309,#27310),(#27311,#27312),(#27313,#27314),
(#27315,#27316),(#27317,#27318),(#27319,#27320),(#27321,#27322),(#27323,
#27324),(#27325,#27326),(#27327,#27328),(#27329,#27330)),.UNSPECIFIED.,
 .F.,.F.,.F.)
B_SPLINE_SURFACE_WITH_KNOTS((6,1,1,1,1,1,1,1,1,1,1,1,1,1,1,1,1,1,1,1,1,
1,1,1,1,1,1,1,1,1,1,1,1,1,1,1,1,1,1,1,1,1,1,1,1,1,1,1,1,1,1,1,1,1,1,1,1,
1,1,1,1,1,1,1,1,6),(2,2),(-1.,-0.984615384615383,-0.969230769230768,-0.953846153846152,
-0.938461538461537,-0.923076923076922,-0.907692307692306,-0.892307692307691,
-0.876923076923076,-0.86153846153846,-0.846153846153845,-0.83076923076923,
-0.815384615384614,-0.799999999999999,-0.784615384615384,-0.769230769230768,
-0.753846153846153,-0.738461538461538,-0.723076923076922,-0.707692307692307,
-0.692307692307692,-0.676923076923076,-0.661538461538461,-0.646153846153846,
-0.63076923076923,-0.615384615384615,-0.6,-0.584615384615384,-0.569230769230769,
-0.553846153846154,-0.538461538461538,-0.523076923076923,-0.507692307692308,
-0.492307692307692,-0.476923076923077,-0.461538461538462,-0.446153846153846,
-0.430769230769231,-0.415384615384615,-0.4,-0.384615384615385,-0.369230769230769,
-0.353846153846154,-0.338461538461538,-0.323076923076923,-0.307692307692308,
-0.292307692307692,-0.276923076923077,-0.261538461538462,-0.246153846153846,
-0.230769230769231,-0.215384615384615,-0.2,-0.184615384615385,-0.169230769230769,
-0.153846153846154,-0.138461538461538,-0.123076923076923,-0.107692307692308,
-0.0923076923076923,-0.0769230769230769,-0.0615384615384615,-0.0461538461538462,
-0.0307692307692308,-0.0153846153846154,0.),(-1.,1.),.UNSPECIFIED.)
GEOMETRIC_REPRESENTATION_ITEM()
RATIONAL_B_SPLINE_SURFACE(((1.,1.),(1.,1.),(1.,1.),(1.,1.),(1.,1.),(1.,
1.),(1.,1.),(1.,1.),(1.,1.),(1.,1.),(1.,1.),(1.,1.),(1.,1.),(1.,1.),(1.,
1.),(1.,1.),(1.,1.),(1.,1.),(1.,1.),(1.,1.),(1.,1.),(1.,1.),(1.,1.),(1.,
1.),(1.,1.),(1.,1.),(1.,1.),(1.,1.),(1.,1.),(1.,1.),(1.,1.),(1.,1.),(1.,
1.),(1.,1.),(1.,1.),(1.,1.),(1.,1.),(1.,1.),(1.,1.),(1.,1.),(1.,1.),(1.,
1.),(1.,1.),(1.,1.),(1.,1.),(1.,1.),(1.,1.),(1.,1.),(1.,1.),(1.,1.),(1.,
1.),(1.,1.),(1.,1.),(1.,1.),(1.,1.),(1.,1.),(1.,1.),(1.,1.),(1.,1.),(1.,
1.),(1.,1.),(1.,1.),(1.,1.),(1.,1.),(1.,1.),(1.,1.),(1.,1.),(1.,1.),(1.,
1.),(1.,1.)))
REPRESENTATION_ITEM('')
SURFACE()
);
#40=(
BOUNDED_SURFACE()
B_SPLINE_SURFACE(5,1,((#27407,#27408),(#27409,#27410),(#27411,#27412),(#27413,
#27414),(#27415,#27416),(#27417,#27418),(#27419,#27420),(#27421,#27422),
(#27423,#27424),(#27425,#27426),(#27427,#27428),(#27429,#27430),(#27431,
#27432),(#27433,#27434),(#27435,#27436),(#27437,#27438),(#27439,#27440),
(#27441,#27442),(#27443,#27444),(#27445,#27446),(#27447,#27448),(#27449,
#27450),(#27451,#27452),(#27453,#27454),(#27455,#27456),(#27457,#27458),
(#27459,#27460),(#27461,#27462),(#27463,#27464),(#27465,#27466),(#27467,
#27468),(#27469,#27470),(#27471,#27472),(#27473,#27474),(#27475,#27476),
(#27477,#27478),(#27479,#27480),(#27481,#27482),(#27483,#27484),(#27485,
#27486),(#27487,#27488),(#27489,#27490),(#27491,#27492),(#27493,#27494),
(#27495,#27496),(#27497,#27498),(#27499,#27500),(#27501,#27502),(#27503,
#27504),(#27505,#27506),(#27507,#27508),(#27509,#27510),(#27511,#27512),
(#27513,#27514),(#27515,#27516),(#27517,#27518),(#27519,#27520),(#27521,
#27522),(#27523,#27524),(#27525,#27526),(#27527,#27528),(#27529,#27530),
(#27531,#27532),(#27533,#27534),(#27535,#27536),(#27537,#27538),(#27539,
#27540),(#27541,#27542),(#27543,#27544),(#27545,#27546)),.UNSPECIFIED.,
 .F.,.F.,.F.)
B_SPLINE_SURFACE_WITH_KNOTS((6,1,1,1,1,1,1,1,1,1,1,1,1,1,1,1,1,1,1,1,1,
1,1,1,1,1,1,1,1,1,1,1,1,1,1,1,1,1,1,1,1,1,1,1,1,1,1,1,1,1,1,1,1,1,1,1,1,
1,1,1,1,1,1,1,1,6),(2,2),(-1.,-0.984615384615383,-0.969230769230768,-0.953846153846152,
-0.938461538461537,-0.923076923076922,-0.907692307692306,-0.892307692307691,
-0.876923076923076,-0.86153846153846,-0.846153846153845,-0.83076923076923,
-0.815384615384614,-0.799999999999999,-0.784615384615384,-0.769230769230768,
-0.753846153846153,-0.738461538461538,-0.723076923076922,-0.707692307692307,
-0.692307692307692,-0.676923076923076,-0.661538461538461,-0.646153846153846,
-0.63076923076923,-0.615384615384615,-0.6,-0.584615384615384,-0.569230769230769,
-0.553846153846154,-0.538461538461538,-0.523076923076923,-0.507692307692308,
-0.492307692307692,-0.476923076923077,-0.461538461538462,-0.446153846153846,
-0.430769230769231,-0.415384615384615,-0.4,-0.384615384615385,-0.369230769230769,
-0.353846153846154,-0.338461538461538,-0.323076923076923,-0.307692307692308,
-0.292307692307692,-0.276923076923077,-0.261538461538462,-0.246153846153846,
-0.230769230769231,-0.215384615384615,-0.2,-0.184615384615385,-0.169230769230769,
-0.153846153846154,-0.138461538461538,-0.123076923076923,-0.107692307692308,
-0.0923076923076923,-0.0769230769230769,-0.0615384615384615,-0.0461538461538462,
-0.0307692307692308,-0.0153846153846154,0.),(-1.,1.),.UNSPECIFIED.)
GEOMETRIC_REPRESENTATION_ITEM()
RATIONAL_B_SPLINE_SURFACE(((1.,1.),(1.,1.),(1.,1.),(1.,1.),(1.,1.),(1.,
1.),(1.,1.),(1.,1.),(1.,1.),(1.,1.),(1.,1.),(1.,1.),(1.,1.),(1.,1.),(1.,
1.),(1.,1.),(1.,1.),(1.,1.),(1.,1.),(1.,1.),(1.,1.),(1.,1.),(1.,1.),(1.,
1.),(1.,1.),(1.,1.),(1.,1.),(1.,1.),(1.,1.),(1.,1.),(1.,1.),(1.,1.),(1.,
1.),(1.,1.),(1.,1.),(1.,1.),(1.,1.),(1.,1.),(1.,1.),(1.,1.),(1.,1.),(1.,
1.),(1.,1.),(1.,1.),(1.,1.),(1.,1.),(1.,1.),(1.,1.),(1.,1.),(1.,1.),(1.,
1.),(1.,1.),(1.,1.),(1.,1.),(1.,1.),(1.,1.),(1.,1.),(1.,1.),(1.,1.),(1.,
1.),(1.,1.),(1.,1.),(1.,1.),(1.,1.),(1.,1.),(1.,1.),(1.,1.),(1.,1.),(1.,
1.),(1.,1.)))
REPRESENTATION_ITEM('')
SURFACE()
);
#41=(
BOUNDED_SURFACE()
B_SPLINE_SURFACE(5,1,((#27623,#27624),(#27625,#27626),(#27627,#27628),(#27629,
#27630),(#27631,#27632),(#27633,#27634),(#27635,#27636),(#27637,#27638),
(#27639,#27640),(#27641,#27642),(#27643,#27644),(#27645,#27646),(#27647,
#27648),(#27649,#27650),(#27651,#27652),(#27653,#27654),(#27655,#27656),
(#27657,#27658),(#27659,#27660),(#27661,#27662),(#27663,#27664),(#27665,
#27666),(#27667,#27668),(#27669,#27670),(#27671,#27672),(#27673,#27674),
(#27675,#27676),(#27677,#27678),(#27679,#27680),(#27681,#27682),(#27683,
#27684),(#27685,#27686),(#27687,#27688),(#27689,#27690),(#27691,#27692),
(#27693,#27694),(#27695,#27696),(#27697,#27698),(#27699,#27700),(#27701,
#27702),(#27703,#27704),(#27705,#27706),(#27707,#27708),(#27709,#27710),
(#27711,#27712),(#27713,#27714),(#27715,#27716),(#27717,#27718),(#27719,
#27720),(#27721,#27722),(#27723,#27724),(#27725,#27726),(#27727,#27728),
(#27729,#27730),(#27731,#27732),(#27733,#27734),(#27735,#27736),(#27737,
#27738),(#27739,#27740),(#27741,#27742),(#27743,#27744),(#27745,#27746),
(#27747,#27748),(#27749,#27750),(#27751,#27752),(#27753,#27754),(#27755,
#27756),(#27757,#27758),(#27759,#27760),(#27761,#27762)),.UNSPECIFIED.,
 .F.,.F.,.F.)
B_SPLINE_SURFACE_WITH_KNOTS((6,1,1,1,1,1,1,1,1,1,1,1,1,1,1,1,1,1,1,1,1,
1,1,1,1,1,1,1,1,1,1,1,1,1,1,1,1,1,1,1,1,1,1,1,1,1,1,1,1,1,1,1,1,1,1,1,1,
1,1,1,1,1,1,1,1,6),(2,2),(-1.,-0.984615384615383,-0.969230769230768,-0.953846153846152,
-0.938461538461537,-0.923076923076922,-0.907692307692306,-0.892307692307691,
-0.876923076923076,-0.86153846153846,-0.846153846153845,-0.83076923076923,
-0.815384615384614,-0.799999999999999,-0.784615384615384,-0.769230769230768,
-0.753846153846153,-0.738461538461538,-0.723076923076922,-0.707692307692307,
-0.692307692307692,-0.676923076923076,-0.661538461538461,-0.646153846153846,
-0.63076923076923,-0.615384615384615,-0.6,-0.584615384615384,-0.569230769230769,
-0.553846153846154,-0.538461538461538,-0.523076923076923,-0.507692307692308,
-0.492307692307692,-0.476923076923077,-0.461538461538462,-0.446153846153846,
-0.430769230769231,-0.415384615384615,-0.4,-0.384615384615385,-0.369230769230769,
-0.353846153846154,-0.338461538461538,-0.323076923076923,-0.307692307692308,
-0.292307692307692,-0.276923076923077,-0.261538461538462,-0.246153846153846,
-0.230769230769231,-0.215384615384615,-0.2,-0.184615384615385,-0.169230769230769,
-0.153846153846154,-0.138461538461538,-0.123076923076923,-0.107692307692308,
-0.0923076923076923,-0.0769230769230769,-0.0615384615384615,-0.0461538461538462,
-0.0307692307692308,-0.0153846153846154,0.),(-1.,1.),.UNSPECIFIED.)
GEOMETRIC_REPRESENTATION_ITEM()
RATIONAL_B_SPLINE_SURFACE(((1.,1.),(1.,1.),(1.,1.),(1.,1.),(1.,1.),(1.,
1.),(1.,1.),(1.,1.),(1.,1.),(1.,1.),(1.,1.),(1.,1.),(1.,1.),(1.,1.),(1.,
1.),(1.,1.),(1.,1.),(1.,1.),(1.,1.),(1.,1.),(1.,1.),(1.,1.),(1.,1.),(1.,
1.),(1.,1.),(1.,1.),(1.,1.),(1.,1.),(1.,1.),(1.,1.),(1.,1.),(1.,1.),(1.,
1.),(1.,1.),(1.,1.),(1.,1.),(1.,1.),(1.,1.),(1.,1.),(1.,1.),(1.,1.),(1.,
1.),(1.,1.),(1.,1.),(1.,1.),(1.,1.),(1.,1.),(1.,1.),(1.,1.),(1.,1.),(1.,
1.),(1.,1.),(1.,1.),(1.,1.),(1.,1.),(1.,1.),(1.,1.),(1.,1.),(1.,1.),(1.,
1.),(1.,1.),(1.,1.),(1.,1.),(1.,1.),(1.,1.),(1.,1.),(1.,1.),(1.,1.),(1.,
1.),(1.,1.)))
REPRESENTATION_ITEM('')
SURFACE()
);
#42=(
BOUNDED_SURFACE()
B_SPLINE_SURFACE(5,1,((#27839,#27840),(#27841,#27842),(#27843,#27844),(#27845,
#27846),(#27847,#27848),(#27849,#27850),(#27851,#27852),(#27853,#27854),
(#27855,#27856),(#27857,#27858),(#27859,#27860),(#27861,#27862),(#27863,
#27864),(#27865,#27866),(#27867,#27868),(#27869,#27870),(#27871,#27872),
(#27873,#27874),(#27875,#27876),(#27877,#27878),(#27879,#27880),(#27881,
#27882),(#27883,#27884),(#27885,#27886),(#27887,#27888),(#27889,#27890),
(#27891,#27892),(#27893,#27894),(#27895,#27896),(#27897,#27898),(#27899,
#27900),(#27901,#27902),(#27903,#27904),(#27905,#27906),(#27907,#27908),
(#27909,#27910),(#27911,#27912),(#27913,#27914),(#27915,#27916),(#27917,
#27918),(#27919,#27920),(#27921,#27922),(#27923,#27924),(#27925,#27926),
(#27927,#27928),(#27929,#27930),(#27931,#27932),(#27933,#27934),(#27935,
#27936),(#27937,#27938),(#27939,#27940),(#27941,#27942),(#27943,#27944),
(#27945,#27946),(#27947,#27948),(#27949,#27950),(#27951,#27952),(#27953,
#27954),(#27955,#27956),(#27957,#27958),(#27959,#27960),(#27961,#27962),
(#27963,#27964),(#27965,#27966),(#27967,#27968),(#27969,#27970),(#27971,
#27972),(#27973,#27974),(#27975,#27976),(#27977,#27978)),.UNSPECIFIED.,
 .F.,.F.,.F.)
B_SPLINE_SURFACE_WITH_KNOTS((6,1,1,1,1,1,1,1,1,1,1,1,1,1,1,1,1,1,1,1,1,
1,1,1,1,1,1,1,1,1,1,1,1,1,1,1,1,1,1,1,1,1,1,1,1,1,1,1,1,1,1,1,1,1,1,1,1,
1,1,1,1,1,1,1,1,6),(2,2),(-1.,-0.984615384615383,-0.969230769230768,-0.953846153846152,
-0.938461538461537,-0.923076923076922,-0.907692307692306,-0.892307692307691,
-0.876923076923076,-0.86153846153846,-0.846153846153845,-0.83076923076923,
-0.815384615384614,-0.799999999999999,-0.784615384615384,-0.769230769230768,
-0.753846153846153,-0.738461538461538,-0.723076923076922,-0.707692307692307,
-0.692307692307692,-0.676923076923076,-0.661538461538461,-0.646153846153846,
-0.63076923076923,-0.615384615384615,-0.6,-0.584615384615384,-0.569230769230769,
-0.553846153846154,-0.538461538461538,-0.523076923076923,-0.507692307692308,
-0.492307692307692,-0.476923076923077,-0.461538461538462,-0.446153846153846,
-0.430769230769231,-0.415384615384615,-0.4,-0.384615384615385,-0.369230769230769,
-0.353846153846154,-0.338461538461538,-0.323076923076923,-0.307692307692308,
-0.292307692307692,-0.276923076923077,-0.261538461538462,-0.246153846153846,
-0.230769230769231,-0.215384615384615,-0.2,-0.184615384615385,-0.169230769230769,
-0.153846153846154,-0.138461538461538,-0.123076923076923,-0.107692307692308,
-0.0923076923076923,-0.0769230769230769,-0.0615384615384615,-0.0461538461538462,
-0.0307692307692308,-0.0153846153846154,0.),(-1.,1.),.UNSPECIFIED.)
GEOMETRIC_REPRESENTATION_ITEM()
RATIONAL_B_SPLINE_SURFACE(((1.,1.),(1.,1.),(1.,1.),(1.,1.),(1.,1.),(1.,
1.),(1.,1.),(1.,1.),(1.,1.),(1.,1.),(1.,1.),(1.,1.),(1.,1.),(1.,1.),(1.,
1.),(1.,1.),(1.,1.),(1.,1.),(1.,1.),(1.,1.),(1.,1.),(1.,1.),(1.,1.),(1.,
1.),(1.,1.),(1.,1.),(1.,1.),(1.,1.),(1.,1.),(1.,1.),(1.,1.),(1.,1.),(1.,
1.),(1.,1.),(1.,1.),(1.,1.),(1.,1.),(1.,1.),(1.,1.),(1.,1.),(1.,1.),(1.,
1.),(1.,1.),(1.,1.),(1.,1.),(1.,1.),(1.,1.),(1.,1.),(1.,1.),(1.,1.),(1.,
1.),(1.,1.),(1.,1.),(1.,1.),(1.,1.),(1.,1.),(1.,1.),(1.,1.),(1.,1.),(1.,
1.),(1.,1.),(1.,1.),(1.,1.),(1.,1.),(1.,1.),(1.,1.),(1.,1.),(1.,1.),(1.,
1.),(1.,1.)))
REPRESENTATION_ITEM('')
SURFACE()
);
#43=(
BOUNDED_SURFACE()
B_SPLINE_SURFACE(5,1,((#28055,#28056),(#28057,#28058),(#28059,#28060),(#28061,
#28062),(#28063,#28064),(#28065,#28066),(#28067,#28068),(#28069,#28070),
(#28071,#28072),(#28073,#28074),(#28075,#28076),(#28077,#28078),(#28079,
#28080),(#28081,#28082),(#28083,#28084),(#28085,#28086),(#28087,#28088),
(#28089,#28090),(#28091,#28092),(#28093,#28094),(#28095,#28096),(#28097,
#28098),(#28099,#28100),(#28101,#28102),(#28103,#28104),(#28105,#28106),
(#28107,#28108),(#28109,#28110),(#28111,#28112),(#28113,#28114),(#28115,
#28116),(#28117,#28118),(#28119,#28120),(#28121,#28122),(#28123,#28124),
(#28125,#28126),(#28127,#28128),(#28129,#28130),(#28131,#28132),(#28133,
#28134),(#28135,#28136),(#28137,#28138),(#28139,#28140),(#28141,#28142),
(#28143,#28144),(#28145,#28146),(#28147,#28148),(#28149,#28150),(#28151,
#28152),(#28153,#28154),(#28155,#28156),(#28157,#28158),(#28159,#28160),
(#28161,#28162),(#28163,#28164),(#28165,#28166),(#28167,#28168),(#28169,
#28170),(#28171,#28172),(#28173,#28174),(#28175,#28176),(#28177,#28178),
(#28179,#28180),(#28181,#28182),(#28183,#28184),(#28185,#28186),(#28187,
#28188),(#28189,#28190),(#28191,#28192),(#28193,#28194)),.UNSPECIFIED.,
 .F.,.F.,.F.)
B_SPLINE_SURFACE_WITH_KNOTS((6,1,1,1,1,1,1,1,1,1,1,1,1,1,1,1,1,1,1,1,1,
1,1,1,1,1,1,1,1,1,1,1,1,1,1,1,1,1,1,1,1,1,1,1,1,1,1,1,1,1,1,1,1,1,1,1,1,
1,1,1,1,1,1,1,1,6),(2,2),(-1.,-0.984615384615383,-0.969230769230768,-0.953846153846152,
-0.938461538461537,-0.923076923076922,-0.907692307692306,-0.892307692307691,
-0.876923076923076,-0.86153846153846,-0.846153846153845,-0.83076923076923,
-0.815384615384614,-0.799999999999999,-0.784615384615384,-0.769230769230768,
-0.753846153846153,-0.738461538461538,-0.723076923076922,-0.707692307692307,
-0.692307692307692,-0.676923076923076,-0.661538461538461,-0.646153846153846,
-0.63076923076923,-0.615384615384615,-0.6,-0.584615384615384,-0.569230769230769,
-0.553846153846154,-0.538461538461538,-0.523076923076923,-0.507692307692308,
-0.492307692307692,-0.476923076923077,-0.461538461538462,-0.446153846153846,
-0.430769230769231,-0.415384615384615,-0.4,-0.384615384615385,-0.369230769230769,
-0.353846153846154,-0.338461538461538,-0.323076923076923,-0.307692307692308,
-0.292307692307692,-0.276923076923077,-0.261538461538462,-0.246153846153846,
-0.230769230769231,-0.215384615384615,-0.2,-0.184615384615385,-0.169230769230769,
-0.153846153846154,-0.138461538461538,-0.123076923076923,-0.107692307692308,
-0.0923076923076923,-0.0769230769230769,-0.0615384615384615,-0.0461538461538462,
-0.0307692307692308,-0.0153846153846154,0.),(-1.,1.),.UNSPECIFIED.)
GEOMETRIC_REPRESENTATION_ITEM()
RATIONAL_B_SPLINE_SURFACE(((1.,1.),(1.,1.),(1.,1.),(1.,1.),(1.,1.),(1.,
1.),(1.,1.),(1.,1.),(1.,1.),(1.,1.),(1.,1.),(1.,1.),(1.,1.),(1.,1.),(1.,
1.),(1.,1.),(1.,1.),(1.,1.),(1.,1.),(1.,1.),(1.,1.),(1.,1.),(1.,1.),(1.,
1.),(1.,1.),(1.,1.),(1.,1.),(1.,1.),(1.,1.),(1.,1.),(1.,1.),(1.,1.),(1.,
1.),(1.,1.),(1.,1.),(1.,1.),(1.,1.),(1.,1.),(1.,1.),(1.,1.),(1.,1.),(1.,
1.),(1.,1.),(1.,1.),(1.,1.),(1.,1.),(1.,1.),(1.,1.),(1.,1.),(1.,1.),(1.,
1.),(1.,1.),(1.,1.),(1.,1.),(1.,1.),(1.,1.),(1.,1.),(1.,1.),(1.,1.),(1.,
1.),(1.,1.),(1.,1.),(1.,1.),(1.,1.),(1.,1.),(1.,1.),(1.,1.),(1.,1.),(1.,
1.),(1.,1.)))
REPRESENTATION_ITEM('')
SURFACE()
);
#44=(
BOUNDED_SURFACE()
B_SPLINE_SURFACE(5,1,((#28271,#28272),(#28273,#28274),(#28275,#28276),(#28277,
#28278),(#28279,#28280),(#28281,#28282),(#28283,#28284),(#28285,#28286),
(#28287,#28288),(#28289,#28290),(#28291,#28292),(#28293,#28294),(#28295,
#28296),(#28297,#28298),(#28299,#28300),(#28301,#28302),(#28303,#28304),
(#28305,#28306),(#28307,#28308),(#28309,#28310),(#28311,#28312),(#28313,
#28314),(#28315,#28316),(#28317,#28318),(#28319,#28320),(#28321,#28322),
(#28323,#28324),(#28325,#28326),(#28327,#28328),(#28329,#28330),(#28331,
#28332),(#28333,#28334),(#28335,#28336),(#28337,#28338),(#28339,#28340),
(#28341,#28342),(#28343,#28344),(#28345,#28346),(#28347,#28348),(#28349,
#28350),(#28351,#28352),(#28353,#28354),(#28355,#28356),(#28357,#28358),
(#28359,#28360),(#28361,#28362),(#28363,#28364),(#28365,#28366),(#28367,
#28368),(#28369,#28370),(#28371,#28372),(#28373,#28374),(#28375,#28376),
(#28377,#28378),(#28379,#28380),(#28381,#28382),(#28383,#28384),(#28385,
#28386),(#28387,#28388),(#28389,#28390),(#28391,#28392),(#28393,#28394),
(#28395,#28396),(#28397,#28398),(#28399,#28400),(#28401,#28402),(#28403,
#28404),(#28405,#28406),(#28407,#28408),(#28409,#28410)),.UNSPECIFIED.,
 .F.,.F.,.F.)
B_SPLINE_SURFACE_WITH_KNOTS((6,1,1,1,1,1,1,1,1,1,1,1,1,1,1,1,1,1,1,1,1,
1,1,1,1,1,1,1,1,1,1,1,1,1,1,1,1,1,1,1,1,1,1,1,1,1,1,1,1,1,1,1,1,1,1,1,1,
1,1,1,1,1,1,1,1,6),(2,2),(-1.,-0.984615384615383,-0.969230769230768,-0.953846153846152,
-0.938461538461537,-0.923076923076922,-0.907692307692306,-0.892307692307691,
-0.876923076923076,-0.86153846153846,-0.846153846153845,-0.83076923076923,
-0.815384615384614,-0.799999999999999,-0.784615384615384,-0.769230769230768,
-0.753846153846153,-0.738461538461538,-0.723076923076922,-0.707692307692307,
-0.692307692307692,-0.676923076923076,-0.661538461538461,-0.646153846153846,
-0.63076923076923,-0.615384615384615,-0.6,-0.584615384615384,-0.569230769230769,
-0.553846153846154,-0.538461538461538,-0.523076923076923,-0.507692307692308,
-0.492307692307692,-0.476923076923077,-0.461538461538462,-0.446153846153846,
-0.430769230769231,-0.415384615384615,-0.4,-0.384615384615385,-0.369230769230769,
-0.353846153846154,-0.338461538461538,-0.323076923076923,-0.307692307692308,
-0.292307692307692,-0.276923076923077,-0.261538461538462,-0.246153846153846,
-0.230769230769231,-0.215384615384615,-0.2,-0.184615384615385,-0.169230769230769,
-0.153846153846154,-0.138461538461538,-0.123076923076923,-0.107692307692308,
-0.0923076923076923,-0.0769230769230769,-0.0615384615384615,-0.0461538461538462,
-0.0307692307692308,-0.0153846153846154,0.),(-1.,1.),.UNSPECIFIED.)
GEOMETRIC_REPRESENTATION_ITEM()
RATIONAL_B_SPLINE_SURFACE(((1.,1.),(1.,1.),(1.,1.),(1.,1.),(1.,1.),(1.,
1.),(1.,1.),(1.,1.),(1.,1.),(1.,1.),(1.,1.),(1.,1.),(1.,1.),(1.,1.),(1.,
1.),(1.,1.),(1.,1.),(1.,1.),(1.,1.),(1.,1.),(1.,1.),(1.,1.),(1.,1.),(1.,
1.),(1.,1.),(1.,1.),(1.,1.),(1.,1.),(1.,1.),(1.,1.),(1.,1.),(1.,1.),(1.,
1.),(1.,1.),(1.,1.),(1.,1.),(1.,1.),(1.,1.),(1.,1.),(1.,1.),(1.,1.),(1.,
1.),(1.,1.),(1.,1.),(1.,1.),(1.,1.),(1.,1.),(1.,1.),(1.,1.),(1.,1.),(1.,
1.),(1.,1.),(1.,1.),(1.,1.),(1.,1.),(1.,1.),(1.,1.),(1.,1.),(1.,1.),(1.,
1.),(1.,1.),(1.,1.),(1.,1.),(1.,1.),(1.,1.),(1.,1.),(1.,1.),(1.,1.),(1.,
1.),(1.,1.)))
REPRESENTATION_ITEM('')
SURFACE()
);
#45=(
BOUNDED_SURFACE()
B_SPLINE_SURFACE(5,1,((#28487,#28488),(#28489,#28490),(#28491,#28492),(#28493,
#28494),(#28495,#28496),(#28497,#28498),(#28499,#28500),(#28501,#28502),
(#28503,#28504),(#28505,#28506),(#28507,#28508),(#28509,#28510),(#28511,
#28512),(#28513,#28514),(#28515,#28516),(#28517,#28518),(#28519,#28520),
(#28521,#28522),(#28523,#28524),(#28525,#28526),(#28527,#28528),(#28529,
#28530),(#28531,#28532),(#28533,#28534),(#28535,#28536),(#28537,#28538),
(#28539,#28540),(#28541,#28542),(#28543,#28544),(#28545,#28546),(#28547,
#28548),(#28549,#28550),(#28551,#28552),(#28553,#28554),(#28555,#28556),
(#28557,#28558),(#28559,#28560),(#28561,#28562),(#28563,#28564),(#28565,
#28566),(#28567,#28568),(#28569,#28570),(#28571,#28572),(#28573,#28574),
(#28575,#28576),(#28577,#28578),(#28579,#28580),(#28581,#28582),(#28583,
#28584),(#28585,#28586),(#28587,#28588),(#28589,#28590),(#28591,#28592),
(#28593,#28594),(#28595,#28596),(#28597,#28598),(#28599,#28600),(#28601,
#28602),(#28603,#28604),(#28605,#28606),(#28607,#28608),(#28609,#28610),
(#28611,#28612),(#28613,#28614),(#28615,#28616),(#28617,#28618),(#28619,
#28620),(#28621,#28622),(#28623,#28624),(#28625,#28626)),.UNSPECIFIED.,
 .F.,.F.,.F.)
B_SPLINE_SURFACE_WITH_KNOTS((6,1,1,1,1,1,1,1,1,1,1,1,1,1,1,1,1,1,1,1,1,
1,1,1,1,1,1,1,1,1,1,1,1,1,1,1,1,1,1,1,1,1,1,1,1,1,1,1,1,1,1,1,1,1,1,1,1,
1,1,1,1,1,1,1,1,6),(2,2),(-1.,-0.984615384615383,-0.969230769230768,-0.953846153846152,
-0.938461538461537,-0.923076923076922,-0.907692307692306,-0.892307692307691,
-0.876923076923076,-0.86153846153846,-0.846153846153845,-0.83076923076923,
-0.815384615384614,-0.799999999999999,-0.784615384615384,-0.769230769230768,
-0.753846153846153,-0.738461538461538,-0.723076923076922,-0.707692307692307,
-0.692307692307692,-0.676923076923076,-0.661538461538461,-0.646153846153846,
-0.63076923076923,-0.615384615384615,-0.6,-0.584615384615384,-0.569230769230769,
-0.553846153846154,-0.538461538461538,-0.523076923076923,-0.507692307692308,
-0.492307692307692,-0.476923076923077,-0.461538461538462,-0.446153846153846,
-0.430769230769231,-0.415384615384615,-0.4,-0.384615384615385,-0.369230769230769,
-0.353846153846154,-0.338461538461538,-0.323076923076923,-0.307692307692308,
-0.292307692307692,-0.276923076923077,-0.261538461538462,-0.246153846153846,
-0.230769230769231,-0.215384615384615,-0.2,-0.184615384615385,-0.169230769230769,
-0.153846153846154,-0.138461538461538,-0.123076923076923,-0.107692307692308,
-0.0923076923076923,-0.0769230769230769,-0.0615384615384615,-0.0461538461538462,
-0.0307692307692308,-0.0153846153846154,0.),(-1.,1.),.UNSPECIFIED.)
GEOMETRIC_REPRESENTATION_ITEM()
RATIONAL_B_SPLINE_SURFACE(((1.,1.),(1.,1.),(1.,1.),(1.,1.),(1.,1.),(1.,
1.),(1.,1.),(1.,1.),(1.,1.),(1.,1.),(1.,1.),(1.,1.),(1.,1.),(1.,1.),(1.,
1.),(1.,1.),(1.,1.),(1.,1.),(1.,1.),(1.,1.),(1.,1.),(1.,1.),(1.,1.),(1.,
1.),(1.,1.),(1.,1.),(1.,1.),(1.,1.),(1.,1.),(1.,1.),(1.,1.),(1.,1.),(1.,
1.),(1.,1.),(1.,1.),(1.,1.),(1.,1.),(1.,1.),(1.,1.),(1.,1.),(1.,1.),(1.,
1.),(1.,1.),(1.,1.),(1.,1.),(1.,1.),(1.,1.),(1.,1.),(1.,1.),(1.,1.),(1.,
1.),(1.,1.),(1.,1.),(1.,1.),(1.,1.),(1.,1.),(1.,1.),(1.,1.),(1.,1.),(1.,
1.),(1.,1.),(1.,1.),(1.,1.),(1.,1.),(1.,1.),(1.,1.),(1.,1.),(1.,1.),(1.,
1.),(1.,1.)))
REPRESENTATION_ITEM('')
SURFACE()
);
#46=(
BOUNDED_SURFACE()
B_SPLINE_SURFACE(5,1,((#28703,#28704),(#28705,#28706),(#28707,#28708),(#28709,
#28710),(#28711,#28712),(#28713,#28714),(#28715,#28716),(#28717,#28718),
(#28719,#28720),(#28721,#28722),(#28723,#28724),(#28725,#28726),(#28727,
#28728),(#28729,#28730),(#28731,#28732),(#28733,#28734),(#28735,#28736),
(#28737,#28738),(#28739,#28740),(#28741,#28742),(#28743,#28744),(#28745,
#28746),(#28747,#28748),(#28749,#28750),(#28751,#28752),(#28753,#28754),
(#28755,#28756),(#28757,#28758),(#28759,#28760),(#28761,#28762),(#28763,
#28764),(#28765,#28766),(#28767,#28768),(#28769,#28770),(#28771,#28772),
(#28773,#28774),(#28775,#28776),(#28777,#28778),(#28779,#28780),(#28781,
#28782),(#28783,#28784),(#28785,#28786),(#28787,#28788),(#28789,#28790),
(#28791,#28792),(#28793,#28794),(#28795,#28796),(#28797,#28798),(#28799,
#28800),(#28801,#28802),(#28803,#28804),(#28805,#28806),(#28807,#28808),
(#28809,#28810),(#28811,#28812),(#28813,#28814),(#28815,#28816),(#28817,
#28818),(#28819,#28820),(#28821,#28822),(#28823,#28824),(#28825,#28826),
(#28827,#28828),(#28829,#28830),(#28831,#28832),(#28833,#28834),(#28835,
#28836),(#28837,#28838),(#28839,#28840),(#28841,#28842)),.UNSPECIFIED.,
 .F.,.F.,.F.)
B_SPLINE_SURFACE_WITH_KNOTS((6,1,1,1,1,1,1,1,1,1,1,1,1,1,1,1,1,1,1,1,1,
1,1,1,1,1,1,1,1,1,1,1,1,1,1,1,1,1,1,1,1,1,1,1,1,1,1,1,1,1,1,1,1,1,1,1,1,
1,1,1,1,1,1,1,1,6),(2,2),(-1.,-0.984615384615383,-0.969230769230768,-0.953846153846152,
-0.938461538461537,-0.923076923076922,-0.907692307692306,-0.892307692307691,
-0.876923076923076,-0.86153846153846,-0.846153846153845,-0.83076923076923,
-0.815384615384614,-0.799999999999999,-0.784615384615384,-0.769230769230768,
-0.753846153846153,-0.738461538461538,-0.723076923076922,-0.707692307692307,
-0.692307692307692,-0.676923076923076,-0.661538461538461,-0.646153846153846,
-0.63076923076923,-0.615384615384615,-0.6,-0.584615384615384,-0.569230769230769,
-0.553846153846154,-0.538461538461538,-0.523076923076923,-0.507692307692308,
-0.492307692307692,-0.476923076923077,-0.461538461538462,-0.446153846153846,
-0.430769230769231,-0.415384615384615,-0.4,-0.384615384615385,-0.369230769230769,
-0.353846153846154,-0.338461538461538,-0.323076923076923,-0.307692307692308,
-0.292307692307692,-0.276923076923077,-0.261538461538462,-0.246153846153846,
-0.230769230769231,-0.215384615384615,-0.2,-0.184615384615385,-0.169230769230769,
-0.153846153846154,-0.138461538461538,-0.123076923076923,-0.107692307692308,
-0.0923076923076923,-0.0769230769230769,-0.0615384615384615,-0.0461538461538462,
-0.0307692307692308,-0.0153846153846154,0.),(-1.,1.),.UNSPECIFIED.)
GEOMETRIC_REPRESENTATION_ITEM()
RATIONAL_B_SPLINE_SURFACE(((1.,1.),(1.,1.),(1.,1.),(1.,1.),(1.,1.),(1.,
1.),(1.,1.),(1.,1.),(1.,1.),(1.,1.),(1.,1.),(1.,1.),(1.,1.),(1.,1.),(1.,
1.),(1.,1.),(1.,1.),(1.,1.),(1.,1.),(1.,1.),(1.,1.),(1.,1.),(1.,1.),(1.,
1.),(1.,1.),(1.,1.),(1.,1.),(1.,1.),(1.,1.),(1.,1.),(1.,1.),(1.,1.),(1.,
1.),(1.,1.),(1.,1.),(1.,1.),(1.,1.),(1.,1.),(1.,1.),(1.,1.),(1.,1.),(1.,
1.),(1.,1.),(1.,1.),(1.,1.),(1.,1.),(1.,1.),(1.,1.),(1.,1.),(1.,1.),(1.,
1.),(1.,1.),(1.,1.),(1.,1.),(1.,1.),(1.,1.),(1.,1.),(1.,1.),(1.,1.),(1.,
1.),(1.,1.),(1.,1.),(1.,1.),(1.,1.),(1.,1.),(1.,1.),(1.,1.),(1.,1.),(1.,
1.),(1.,1.)))
REPRESENTATION_ITEM('')
SURFACE()
);
#47=(
BOUNDED_SURFACE()
B_SPLINE_SURFACE(5,1,((#28919,#28920),(#28921,#28922),(#28923,#28924),(#28925,
#28926),(#28927,#28928),(#28929,#28930),(#28931,#28932),(#28933,#28934),
(#28935,#28936),(#28937,#28938),(#28939,#28940),(#28941,#28942),(#28943,
#28944),(#28945,#28946),(#28947,#28948),(#28949,#28950),(#28951,#28952),
(#28953,#28954),(#28955,#28956),(#28957,#28958),(#28959,#28960),(#28961,
#28962),(#28963,#28964),(#28965,#28966),(#28967,#28968),(#28969,#28970),
(#28971,#28972),(#28973,#28974),(#28975,#28976),(#28977,#28978),(#28979,
#28980),(#28981,#28982),(#28983,#28984),(#28985,#28986),(#28987,#28988),
(#28989,#28990),(#28991,#28992),(#28993,#28994),(#28995,#28996),(#28997,
#28998),(#28999,#29000),(#29001,#29002),(#29003,#29004),(#29005,#29006),
(#29007,#29008),(#29009,#29010),(#29011,#29012),(#29013,#29014),(#29015,
#29016),(#29017,#29018),(#29019,#29020),(#29021,#29022),(#29023,#29024),
(#29025,#29026),(#29027,#29028),(#29029,#29030),(#29031,#29032),(#29033,
#29034),(#29035,#29036),(#29037,#29038),(#29039,#29040),(#29041,#29042),
(#29043,#29044),(#29045,#29046),(#29047,#29048),(#29049,#29050),(#29051,
#29052),(#29053,#29054),(#29055,#29056),(#29057,#29058)),.UNSPECIFIED.,
 .F.,.F.,.F.)
B_SPLINE_SURFACE_WITH_KNOTS((6,1,1,1,1,1,1,1,1,1,1,1,1,1,1,1,1,1,1,1,1,
1,1,1,1,1,1,1,1,1,1,1,1,1,1,1,1,1,1,1,1,1,1,1,1,1,1,1,1,1,1,1,1,1,1,1,1,
1,1,1,1,1,1,1,1,6),(2,2),(-1.,-0.984615384615383,-0.969230769230768,-0.953846153846152,
-0.938461538461537,-0.923076923076922,-0.907692307692306,-0.892307692307691,
-0.876923076923076,-0.86153846153846,-0.846153846153845,-0.83076923076923,
-0.815384615384614,-0.799999999999999,-0.784615384615384,-0.769230769230768,
-0.753846153846153,-0.738461538461538,-0.723076923076922,-0.707692307692307,
-0.692307692307692,-0.676923076923076,-0.661538461538461,-0.646153846153846,
-0.63076923076923,-0.615384615384615,-0.6,-0.584615384615384,-0.569230769230769,
-0.553846153846154,-0.538461538461538,-0.523076923076923,-0.507692307692308,
-0.492307692307692,-0.476923076923077,-0.461538461538462,-0.446153846153846,
-0.430769230769231,-0.415384615384615,-0.4,-0.384615384615385,-0.369230769230769,
-0.353846153846154,-0.338461538461538,-0.323076923076923,-0.307692307692308,
-0.292307692307692,-0.276923076923077,-0.261538461538462,-0.246153846153846,
-0.230769230769231,-0.215384615384615,-0.2,-0.184615384615385,-0.169230769230769,
-0.153846153846154,-0.138461538461538,-0.123076923076923,-0.107692307692308,
-0.0923076923076923,-0.0769230769230769,-0.0615384615384615,-0.0461538461538462,
-0.0307692307692308,-0.0153846153846154,0.),(-1.,1.),.UNSPECIFIED.)
GEOMETRIC_REPRESENTATION_ITEM()
RATIONAL_B_SPLINE_SURFACE(((1.,1.),(1.,1.),(1.,1.),(1.,1.),(1.,1.),(1.,
1.),(1.,1.),(1.,1.),(1.,1.),(1.,1.),(1.,1.),(1.,1.),(1.,1.),(1.,1.),(1.,
1.),(1.,1.),(1.,1.),(1.,1.),(1.,1.),(1.,1.),(1.,1.),(1.,1.),(1.,1.),(1.,
1.),(1.,1.),(1.,1.),(1.,1.),(1.,1.),(1.,1.),(1.,1.),(1.,1.),(1.,1.),(1.,
1.),(1.,1.),(1.,1.),(1.,1.),(1.,1.),(1.,1.),(1.,1.),(1.,1.),(1.,1.),(1.,
1.),(1.,1.),(1.,1.),(1.,1.),(1.,1.),(1.,1.),(1.,1.),(1.,1.),(1.,1.),(1.,
1.),(1.,1.),(1.,1.),(1.,1.),(1.,1.),(1.,1.),(1.,1.),(1.,1.),(1.,1.),(1.,
1.),(1.,1.),(1.,1.),(1.,1.),(1.,1.),(1.,1.),(1.,1.),(1.,1.),(1.,1.),(1.,
1.),(1.,1.)))
REPRESENTATION_ITEM('')
SURFACE()
);
#48=(
BOUNDED_SURFACE()
B_SPLINE_SURFACE(5,1,((#29135,#29136),(#29137,#29138),(#29139,#29140),(#29141,
#29142),(#29143,#29144),(#29145,#29146),(#29147,#29148),(#29149,#29150),
(#29151,#29152),(#29153,#29154),(#29155,#29156),(#29157,#29158),(#29159,
#29160),(#29161,#29162),(#29163,#29164),(#29165,#29166),(#29167,#29168),
(#29169,#29170),(#29171,#29172),(#29173,#29174),(#29175,#29176),(#29177,
#29178),(#29179,#29180),(#29181,#29182),(#29183,#29184),(#29185,#29186),
(#29187,#29188),(#29189,#29190),(#29191,#29192),(#29193,#29194),(#29195,
#29196),(#29197,#29198),(#29199,#29200),(#29201,#29202),(#29203,#29204),
(#29205,#29206),(#29207,#29208),(#29209,#29210),(#29211,#29212),(#29213,
#29214),(#29215,#29216),(#29217,#29218),(#29219,#29220),(#29221,#29222),
(#29223,#29224),(#29225,#29226),(#29227,#29228),(#29229,#29230),(#29231,
#29232),(#29233,#29234),(#29235,#29236),(#29237,#29238),(#29239,#29240),
(#29241,#29242),(#29243,#29244),(#29245,#29246),(#29247,#29248),(#29249,
#29250),(#29251,#29252),(#29253,#29254),(#29255,#29256),(#29257,#29258),
(#29259,#29260),(#29261,#29262),(#29263,#29264),(#29265,#29266),(#29267,
#29268),(#29269,#29270),(#29271,#29272),(#29273,#29274)),.UNSPECIFIED.,
 .F.,.F.,.F.)
B_SPLINE_SURFACE_WITH_KNOTS((6,1,1,1,1,1,1,1,1,1,1,1,1,1,1,1,1,1,1,1,1,
1,1,1,1,1,1,1,1,1,1,1,1,1,1,1,1,1,1,1,1,1,1,1,1,1,1,1,1,1,1,1,1,1,1,1,1,
1,1,1,1,1,1,1,1,6),(2,2),(-1.,-0.984615384615383,-0.969230769230768,-0.953846153846152,
-0.938461538461537,-0.923076923076922,-0.907692307692306,-0.892307692307691,
-0.876923076923076,-0.86153846153846,-0.846153846153845,-0.83076923076923,
-0.815384615384614,-0.799999999999999,-0.784615384615384,-0.769230769230768,
-0.753846153846153,-0.738461538461538,-0.723076923076922,-0.707692307692307,
-0.692307692307692,-0.676923076923076,-0.661538461538461,-0.646153846153846,
-0.63076923076923,-0.615384615384615,-0.6,-0.584615384615384,-0.569230769230769,
-0.553846153846154,-0.538461538461538,-0.523076923076923,-0.507692307692308,
-0.492307692307692,-0.476923076923077,-0.461538461538462,-0.446153846153846,
-0.430769230769231,-0.415384615384615,-0.4,-0.384615384615385,-0.369230769230769,
-0.353846153846154,-0.338461538461538,-0.323076923076923,-0.307692307692308,
-0.292307692307692,-0.276923076923077,-0.261538461538462,-0.246153846153846,
-0.230769230769231,-0.215384615384615,-0.2,-0.184615384615385,-0.169230769230769,
-0.153846153846154,-0.138461538461538,-0.123076923076923,-0.107692307692308,
-0.0923076923076923,-0.0769230769230769,-0.0615384615384615,-0.0461538461538462,
-0.0307692307692308,-0.0153846153846154,0.),(-1.,1.),.UNSPECIFIED.)
GEOMETRIC_REPRESENTATION_ITEM()
RATIONAL_B_SPLINE_SURFACE(((1.,1.),(1.,1.),(1.,1.),(1.,1.),(1.,1.),(1.,
1.),(1.,1.),(1.,1.),(1.,1.),(1.,1.),(1.,1.),(1.,1.),(1.,1.),(1.,1.),(1.,
1.),(1.,1.),(1.,1.),(1.,1.),(1.,1.),(1.,1.),(1.,1.),(1.,1.),(1.,1.),(1.,
1.),(1.,1.),(1.,1.),(1.,1.),(1.,1.),(1.,1.),(1.,1.),(1.,1.),(1.,1.),(1.,
1.),(1.,1.),(1.,1.),(1.,1.),(1.,1.),(1.,1.),(1.,1.),(1.,1.),(1.,1.),(1.,
1.),(1.,1.),(1.,1.),(1.,1.),(1.,1.),(1.,1.),(1.,1.),(1.,1.),(1.,1.),(1.,
1.),(1.,1.),(1.,1.),(1.,1.),(1.,1.),(1.,1.),(1.,1.),(1.,1.),(1.,1.),(1.,
1.),(1.,1.),(1.,1.),(1.,1.),(1.,1.),(1.,1.),(1.,1.),(1.,1.),(1.,1.),(1.,
1.),(1.,1.)))
REPRESENTATION_ITEM('')
SURFACE()
);
#49=(
BOUNDED_SURFACE()
B_SPLINE_SURFACE(5,1,((#29351,#29352),(#29353,#29354),(#29355,#29356),(#29357,
#29358),(#29359,#29360),(#29361,#29362),(#29363,#29364),(#29365,#29366),
(#29367,#29368),(#29369,#29370),(#29371,#29372),(#29373,#29374),(#29375,
#29376),(#29377,#29378),(#29379,#29380),(#29381,#29382),(#29383,#29384),
(#29385,#29386),(#29387,#29388),(#29389,#29390),(#29391,#29392),(#29393,
#29394),(#29395,#29396),(#29397,#29398),(#29399,#29400),(#29401,#29402),
(#29403,#29404),(#29405,#29406),(#29407,#29408),(#29409,#29410),(#29411,
#29412),(#29413,#29414),(#29415,#29416),(#29417,#29418),(#29419,#29420),
(#29421,#29422),(#29423,#29424),(#29425,#29426),(#29427,#29428),(#29429,
#29430),(#29431,#29432),(#29433,#29434),(#29435,#29436),(#29437,#29438),
(#29439,#29440),(#29441,#29442),(#29443,#29444),(#29445,#29446),(#29447,
#29448),(#29449,#29450),(#29451,#29452),(#29453,#29454),(#29455,#29456),
(#29457,#29458),(#29459,#29460),(#29461,#29462),(#29463,#29464),(#29465,
#29466),(#29467,#29468),(#29469,#29470),(#29471,#29472),(#29473,#29474),
(#29475,#29476),(#29477,#29478),(#29479,#29480),(#29481,#29482),(#29483,
#29484),(#29485,#29486),(#29487,#29488),(#29489,#29490)),.UNSPECIFIED.,
 .F.,.F.,.F.)
B_SPLINE_SURFACE_WITH_KNOTS((6,1,1,1,1,1,1,1,1,1,1,1,1,1,1,1,1,1,1,1,1,
1,1,1,1,1,1,1,1,1,1,1,1,1,1,1,1,1,1,1,1,1,1,1,1,1,1,1,1,1,1,1,1,1,1,1,1,
1,1,1,1,1,1,1,1,6),(2,2),(-1.,-0.984615384615383,-0.969230769230768,-0.953846153846152,
-0.938461538461537,-0.923076923076922,-0.907692307692306,-0.892307692307691,
-0.876923076923076,-0.86153846153846,-0.846153846153845,-0.83076923076923,
-0.815384615384614,-0.799999999999999,-0.784615384615384,-0.769230769230768,
-0.753846153846153,-0.738461538461538,-0.723076923076922,-0.707692307692307,
-0.692307692307692,-0.676923076923076,-0.661538461538461,-0.646153846153846,
-0.63076923076923,-0.615384615384615,-0.6,-0.584615384615384,-0.569230769230769,
-0.553846153846154,-0.538461538461538,-0.523076923076923,-0.507692307692308,
-0.492307692307692,-0.476923076923077,-0.461538461538462,-0.446153846153846,
-0.430769230769231,-0.415384615384615,-0.4,-0.384615384615385,-0.369230769230769,
-0.353846153846154,-0.338461538461538,-0.323076923076923,-0.307692307692308,
-0.292307692307692,-0.276923076923077,-0.261538461538462,-0.246153846153846,
-0.230769230769231,-0.215384615384615,-0.2,-0.184615384615385,-0.169230769230769,
-0.153846153846154,-0.138461538461538,-0.123076923076923,-0.107692307692308,
-0.0923076923076923,-0.0769230769230769,-0.0615384615384615,-0.0461538461538462,
-0.0307692307692308,-0.0153846153846154,0.),(-1.,1.),.UNSPECIFIED.)
GEOMETRIC_REPRESENTATION_ITEM()
RATIONAL_B_SPLINE_SURFACE(((1.,1.),(1.,1.),(1.,1.),(1.,1.),(1.,1.),(1.,
1.),(1.,1.),(1.,1.),(1.,1.),(1.,1.),(1.,1.),(1.,1.),(1.,1.),(1.,1.),(1.,
1.),(1.,1.),(1.,1.),(1.,1.),(1.,1.),(1.,1.),(1.,1.),(1.,1.),(1.,1.),(1.,
1.),(1.,1.),(1.,1.),(1.,1.),(1.,1.),(1.,1.),(1.,1.),(1.,1.),(1.,1.),(1.,
1.),(1.,1.),(1.,1.),(1.,1.),(1.,1.),(1.,1.),(1.,1.),(1.,1.),(1.,1.),(1.,
1.),(1.,1.),(1.,1.),(1.,1.),(1.,1.),(1.,1.),(1.,1.),(1.,1.),(1.,1.),(1.,
1.),(1.,1.),(1.,1.),(1.,1.),(1.,1.),(1.,1.),(1.,1.),(1.,1.),(1.,1.),(1.,
1.),(1.,1.),(1.,1.),(1.,1.),(1.,1.),(1.,1.),(1.,1.),(1.,1.),(1.,1.),(1.,
1.),(1.,1.)))
REPRESENTATION_ITEM('')
SURFACE()
);
#50=(
BOUNDED_SURFACE()
B_SPLINE_SURFACE(5,1,((#29567,#29568),(#29569,#29570),(#29571,#29572),(#29573,
#29574),(#29575,#29576),(#29577,#29578),(#29579,#29580),(#29581,#29582),
(#29583,#29584),(#29585,#29586),(#29587,#29588),(#29589,#29590),(#29591,
#29592),(#29593,#29594),(#29595,#29596),(#29597,#29598),(#29599,#29600),
(#29601,#29602),(#29603,#29604),(#29605,#29606),(#29607,#29608),(#29609,
#29610),(#29611,#29612),(#29613,#29614),(#29615,#29616),(#29617,#29618),
(#29619,#29620),(#29621,#29622),(#29623,#29624),(#29625,#29626),(#29627,
#29628),(#29629,#29630),(#29631,#29632),(#29633,#29634),(#29635,#29636),
(#29637,#29638),(#29639,#29640),(#29641,#29642),(#29643,#29644),(#29645,
#29646),(#29647,#29648),(#29649,#29650),(#29651,#29652),(#29653,#29654),
(#29655,#29656),(#29657,#29658),(#29659,#29660),(#29661,#29662),(#29663,
#29664),(#29665,#29666),(#29667,#29668),(#29669,#29670),(#29671,#29672),
(#29673,#29674),(#29675,#29676),(#29677,#29678),(#29679,#29680),(#29681,
#29682),(#29683,#29684),(#29685,#29686),(#29687,#29688),(#29689,#29690),
(#29691,#29692),(#29693,#29694),(#29695,#29696),(#29697,#29698),(#29699,
#29700),(#29701,#29702),(#29703,#29704),(#29705,#29706)),.UNSPECIFIED.,
 .F.,.F.,.F.)
B_SPLINE_SURFACE_WITH_KNOTS((6,1,1,1,1,1,1,1,1,1,1,1,1,1,1,1,1,1,1,1,1,
1,1,1,1,1,1,1,1,1,1,1,1,1,1,1,1,1,1,1,1,1,1,1,1,1,1,1,1,1,1,1,1,1,1,1,1,
1,1,1,1,1,1,1,1,6),(2,2),(-1.,-0.984615384615383,-0.969230769230768,-0.953846153846152,
-0.938461538461537,-0.923076923076922,-0.907692307692306,-0.892307692307691,
-0.876923076923076,-0.86153846153846,-0.846153846153845,-0.83076923076923,
-0.815384615384614,-0.799999999999999,-0.784615384615384,-0.769230769230768,
-0.753846153846153,-0.738461538461538,-0.723076923076922,-0.707692307692307,
-0.692307692307692,-0.676923076923076,-0.661538461538461,-0.646153846153846,
-0.63076923076923,-0.615384615384615,-0.6,-0.584615384615384,-0.569230769230769,
-0.553846153846154,-0.538461538461538,-0.523076923076923,-0.507692307692308,
-0.492307692307692,-0.476923076923077,-0.461538461538462,-0.446153846153846,
-0.430769230769231,-0.415384615384615,-0.4,-0.384615384615385,-0.369230769230769,
-0.353846153846154,-0.338461538461538,-0.323076923076923,-0.307692307692308,
-0.292307692307692,-0.276923076923077,-0.261538461538462,-0.246153846153846,
-0.230769230769231,-0.215384615384615,-0.2,-0.184615384615385,-0.169230769230769,
-0.153846153846154,-0.138461538461538,-0.123076923076923,-0.107692307692308,
-0.0923076923076923,-0.0769230769230769,-0.0615384615384615,-0.0461538461538462,
-0.0307692307692308,-0.0153846153846154,0.),(-1.,1.),.UNSPECIFIED.)
GEOMETRIC_REPRESENTATION_ITEM()
RATIONAL_B_SPLINE_SURFACE(((1.,1.),(1.,1.),(1.,1.),(1.,1.),(1.,1.),(1.,
1.),(1.,1.),(1.,1.),(1.,1.),(1.,1.),(1.,1.),(1.,1.),(1.,1.),(1.,1.),(1.,
1.),(1.,1.),(1.,1.),(1.,1.),(1.,1.),(1.,1.),(1.,1.),(1.,1.),(1.,1.),(1.,
1.),(1.,1.),(1.,1.),(1.,1.),(1.,1.),(1.,1.),(1.,1.),(1.,1.),(1.,1.),(1.,
1.),(1.,1.),(1.,1.),(1.,1.),(1.,1.),(1.,1.),(1.,1.),(1.,1.),(1.,1.),(1.,
1.),(1.,1.),(1.,1.),(1.,1.),(1.,1.),(1.,1.),(1.,1.),(1.,1.),(1.,1.),(1.,
1.),(1.,1.),(1.,1.),(1.,1.),(1.,1.),(1.,1.),(1.,1.),(1.,1.),(1.,1.),(1.,
1.),(1.,1.),(1.,1.),(1.,1.),(1.,1.),(1.,1.),(1.,1.),(1.,1.),(1.,1.),(1.,
1.),(1.,1.)))
REPRESENTATION_ITEM('')
SURFACE()
);
#51=(
BOUNDED_SURFACE()
B_SPLINE_SURFACE(5,1,((#35999,#36000),(#36001,#36002),(#36003,#36004),(#36005,
#36006),(#36007,#36008),(#36009,#36010),(#36011,#36012),(#36013,#36014),
(#36015,#36016),(#36017,#36018),(#36019,#36020),(#36021,#36022),(#36023,
#36024),(#36025,#36026),(#36027,#36028),(#36029,#36030),(#36031,#36032),
(#36033,#36034),(#36035,#36036),(#36037,#36038),(#36039,#36040),(#36041,
#36042),(#36043,#36044),(#36045,#36046),(#36047,#36048),(#36049,#36050),
(#36051,#36052),(#36053,#36054),(#36055,#36056),(#36057,#36058),(#36059,
#36060),(#36061,#36062),(#36063,#36064),(#36065,#36066),(#36067,#36068),
(#36069,#36070),(#36071,#36072),(#36073,#36074),(#36075,#36076),(#36077,
#36078),(#36079,#36080),(#36081,#36082),(#36083,#36084),(#36085,#36086),
(#36087,#36088),(#36089,#36090),(#36091,#36092),(#36093,#36094),(#36095,
#36096),(#36097,#36098),(#36099,#36100),(#36101,#36102),(#36103,#36104),
(#36105,#36106),(#36107,#36108),(#36109,#36110),(#36111,#36112),(#36113,
#36114),(#36115,#36116),(#36117,#36118),(#36119,#36120),(#36121,#36122),
(#36123,#36124),(#36125,#36126),(#36127,#36128),(#36129,#36130),(#36131,
#36132),(#36133,#36134),(#36135,#36136),(#36137,#36138)),.UNSPECIFIED.,
 .F.,.F.,.F.)
B_SPLINE_SURFACE_WITH_KNOTS((6,1,1,1,1,1,1,1,1,1,1,1,1,1,1,1,1,1,1,1,1,
1,1,1,1,1,1,1,1,1,1,1,1,1,1,1,1,1,1,1,1,1,1,1,1,1,1,1,1,1,1,1,1,1,1,1,1,
1,1,1,1,1,1,1,1,6),(2,2),(-1.,-0.984615384615383,-0.969230769230768,-0.953846153846152,
-0.938461538461537,-0.923076923076922,-0.907692307692306,-0.892307692307691,
-0.876923076923076,-0.86153846153846,-0.846153846153845,-0.83076923076923,
-0.815384615384614,-0.799999999999999,-0.784615384615384,-0.769230769230768,
-0.753846153846153,-0.738461538461538,-0.723076923076922,-0.707692307692307,
-0.692307692307692,-0.676923076923076,-0.661538461538461,-0.646153846153846,
-0.63076923076923,-0.615384615384615,-0.6,-0.584615384615384,-0.569230769230769,
-0.553846153846154,-0.538461538461538,-0.523076923076923,-0.507692307692308,
-0.492307692307692,-0.476923076923077,-0.461538461538462,-0.446153846153846,
-0.430769230769231,-0.415384615384615,-0.4,-0.384615384615385,-0.369230769230769,
-0.353846153846154,-0.338461538461538,-0.323076923076923,-0.307692307692308,
-0.292307692307692,-0.276923076923077,-0.261538461538462,-0.246153846153846,
-0.230769230769231,-0.215384615384615,-0.2,-0.184615384615385,-0.169230769230769,
-0.153846153846154,-0.138461538461538,-0.123076923076923,-0.107692307692308,
-0.0923076923076923,-0.0769230769230769,-0.0615384615384615,-0.0461538461538462,
-0.0307692307692308,-0.0153846153846154,0.),(-1.,1.),.UNSPECIFIED.)
GEOMETRIC_REPRESENTATION_ITEM()
RATIONAL_B_SPLINE_SURFACE(((1.,1.),(1.,1.),(1.,1.),(1.,1.),(1.,1.),(1.,
1.),(1.,1.),(1.,1.),(1.,1.),(1.,1.),(1.,1.),(1.,1.),(1.,1.),(1.,1.),(1.,
1.),(1.,1.),(1.,1.),(1.,1.),(1.,1.),(1.,1.),(1.,1.),(1.,1.),(1.,1.),(1.,
1.),(1.,1.),(1.,1.),(1.,1.),(1.,1.),(1.,1.),(1.,1.),(1.,1.),(1.,1.),(1.,
1.),(1.,1.),(1.,1.),(1.,1.),(1.,1.),(1.,1.),(1.,1.),(1.,1.),(1.,1.),(1.,
1.),(1.,1.),(1.,1.),(1.,1.),(1.,1.),(1.,1.),(1.,1.),(1.,1.),(1.,1.),(1.,
1.),(1.,1.),(1.,1.),(1.,1.),(1.,1.),(1.,1.),(1.,1.),(1.,1.),(1.,1.),(1.,
1.),(1.,1.),(1.,1.),(1.,1.),(1.,1.),(1.,1.),(1.,1.),(1.,1.),(1.,1.),(1.,
1.),(1.,1.)))
REPRESENTATION_ITEM('')
SURFACE()
);
#52=(
BOUNDED_SURFACE()
B_SPLINE_SURFACE(5,1,((#36218,#36219),(#36220,#36221),(#36222,#36223),(#36224,
#36225),(#36226,#36227),(#36228,#36229),(#36230,#36231),(#36232,#36233),
(#36234,#36235),(#36236,#36237),(#36238,#36239),(#36240,#36241),(#36242,
#36243),(#36244,#36245),(#36246,#36247),(#36248,#36249),(#36250,#36251),
(#36252,#36253),(#36254,#36255),(#36256,#36257),(#36258,#36259),(#36260,
#36261),(#36262,#36263),(#36264,#36265),(#36266,#36267),(#36268,#36269),
(#36270,#36271),(#36272,#36273),(#36274,#36275),(#36276,#36277),(#36278,
#36279),(#36280,#36281),(#36282,#36283),(#36284,#36285),(#36286,#36287),
(#36288,#36289),(#36290,#36291),(#36292,#36293),(#36294,#36295),(#36296,
#36297),(#36298,#36299),(#36300,#36301),(#36302,#36303),(#36304,#36305),
(#36306,#36307),(#36308,#36309),(#36310,#36311),(#36312,#36313),(#36314,
#36315),(#36316,#36317),(#36318,#36319),(#36320,#36321),(#36322,#36323),
(#36324,#36325),(#36326,#36327),(#36328,#36329),(#36330,#36331),(#36332,
#36333),(#36334,#36335),(#36336,#36337),(#36338,#36339),(#36340,#36341),
(#36342,#36343),(#36344,#36345),(#36346,#36347),(#36348,#36349),(#36350,
#36351),(#36352,#36353),(#36354,#36355),(#36356,#36357)),.UNSPECIFIED.,
 .F.,.F.,.F.)
B_SPLINE_SURFACE_WITH_KNOTS((6,1,1,1,1,1,1,1,1,1,1,1,1,1,1,1,1,1,1,1,1,
1,1,1,1,1,1,1,1,1,1,1,1,1,1,1,1,1,1,1,1,1,1,1,1,1,1,1,1,1,1,1,1,1,1,1,1,
1,1,1,1,1,1,1,1,6),(2,2),(-1.,-0.984615384615383,-0.969230769230768,-0.953846153846152,
-0.938461538461537,-0.923076923076922,-0.907692307692306,-0.892307692307691,
-0.876923076923076,-0.86153846153846,-0.846153846153845,-0.83076923076923,
-0.815384615384614,-0.799999999999999,-0.784615384615384,-0.769230769230768,
-0.753846153846153,-0.738461538461538,-0.723076923076922,-0.707692307692307,
-0.692307692307692,-0.676923076923076,-0.661538461538461,-0.646153846153846,
-0.63076923076923,-0.615384615384615,-0.6,-0.584615384615384,-0.569230769230769,
-0.553846153846154,-0.538461538461538,-0.523076923076923,-0.507692307692308,
-0.492307692307692,-0.476923076923077,-0.461538461538462,-0.446153846153846,
-0.430769230769231,-0.415384615384615,-0.4,-0.384615384615385,-0.369230769230769,
-0.353846153846154,-0.338461538461538,-0.323076923076923,-0.307692307692308,
-0.292307692307692,-0.276923076923077,-0.261538461538462,-0.246153846153846,
-0.230769230769231,-0.215384615384615,-0.2,-0.184615384615385,-0.169230769230769,
-0.153846153846154,-0.138461538461538,-0.123076923076923,-0.107692307692308,
-0.0923076923076923,-0.0769230769230769,-0.0615384615384615,-0.0461538461538462,
-0.0307692307692308,-0.0153846153846154,0.),(-1.,1.),.UNSPECIFIED.)
GEOMETRIC_REPRESENTATION_ITEM()
RATIONAL_B_SPLINE_SURFACE(((1.,1.),(1.,1.),(1.,1.),(1.,1.),(1.,1.),(1.,
1.),(1.,1.),(1.,1.),(1.,1.),(1.,1.),(1.,1.),(1.,1.),(1.,1.),(1.,1.),(1.,
1.),(1.,1.),(1.,1.),(1.,1.),(1.,1.),(1.,1.),(1.,1.),(1.,1.),(1.,1.),(1.,
1.),(1.,1.),(1.,1.),(1.,1.),(1.,1.),(1.,1.),(1.,1.),(1.,1.),(1.,1.),(1.,
1.),(1.,1.),(1.,1.),(1.,1.),(1.,1.),(1.,1.),(1.,1.),(1.,1.),(1.,1.),(1.,
1.),(1.,1.),(1.,1.),(1.,1.),(1.,1.),(1.,1.),(1.,1.),(1.,1.),(1.,1.),(1.,
1.),(1.,1.),(1.,1.),(1.,1.),(1.,1.),(1.,1.),(1.,1.),(1.,1.),(1.,1.),(1.,
1.),(1.,1.),(1.,1.),(1.,1.),(1.,1.),(1.,1.),(1.,1.),(1.,1.),(1.,1.),(1.,
1.),(1.,1.)))
REPRESENTATION_ITEM('')
SURFACE()
);
#53=(
BOUNDED_SURFACE()
B_SPLINE_SURFACE(5,1,((#36448,#36449),(#36450,#36451),(#36452,#36453),(#36454,
#36455),(#36456,#36457),(#36458,#36459),(#36460,#36461),(#36462,#36463),
(#36464,#36465),(#36466,#36467),(#36468,#36469),(#36470,#36471),(#36472,
#36473),(#36474,#36475),(#36476,#36477),(#36478,#36479),(#36480,#36481),
(#36482,#36483),(#36484,#36485),(#36486,#36487),(#36488,#36489),(#36490,
#36491),(#36492,#36493),(#36494,#36495),(#36496,#36497),(#36498,#36499),
(#36500,#36501),(#36502,#36503),(#36504,#36505),(#36506,#36507),(#36508,
#36509),(#36510,#36511),(#36512,#36513),(#36514,#36515),(#36516,#36517),
(#36518,#36519),(#36520,#36521),(#36522,#36523),(#36524,#36525),(#36526,
#36527),(#36528,#36529),(#36530,#36531),(#36532,#36533),(#36534,#36535),
(#36536,#36537),(#36538,#36539),(#36540,#36541),(#36542,#36543),(#36544,
#36545),(#36546,#36547),(#36548,#36549),(#36550,#36551),(#36552,#36553),
(#36554,#36555),(#36556,#36557),(#36558,#36559),(#36560,#36561),(#36562,
#36563),(#36564,#36565),(#36566,#36567),(#36568,#36569),(#36570,#36571),
(#36572,#36573),(#36574,#36575),(#36576,#36577),(#36578,#36579),(#36580,
#36581),(#36582,#36583),(#36584,#36585),(#36586,#36587)),.UNSPECIFIED.,
 .F.,.F.,.F.)
B_SPLINE_SURFACE_WITH_KNOTS((6,1,1,1,1,1,1,1,1,1,1,1,1,1,1,1,1,1,1,1,1,
1,1,1,1,1,1,1,1,1,1,1,1,1,1,1,1,1,1,1,1,1,1,1,1,1,1,1,1,1,1,1,1,1,1,1,1,
1,1,1,1,1,1,1,1,6),(2,2),(-1.,-0.984615384615383,-0.969230769230768,-0.953846153846152,
-0.938461538461537,-0.923076923076922,-0.907692307692306,-0.892307692307691,
-0.876923076923076,-0.86153846153846,-0.846153846153845,-0.83076923076923,
-0.815384615384614,-0.799999999999999,-0.784615384615384,-0.769230769230768,
-0.753846153846153,-0.738461538461538,-0.723076923076922,-0.707692307692307,
-0.692307692307692,-0.676923076923076,-0.661538461538461,-0.646153846153846,
-0.63076923076923,-0.615384615384615,-0.6,-0.584615384615384,-0.569230769230769,
-0.553846153846154,-0.538461538461538,-0.523076923076923,-0.507692307692308,
-0.492307692307692,-0.476923076923077,-0.461538461538462,-0.446153846153846,
-0.430769230769231,-0.415384615384615,-0.4,-0.384615384615385,-0.369230769230769,
-0.353846153846154,-0.338461538461538,-0.323076923076923,-0.307692307692308,
-0.292307692307692,-0.276923076923077,-0.261538461538462,-0.246153846153846,
-0.230769230769231,-0.215384615384615,-0.2,-0.184615384615385,-0.169230769230769,
-0.153846153846154,-0.138461538461538,-0.123076923076923,-0.107692307692308,
-0.0923076923076923,-0.0769230769230769,-0.0615384615384615,-0.0461538461538462,
-0.0307692307692308,-0.0153846153846154,0.),(-1.,1.),.UNSPECIFIED.)
GEOMETRIC_REPRESENTATION_ITEM()
RATIONAL_B_SPLINE_SURFACE(((1.,1.),(1.,1.),(1.,1.),(1.,1.),(1.,1.),(1.,
1.),(1.,1.),(1.,1.),(1.,1.),(1.,1.),(1.,1.),(1.,1.),(1.,1.),(1.,1.),(1.,
1.),(1.,1.),(1.,1.),(1.,1.),(1.,1.),(1.,1.),(1.,1.),(1.,1.),(1.,1.),(1.,
1.),(1.,1.),(1.,1.),(1.,1.),(1.,1.),(1.,1.),(1.,1.),(1.,1.),(1.,1.),(1.,
1.),(1.,1.),(1.,1.),(1.,1.),(1.,1.),(1.,1.),(1.,1.),(1.,1.),(1.,1.),(1.,
1.),(1.,1.),(1.,1.),(1.,1.),(1.,1.),(1.,1.),(1.,1.),(1.,1.),(1.,1.),(1.,
1.),(1.,1.),(1.,1.),(1.,1.),(1.,1.),(1.,1.),(1.,1.),(1.,1.),(1.,1.),(1.,
1.),(1.,1.),(1.,1.),(1.,1.),(1.,1.),(1.,1.),(1.,1.),(1.,1.),(1.,1.),(1.,
1.),(1.,1.)))
REPRESENTATION_ITEM('')
SURFACE()
);
#54=(
BOUNDED_SURFACE()
B_SPLINE_SURFACE(5,1,((#36660,#36661),(#36662,#36663),(#36664,#36665),(#36666,
#36667),(#36668,#36669),(#36670,#36671),(#36672,#36673),(#36674,#36675),
(#36676,#36677),(#36678,#36679),(#36680,#36681),(#36682,#36683),(#36684,
#36685),(#36686,#36687),(#36688,#36689),(#36690,#36691),(#36692,#36693),
(#36694,#36695),(#36696,#36697),(#36698,#36699),(#36700,#36701),(#36702,
#36703),(#36704,#36705),(#36706,#36707),(#36708,#36709),(#36710,#36711),
(#36712,#36713),(#36714,#36715),(#36716,#36717),(#36718,#36719),(#36720,
#36721),(#36722,#36723),(#36724,#36725),(#36726,#36727),(#36728,#36729),
(#36730,#36731),(#36732,#36733),(#36734,#36735),(#36736,#36737),(#36738,
#36739),(#36740,#36741),(#36742,#36743),(#36744,#36745),(#36746,#36747),
(#36748,#36749),(#36750,#36751),(#36752,#36753),(#36754,#36755),(#36756,
#36757),(#36758,#36759),(#36760,#36761),(#36762,#36763),(#36764,#36765),
(#36766,#36767),(#36768,#36769),(#36770,#36771),(#36772,#36773),(#36774,
#36775),(#36776,#36777),(#36778,#36779),(#36780,#36781),(#36782,#36783),
(#36784,#36785),(#36786,#36787),(#36788,#36789),(#36790,#36791),(#36792,
#36793),(#36794,#36795),(#36796,#36797),(#36798,#36799)),.UNSPECIFIED.,
 .F.,.F.,.F.)
B_SPLINE_SURFACE_WITH_KNOTS((6,1,1,1,1,1,1,1,1,1,1,1,1,1,1,1,1,1,1,1,1,
1,1,1,1,1,1,1,1,1,1,1,1,1,1,1,1,1,1,1,1,1,1,1,1,1,1,1,1,1,1,1,1,1,1,1,1,
1,1,1,1,1,1,1,1,6),(2,2),(-1.,-0.984615384615383,-0.969230769230768,-0.953846153846152,
-0.938461538461537,-0.923076923076922,-0.907692307692306,-0.892307692307691,
-0.876923076923076,-0.86153846153846,-0.846153846153845,-0.83076923076923,
-0.815384615384614,-0.799999999999999,-0.784615384615384,-0.769230769230768,
-0.753846153846153,-0.738461538461538,-0.723076923076922,-0.707692307692307,
-0.692307692307692,-0.676923076923076,-0.661538461538461,-0.646153846153846,
-0.63076923076923,-0.615384615384615,-0.6,-0.584615384615384,-0.569230769230769,
-0.553846153846154,-0.538461538461538,-0.523076923076923,-0.507692307692308,
-0.492307692307692,-0.476923076923077,-0.461538461538462,-0.446153846153846,
-0.430769230769231,-0.415384615384615,-0.4,-0.384615384615385,-0.369230769230769,
-0.353846153846154,-0.338461538461538,-0.323076923076923,-0.307692307692308,
-0.292307692307692,-0.276923076923077,-0.261538461538462,-0.246153846153846,
-0.230769230769231,-0.215384615384615,-0.2,-0.184615384615385,-0.169230769230769,
-0.153846153846154,-0.138461538461538,-0.123076923076923,-0.107692307692308,
-0.0923076923076923,-0.0769230769230769,-0.0615384615384615,-0.0461538461538462,
-0.0307692307692308,-0.0153846153846154,0.),(-1.,1.),.UNSPECIFIED.)
GEOMETRIC_REPRESENTATION_ITEM()
RATIONAL_B_SPLINE_SURFACE(((1.,1.),(1.,1.),(1.,1.),(1.,1.),(1.,1.),(1.,
1.),(1.,1.),(1.,1.),(1.,1.),(1.,1.),(1.,1.),(1.,1.),(1.,1.),(1.,1.),(1.,
1.),(1.,1.),(1.,1.),(1.,1.),(1.,1.),(1.,1.),(1.,1.),(1.,1.),(1.,1.),(1.,
1.),(1.,1.),(1.,1.),(1.,1.),(1.,1.),(1.,1.),(1.,1.),(1.,1.),(1.,1.),(1.,
1.),(1.,1.),(1.,1.),(1.,1.),(1.,1.),(1.,1.),(1.,1.),(1.,1.),(1.,1.),(1.,
1.),(1.,1.),(1.,1.),(1.,1.),(1.,1.),(1.,1.),(1.,1.),(1.,1.),(1.,1.),(1.,
1.),(1.,1.),(1.,1.),(1.,1.),(1.,1.),(1.,1.),(1.,1.),(1.,1.),(1.,1.),(1.,
1.),(1.,1.),(1.,1.),(1.,1.),(1.,1.),(1.,1.),(1.,1.),(1.,1.),(1.,1.),(1.,
1.),(1.,1.)))
REPRESENTATION_ITEM('')
SURFACE()
);
#55=(
BOUNDED_SURFACE()
B_SPLINE_SURFACE(5,1,((#36890,#36891),(#36892,#36893),(#36894,#36895),(#36896,
#36897),(#36898,#36899),(#36900,#36901),(#36902,#36903),(#36904,#36905),
(#36906,#36907),(#36908,#36909),(#36910,#36911),(#36912,#36913),(#36914,
#36915),(#36916,#36917),(#36918,#36919),(#36920,#36921),(#36922,#36923),
(#36924,#36925),(#36926,#36927),(#36928,#36929),(#36930,#36931),(#36932,
#36933),(#36934,#36935),(#36936,#36937),(#36938,#36939),(#36940,#36941),
(#36942,#36943),(#36944,#36945),(#36946,#36947),(#36948,#36949),(#36950,
#36951),(#36952,#36953),(#36954,#36955),(#36956,#36957),(#36958,#36959),
(#36960,#36961),(#36962,#36963),(#36964,#36965),(#36966,#36967),(#36968,
#36969),(#36970,#36971),(#36972,#36973),(#36974,#36975),(#36976,#36977),
(#36978,#36979),(#36980,#36981),(#36982,#36983),(#36984,#36985),(#36986,
#36987),(#36988,#36989),(#36990,#36991),(#36992,#36993),(#36994,#36995),
(#36996,#36997),(#36998,#36999),(#37000,#37001),(#37002,#37003),(#37004,
#37005),(#37006,#37007),(#37008,#37009),(#37010,#37011),(#37012,#37013),
(#37014,#37015),(#37016,#37017),(#37018,#37019),(#37020,#37021),(#37022,
#37023),(#37024,#37025),(#37026,#37027),(#37028,#37029)),.UNSPECIFIED.,
 .F.,.F.,.F.)
B_SPLINE_SURFACE_WITH_KNOTS((6,1,1,1,1,1,1,1,1,1,1,1,1,1,1,1,1,1,1,1,1,
1,1,1,1,1,1,1,1,1,1,1,1,1,1,1,1,1,1,1,1,1,1,1,1,1,1,1,1,1,1,1,1,1,1,1,1,
1,1,1,1,1,1,1,1,6),(2,2),(-1.,-0.984615384615383,-0.969230769230768,-0.953846153846152,
-0.938461538461537,-0.923076923076922,-0.907692307692306,-0.892307692307691,
-0.876923076923076,-0.86153846153846,-0.846153846153845,-0.83076923076923,
-0.815384615384614,-0.799999999999999,-0.784615384615384,-0.769230769230768,
-0.753846153846153,-0.738461538461538,-0.723076923076922,-0.707692307692307,
-0.692307692307692,-0.676923076923076,-0.661538461538461,-0.646153846153846,
-0.63076923076923,-0.615384615384615,-0.6,-0.584615384615384,-0.569230769230769,
-0.553846153846154,-0.538461538461538,-0.523076923076923,-0.507692307692308,
-0.492307692307692,-0.476923076923077,-0.461538461538462,-0.446153846153846,
-0.430769230769231,-0.415384615384615,-0.4,-0.384615384615385,-0.369230769230769,
-0.353846153846154,-0.338461538461538,-0.323076923076923,-0.307692307692308,
-0.292307692307692,-0.276923076923077,-0.261538461538462,-0.246153846153846,
-0.230769230769231,-0.215384615384615,-0.2,-0.184615384615385,-0.169230769230769,
-0.153846153846154,-0.138461538461538,-0.123076923076923,-0.107692307692308,
-0.0923076923076923,-0.0769230769230769,-0.0615384615384615,-0.0461538461538462,
-0.0307692307692308,-0.0153846153846154,0.),(-1.,1.),.UNSPECIFIED.)
GEOMETRIC_REPRESENTATION_ITEM()
RATIONAL_B_SPLINE_SURFACE(((1.,1.),(1.,1.),(1.,1.),(1.,1.),(1.,1.),(1.,
1.),(1.,1.),(1.,1.),(1.,1.),(1.,1.),(1.,1.),(1.,1.),(1.,1.),(1.,1.),(1.,
1.),(1.,1.),(1.,1.),(1.,1.),(1.,1.),(1.,1.),(1.,1.),(1.,1.),(1.,1.),(1.,
1.),(1.,1.),(1.,1.),(1.,1.),(1.,1.),(1.,1.),(1.,1.),(1.,1.),(1.,1.),(1.,
1.),(1.,1.),(1.,1.),(1.,1.),(1.,1.),(1.,1.),(1.,1.),(1.,1.),(1.,1.),(1.,
1.),(1.,1.),(1.,1.),(1.,1.),(1.,1.),(1.,1.),(1.,1.),(1.,1.),(1.,1.),(1.,
1.),(1.,1.),(1.,1.),(1.,1.),(1.,1.),(1.,1.),(1.,1.),(1.,1.),(1.,1.),(1.,
1.),(1.,1.),(1.,1.),(1.,1.),(1.,1.),(1.,1.),(1.,1.),(1.,1.),(1.,1.),(1.,
1.),(1.,1.)))
REPRESENTATION_ITEM('')
SURFACE()
);
#56=(
BOUNDED_SURFACE()
B_SPLINE_SURFACE(5,1,((#37102,#37103),(#37104,#37105),(#37106,#37107),(#37108,
#37109),(#37110,#37111),(#37112,#37113),(#37114,#37115),(#37116,#37117),
(#37118,#37119),(#37120,#37121),(#37122,#37123),(#37124,#37125),(#37126,
#37127),(#37128,#37129),(#37130,#37131),(#37132,#37133),(#37134,#37135),
(#37136,#37137),(#37138,#37139),(#37140,#37141),(#37142,#37143),(#37144,
#37145),(#37146,#37147),(#37148,#37149),(#37150,#37151),(#37152,#37153),
(#37154,#37155),(#37156,#37157),(#37158,#37159),(#37160,#37161),(#37162,
#37163),(#37164,#37165),(#37166,#37167),(#37168,#37169),(#37170,#37171),
(#37172,#37173),(#37174,#37175),(#37176,#37177),(#37178,#37179),(#37180,
#37181),(#37182,#37183),(#37184,#37185),(#37186,#37187),(#37188,#37189),
(#37190,#37191),(#37192,#37193),(#37194,#37195),(#37196,#37197),(#37198,
#37199),(#37200,#37201),(#37202,#37203),(#37204,#37205),(#37206,#37207),
(#37208,#37209),(#37210,#37211),(#37212,#37213),(#37214,#37215),(#37216,
#37217),(#37218,#37219),(#37220,#37221),(#37222,#37223),(#37224,#37225),
(#37226,#37227),(#37228,#37229),(#37230,#37231),(#37232,#37233),(#37234,
#37235),(#37236,#37237),(#37238,#37239),(#37240,#37241)),.UNSPECIFIED.,
 .F.,.F.,.F.)
B_SPLINE_SURFACE_WITH_KNOTS((6,1,1,1,1,1,1,1,1,1,1,1,1,1,1,1,1,1,1,1,1,
1,1,1,1,1,1,1,1,1,1,1,1,1,1,1,1,1,1,1,1,1,1,1,1,1,1,1,1,1,1,1,1,1,1,1,1,
1,1,1,1,1,1,1,1,6),(2,2),(-1.,-0.984615384615383,-0.969230769230768,-0.953846153846152,
-0.938461538461537,-0.923076923076922,-0.907692307692306,-0.892307692307691,
-0.876923076923076,-0.86153846153846,-0.846153846153845,-0.83076923076923,
-0.815384615384614,-0.799999999999999,-0.784615384615384,-0.769230769230768,
-0.753846153846153,-0.738461538461538,-0.723076923076922,-0.707692307692307,
-0.692307692307692,-0.676923076923076,-0.661538461538461,-0.646153846153846,
-0.63076923076923,-0.615384615384615,-0.6,-0.584615384615384,-0.569230769230769,
-0.553846153846154,-0.538461538461538,-0.523076923076923,-0.507692307692308,
-0.492307692307692,-0.476923076923077,-0.461538461538462,-0.446153846153846,
-0.430769230769231,-0.415384615384615,-0.4,-0.384615384615385,-0.369230769230769,
-0.353846153846154,-0.338461538461538,-0.323076923076923,-0.307692307692308,
-0.292307692307692,-0.276923076923077,-0.261538461538462,-0.246153846153846,
-0.230769230769231,-0.215384615384615,-0.2,-0.184615384615385,-0.169230769230769,
-0.153846153846154,-0.138461538461538,-0.123076923076923,-0.107692307692308,
-0.0923076923076923,-0.0769230769230769,-0.0615384615384615,-0.0461538461538462,
-0.0307692307692308,-0.0153846153846154,0.),(-1.,1.),.UNSPECIFIED.)
GEOMETRIC_REPRESENTATION_ITEM()
RATIONAL_B_SPLINE_SURFACE(((1.,1.),(1.,1.),(1.,1.),(1.,1.),(1.,1.),(1.,
1.),(1.,1.),(1.,1.),(1.,1.),(1.,1.),(1.,1.),(1.,1.),(1.,1.),(1.,1.),(1.,
1.),(1.,1.),(1.,1.),(1.,1.),(1.,1.),(1.,1.),(1.,1.),(1.,1.),(1.,1.),(1.,
1.),(1.,1.),(1.,1.),(1.,1.),(1.,1.),(1.,1.),(1.,1.),(1.,1.),(1.,1.),(1.,
1.),(1.,1.),(1.,1.),(1.,1.),(1.,1.),(1.,1.),(1.,1.),(1.,1.),(1.,1.),(1.,
1.),(1.,1.),(1.,1.),(1.,1.),(1.,1.),(1.,1.),(1.,1.),(1.,1.),(1.,1.),(1.,
1.),(1.,1.),(1.,1.),(1.,1.),(1.,1.),(1.,1.),(1.,1.),(1.,1.),(1.,1.),(1.,
1.),(1.,1.),(1.,1.),(1.,1.),(1.,1.),(1.,1.),(1.,1.),(1.,1.),(1.,1.),(1.,
1.),(1.,1.)))
REPRESENTATION_ITEM('')
SURFACE()
);
#57=(
BOUNDED_SURFACE()
B_SPLINE_SURFACE(5,1,((#37332,#37333),(#37334,#37335),(#37336,#37337),(#37338,
#37339),(#37340,#37341),(#37342,#37343),(#37344,#37345),(#37346,#37347),
(#37348,#37349),(#37350,#37351),(#37352,#37353),(#37354,#37355),(#37356,
#37357),(#37358,#37359),(#37360,#37361),(#37362,#37363),(#37364,#37365),
(#37366,#37367),(#37368,#37369),(#37370,#37371),(#37372,#37373),(#37374,
#37375),(#37376,#37377),(#37378,#37379),(#37380,#37381),(#37382,#37383),
(#37384,#37385),(#37386,#37387),(#37388,#37389),(#37390,#37391),(#37392,
#37393),(#37394,#37395),(#37396,#37397),(#37398,#37399),(#37400,#37401),
(#37402,#37403),(#37404,#37405),(#37406,#37407),(#37408,#37409),(#37410,
#37411),(#37412,#37413),(#37414,#37415),(#37416,#37417),(#37418,#37419),
(#37420,#37421),(#37422,#37423),(#37424,#37425),(#37426,#37427),(#37428,
#37429),(#37430,#37431),(#37432,#37433),(#37434,#37435),(#37436,#37437),
(#37438,#37439),(#37440,#37441),(#37442,#37443),(#37444,#37445),(#37446,
#37447),(#37448,#37449),(#37450,#37451),(#37452,#37453),(#37454,#37455),
(#37456,#37457),(#37458,#37459),(#37460,#37461),(#37462,#37463),(#37464,
#37465),(#37466,#37467),(#37468,#37469),(#37470,#37471)),.UNSPECIFIED.,
 .F.,.F.,.F.)
B_SPLINE_SURFACE_WITH_KNOTS((6,1,1,1,1,1,1,1,1,1,1,1,1,1,1,1,1,1,1,1,1,
1,1,1,1,1,1,1,1,1,1,1,1,1,1,1,1,1,1,1,1,1,1,1,1,1,1,1,1,1,1,1,1,1,1,1,1,
1,1,1,1,1,1,1,1,6),(2,2),(-1.,-0.984615384615383,-0.969230769230768,-0.953846153846152,
-0.938461538461537,-0.923076923076922,-0.907692307692306,-0.892307692307691,
-0.876923076923076,-0.86153846153846,-0.846153846153845,-0.83076923076923,
-0.815384615384614,-0.799999999999999,-0.784615384615384,-0.769230769230768,
-0.753846153846153,-0.738461538461538,-0.723076923076922,-0.707692307692307,
-0.692307692307692,-0.676923076923076,-0.661538461538461,-0.646153846153846,
-0.63076923076923,-0.615384615384615,-0.6,-0.584615384615384,-0.569230769230769,
-0.553846153846154,-0.538461538461538,-0.523076923076923,-0.507692307692308,
-0.492307692307692,-0.476923076923077,-0.461538461538462,-0.446153846153846,
-0.430769230769231,-0.415384615384615,-0.4,-0.384615384615385,-0.369230769230769,
-0.353846153846154,-0.338461538461538,-0.323076923076923,-0.307692307692308,
-0.292307692307692,-0.276923076923077,-0.261538461538462,-0.246153846153846,
-0.230769230769231,-0.215384615384615,-0.2,-0.184615384615385,-0.169230769230769,
-0.153846153846154,-0.138461538461538,-0.123076923076923,-0.107692307692308,
-0.0923076923076923,-0.0769230769230769,-0.0615384615384615,-0.0461538461538462,
-0.0307692307692308,-0.0153846153846154,0.),(-1.,1.),.UNSPECIFIED.)
GEOMETRIC_REPRESENTATION_ITEM()
RATIONAL_B_SPLINE_SURFACE(((1.,1.),(1.,1.),(1.,1.),(1.,1.),(1.,1.),(1.,
1.),(1.,1.),(1.,1.),(1.,1.),(1.,1.),(1.,1.),(1.,1.),(1.,1.),(1.,1.),(1.,
1.),(1.,1.),(1.,1.),(1.,1.),(1.,1.),(1.,1.),(1.,1.),(1.,1.),(1.,1.),(1.,
1.),(1.,1.),(1.,1.),(1.,1.),(1.,1.),(1.,1.),(1.,1.),(1.,1.),(1.,1.),(1.,
1.),(1.,1.),(1.,1.),(1.,1.),(1.,1.),(1.,1.),(1.,1.),(1.,1.),(1.,1.),(1.,
1.),(1.,1.),(1.,1.),(1.,1.),(1.,1.),(1.,1.),(1.,1.),(1.,1.),(1.,1.),(1.,
1.),(1.,1.),(1.,1.),(1.,1.),(1.,1.),(1.,1.),(1.,1.),(1.,1.),(1.,1.),(1.,
1.),(1.,1.),(1.,1.),(1.,1.),(1.,1.),(1.,1.),(1.,1.),(1.,1.),(1.,1.),(1.,
1.),(1.,1.)))
REPRESENTATION_ITEM('')
SURFACE()
);
#58=(
BOUNDED_SURFACE()
B_SPLINE_SURFACE(5,1,((#37544,#37545),(#37546,#37547),(#37548,#37549),(#37550,
#37551),(#37552,#37553),(#37554,#37555),(#37556,#37557),(#37558,#37559),
(#37560,#37561),(#37562,#37563),(#37564,#37565),(#37566,#37567),(#37568,
#37569),(#37570,#37571),(#37572,#37573),(#37574,#37575),(#37576,#37577),
(#37578,#37579),(#37580,#37581),(#37582,#37583),(#37584,#37585),(#37586,
#37587),(#37588,#37589),(#37590,#37591),(#37592,#37593),(#37594,#37595),
(#37596,#37597),(#37598,#37599),(#37600,#37601),(#37602,#37603),(#37604,
#37605),(#37606,#37607),(#37608,#37609),(#37610,#37611),(#37612,#37613),
(#37614,#37615),(#37616,#37617),(#37618,#37619),(#37620,#37621),(#37622,
#37623),(#37624,#37625),(#37626,#37627),(#37628,#37629),(#37630,#37631),
(#37632,#37633),(#37634,#37635),(#37636,#37637),(#37638,#37639),(#37640,
#37641),(#37642,#37643),(#37644,#37645),(#37646,#37647),(#37648,#37649),
(#37650,#37651),(#37652,#37653),(#37654,#37655),(#37656,#37657),(#37658,
#37659),(#37660,#37661),(#37662,#37663),(#37664,#37665),(#37666,#37667),
(#37668,#37669),(#37670,#37671),(#37672,#37673),(#37674,#37675),(#37676,
#37677),(#37678,#37679),(#37680,#37681),(#37682,#37683)),.UNSPECIFIED.,
 .F.,.F.,.F.)
B_SPLINE_SURFACE_WITH_KNOTS((6,1,1,1,1,1,1,1,1,1,1,1,1,1,1,1,1,1,1,1,1,
1,1,1,1,1,1,1,1,1,1,1,1,1,1,1,1,1,1,1,1,1,1,1,1,1,1,1,1,1,1,1,1,1,1,1,1,
1,1,1,1,1,1,1,1,6),(2,2),(-1.,-0.984615384615383,-0.969230769230768,-0.953846153846152,
-0.938461538461537,-0.923076923076922,-0.907692307692306,-0.892307692307691,
-0.876923076923076,-0.86153846153846,-0.846153846153845,-0.83076923076923,
-0.815384615384614,-0.799999999999999,-0.784615384615384,-0.769230769230768,
-0.753846153846153,-0.738461538461538,-0.723076923076922,-0.707692307692307,
-0.692307692307692,-0.676923076923076,-0.661538461538461,-0.646153846153846,
-0.63076923076923,-0.615384615384615,-0.6,-0.584615384615384,-0.569230769230769,
-0.553846153846154,-0.538461538461538,-0.523076923076923,-0.507692307692308,
-0.492307692307692,-0.476923076923077,-0.461538461538462,-0.446153846153846,
-0.430769230769231,-0.415384615384615,-0.4,-0.384615384615385,-0.369230769230769,
-0.353846153846154,-0.338461538461538,-0.323076923076923,-0.307692307692308,
-0.292307692307692,-0.276923076923077,-0.261538461538462,-0.246153846153846,
-0.230769230769231,-0.215384615384615,-0.2,-0.184615384615385,-0.169230769230769,
-0.153846153846154,-0.138461538461538,-0.123076923076923,-0.107692307692308,
-0.0923076923076923,-0.0769230769230769,-0.0615384615384615,-0.0461538461538462,
-0.0307692307692308,-0.0153846153846154,0.),(-1.,1.),.UNSPECIFIED.)
GEOMETRIC_REPRESENTATION_ITEM()
RATIONAL_B_SPLINE_SURFACE(((1.,1.),(1.,1.),(1.,1.),(1.,1.),(1.,1.),(1.,
1.),(1.,1.),(1.,1.),(1.,1.),(1.,1.),(1.,1.),(1.,1.),(1.,1.),(1.,1.),(1.,
1.),(1.,1.),(1.,1.),(1.,1.),(1.,1.),(1.,1.),(1.,1.),(1.,1.),(1.,1.),(1.,
1.),(1.,1.),(1.,1.),(1.,1.),(1.,1.),(1.,1.),(1.,1.),(1.,1.),(1.,1.),(1.,
1.),(1.,1.),(1.,1.),(1.,1.),(1.,1.),(1.,1.),(1.,1.),(1.,1.),(1.,1.),(1.,
1.),(1.,1.),(1.,1.),(1.,1.),(1.,1.),(1.,1.),(1.,1.),(1.,1.),(1.,1.),(1.,
1.),(1.,1.),(1.,1.),(1.,1.),(1.,1.),(1.,1.),(1.,1.),(1.,1.),(1.,1.),(1.,
1.),(1.,1.),(1.,1.),(1.,1.),(1.,1.),(1.,1.),(1.,1.),(1.,1.),(1.,1.),(1.,
1.),(1.,1.)))
REPRESENTATION_ITEM('')
SURFACE()
);
#59=(
BOUNDED_SURFACE()
B_SPLINE_SURFACE(5,1,((#37774,#37775),(#37776,#37777),(#37778,#37779),(#37780,
#37781),(#37782,#37783),(#37784,#37785),(#37786,#37787),(#37788,#37789),
(#37790,#37791),(#37792,#37793),(#37794,#37795),(#37796,#37797),(#37798,
#37799),(#37800,#37801),(#37802,#37803),(#37804,#37805),(#37806,#37807),
(#37808,#37809),(#37810,#37811),(#37812,#37813),(#37814,#37815),(#37816,
#37817),(#37818,#37819),(#37820,#37821),(#37822,#37823),(#37824,#37825),
(#37826,#37827),(#37828,#37829),(#37830,#37831),(#37832,#37833),(#37834,
#37835),(#37836,#37837),(#37838,#37839),(#37840,#37841),(#37842,#37843),
(#37844,#37845),(#37846,#37847),(#37848,#37849),(#37850,#37851),(#37852,
#37853),(#37854,#37855),(#37856,#37857),(#37858,#37859),(#37860,#37861),
(#37862,#37863),(#37864,#37865),(#37866,#37867),(#37868,#37869),(#37870,
#37871),(#37872,#37873),(#37874,#37875),(#37876,#37877),(#37878,#37879),
(#37880,#37881),(#37882,#37883),(#37884,#37885),(#37886,#37887),(#37888,
#37889),(#37890,#37891),(#37892,#37893),(#37894,#37895),(#37896,#37897),
(#37898,#37899),(#37900,#37901),(#37902,#37903),(#37904,#37905),(#37906,
#37907),(#37908,#37909),(#37910,#37911),(#37912,#37913)),.UNSPECIFIED.,
 .F.,.F.,.F.)
B_SPLINE_SURFACE_WITH_KNOTS((6,1,1,1,1,1,1,1,1,1,1,1,1,1,1,1,1,1,1,1,1,
1,1,1,1,1,1,1,1,1,1,1,1,1,1,1,1,1,1,1,1,1,1,1,1,1,1,1,1,1,1,1,1,1,1,1,1,
1,1,1,1,1,1,1,1,6),(2,2),(-1.,-0.984615384615383,-0.969230769230768,-0.953846153846152,
-0.938461538461537,-0.923076923076922,-0.907692307692306,-0.892307692307691,
-0.876923076923076,-0.86153846153846,-0.846153846153845,-0.83076923076923,
-0.815384615384614,-0.799999999999999,-0.784615384615384,-0.769230769230768,
-0.753846153846153,-0.738461538461538,-0.723076923076922,-0.707692307692307,
-0.692307692307692,-0.676923076923076,-0.661538461538461,-0.646153846153846,
-0.63076923076923,-0.615384615384615,-0.6,-0.584615384615384,-0.569230769230769,
-0.553846153846154,-0.538461538461538,-0.523076923076923,-0.507692307692308,
-0.492307692307692,-0.476923076923077,-0.461538461538462,-0.446153846153846,
-0.430769230769231,-0.415384615384615,-0.4,-0.384615384615385,-0.369230769230769,
-0.353846153846154,-0.338461538461538,-0.323076923076923,-0.307692307692308,
-0.292307692307692,-0.276923076923077,-0.261538461538462,-0.246153846153846,
-0.230769230769231,-0.215384615384615,-0.2,-0.184615384615385,-0.169230769230769,
-0.153846153846154,-0.138461538461538,-0.123076923076923,-0.107692307692308,
-0.0923076923076923,-0.0769230769230769,-0.0615384615384615,-0.0461538461538462,
-0.0307692307692308,-0.0153846153846154,0.),(-1.,1.),.UNSPECIFIED.)
GEOMETRIC_REPRESENTATION_ITEM()
RATIONAL_B_SPLINE_SURFACE(((1.,1.),(1.,1.),(1.,1.),(1.,1.),(1.,1.),(1.,
1.),(1.,1.),(1.,1.),(1.,1.),(1.,1.),(1.,1.),(1.,1.),(1.,1.),(1.,1.),(1.,
1.),(1.,1.),(1.,1.),(1.,1.),(1.,1.),(1.,1.),(1.,1.),(1.,1.),(1.,1.),(1.,
1.),(1.,1.),(1.,1.),(1.,1.),(1.,1.),(1.,1.),(1.,1.),(1.,1.),(1.,1.),(1.,
1.),(1.,1.),(1.,1.),(1.,1.),(1.,1.),(1.,1.),(1.,1.),(1.,1.),(1.,1.),(1.,
1.),(1.,1.),(1.,1.),(1.,1.),(1.,1.),(1.,1.),(1.,1.),(1.,1.),(1.,1.),(1.,
1.),(1.,1.),(1.,1.),(1.,1.),(1.,1.),(1.,1.),(1.,1.),(1.,1.),(1.,1.),(1.,
1.),(1.,1.),(1.,1.),(1.,1.),(1.,1.),(1.,1.),(1.,1.),(1.,1.),(1.,1.),(1.,
1.),(1.,1.)))
REPRESENTATION_ITEM('')
SURFACE()
);
#60=(
BOUNDED_SURFACE()
B_SPLINE_SURFACE(5,1,((#37986,#37987),(#37988,#37989),(#37990,#37991),(#37992,
#37993),(#37994,#37995),(#37996,#37997),(#37998,#37999),(#38000,#38001),
(#38002,#38003),(#38004,#38005),(#38006,#38007),(#38008,#38009),(#38010,
#38011),(#38012,#38013),(#38014,#38015),(#38016,#38017),(#38018,#38019),
(#38020,#38021),(#38022,#38023),(#38024,#38025),(#38026,#38027),(#38028,
#38029),(#38030,#38031),(#38032,#38033),(#38034,#38035),(#38036,#38037),
(#38038,#38039),(#38040,#38041),(#38042,#38043),(#38044,#38045),(#38046,
#38047),(#38048,#38049),(#38050,#38051),(#38052,#38053),(#38054,#38055),
(#38056,#38057),(#38058,#38059),(#38060,#38061),(#38062,#38063),(#38064,
#38065),(#38066,#38067),(#38068,#38069),(#38070,#38071),(#38072,#38073),
(#38074,#38075),(#38076,#38077),(#38078,#38079),(#38080,#38081),(#38082,
#38083),(#38084,#38085),(#38086,#38087),(#38088,#38089),(#38090,#38091),
(#38092,#38093),(#38094,#38095),(#38096,#38097),(#38098,#38099),(#38100,
#38101),(#38102,#38103),(#38104,#38105),(#38106,#38107),(#38108,#38109),
(#38110,#38111),(#38112,#38113),(#38114,#38115),(#38116,#38117),(#38118,
#38119),(#38120,#38121),(#38122,#38123),(#38124,#38125)),.UNSPECIFIED.,
 .F.,.F.,.F.)
B_SPLINE_SURFACE_WITH_KNOTS((6,1,1,1,1,1,1,1,1,1,1,1,1,1,1,1,1,1,1,1,1,
1,1,1,1,1,1,1,1,1,1,1,1,1,1,1,1,1,1,1,1,1,1,1,1,1,1,1,1,1,1,1,1,1,1,1,1,
1,1,1,1,1,1,1,1,6),(2,2),(-1.,-0.984615384615383,-0.969230769230768,-0.953846153846152,
-0.938461538461537,-0.923076923076922,-0.907692307692306,-0.892307692307691,
-0.876923076923076,-0.86153846153846,-0.846153846153845,-0.83076923076923,
-0.815384615384614,-0.799999999999999,-0.784615384615384,-0.769230769230768,
-0.753846153846153,-0.738461538461538,-0.723076923076922,-0.707692307692307,
-0.692307692307692,-0.676923076923076,-0.661538461538461,-0.646153846153846,
-0.63076923076923,-0.615384615384615,-0.6,-0.584615384615384,-0.569230769230769,
-0.553846153846154,-0.538461538461538,-0.523076923076923,-0.507692307692308,
-0.492307692307692,-0.476923076923077,-0.461538461538462,-0.446153846153846,
-0.430769230769231,-0.415384615384615,-0.4,-0.384615384615385,-0.369230769230769,
-0.353846153846154,-0.338461538461538,-0.323076923076923,-0.307692307692308,
-0.292307692307692,-0.276923076923077,-0.261538461538462,-0.246153846153846,
-0.230769230769231,-0.215384615384615,-0.2,-0.184615384615385,-0.169230769230769,
-0.153846153846154,-0.138461538461538,-0.123076923076923,-0.107692307692308,
-0.0923076923076923,-0.0769230769230769,-0.0615384615384615,-0.0461538461538462,
-0.0307692307692308,-0.0153846153846154,0.),(-1.,1.),.UNSPECIFIED.)
GEOMETRIC_REPRESENTATION_ITEM()
RATIONAL_B_SPLINE_SURFACE(((1.,1.),(1.,1.),(1.,1.),(1.,1.),(1.,1.),(1.,
1.),(1.,1.),(1.,1.),(1.,1.),(1.,1.),(1.,1.),(1.,1.),(1.,1.),(1.,1.),(1.,
1.),(1.,1.),(1.,1.),(1.,1.),(1.,1.),(1.,1.),(1.,1.),(1.,1.),(1.,1.),(1.,
1.),(1.,1.),(1.,1.),(1.,1.),(1.,1.),(1.,1.),(1.,1.),(1.,1.),(1.,1.),(1.,
1.),(1.,1.),(1.,1.),(1.,1.),(1.,1.),(1.,1.),(1.,1.),(1.,1.),(1.,1.),(1.,
1.),(1.,1.),(1.,1.),(1.,1.),(1.,1.),(1.,1.),(1.,1.),(1.,1.),(1.,1.),(1.,
1.),(1.,1.),(1.,1.),(1.,1.),(1.,1.),(1.,1.),(1.,1.),(1.,1.),(1.,1.),(1.,
1.),(1.,1.),(1.,1.),(1.,1.),(1.,1.),(1.,1.),(1.,1.),(1.,1.),(1.,1.),(1.,
1.),(1.,1.)))
REPRESENTATION_ITEM('')
SURFACE()
);
#61=(
BOUNDED_SURFACE()
B_SPLINE_SURFACE(5,1,((#38216,#38217),(#38218,#38219),(#38220,#38221),(#38222,
#38223),(#38224,#38225),(#38226,#38227),(#38228,#38229),(#38230,#38231),
(#38232,#38233),(#38234,#38235),(#38236,#38237),(#38238,#38239),(#38240,
#38241),(#38242,#38243),(#38244,#38245),(#38246,#38247),(#38248,#38249),
(#38250,#38251),(#38252,#38253),(#38254,#38255),(#38256,#38257),(#38258,
#38259),(#38260,#38261),(#38262,#38263),(#38264,#38265),(#38266,#38267),
(#38268,#38269),(#38270,#38271),(#38272,#38273),(#38274,#38275),(#38276,
#38277),(#38278,#38279),(#38280,#38281),(#38282,#38283),(#38284,#38285),
(#38286,#38287),(#38288,#38289),(#38290,#38291),(#38292,#38293),(#38294,
#38295),(#38296,#38297),(#38298,#38299),(#38300,#38301),(#38302,#38303),
(#38304,#38305),(#38306,#38307),(#38308,#38309),(#38310,#38311),(#38312,
#38313),(#38314,#38315),(#38316,#38317),(#38318,#38319),(#38320,#38321),
(#38322,#38323),(#38324,#38325),(#38326,#38327),(#38328,#38329),(#38330,
#38331),(#38332,#38333),(#38334,#38335),(#38336,#38337),(#38338,#38339),
(#38340,#38341),(#38342,#38343),(#38344,#38345),(#38346,#38347),(#38348,
#38349),(#38350,#38351),(#38352,#38353),(#38354,#38355)),.UNSPECIFIED.,
 .F.,.F.,.F.)
B_SPLINE_SURFACE_WITH_KNOTS((6,1,1,1,1,1,1,1,1,1,1,1,1,1,1,1,1,1,1,1,1,
1,1,1,1,1,1,1,1,1,1,1,1,1,1,1,1,1,1,1,1,1,1,1,1,1,1,1,1,1,1,1,1,1,1,1,1,
1,1,1,1,1,1,1,1,6),(2,2),(-1.,-0.984615384615383,-0.969230769230768,-0.953846153846152,
-0.938461538461537,-0.923076923076922,-0.907692307692306,-0.892307692307691,
-0.876923076923076,-0.86153846153846,-0.846153846153845,-0.83076923076923,
-0.815384615384614,-0.799999999999999,-0.784615384615384,-0.769230769230768,
-0.753846153846153,-0.738461538461538,-0.723076923076922,-0.707692307692307,
-0.692307692307692,-0.676923076923076,-0.661538461538461,-0.646153846153846,
-0.63076923076923,-0.615384615384615,-0.6,-0.584615384615384,-0.569230769230769,
-0.553846153846154,-0.538461538461538,-0.523076923076923,-0.507692307692308,
-0.492307692307692,-0.476923076923077,-0.461538461538462,-0.446153846153846,
-0.430769230769231,-0.415384615384615,-0.4,-0.384615384615385,-0.369230769230769,
-0.353846153846154,-0.338461538461538,-0.323076923076923,-0.307692307692308,
-0.292307692307692,-0.276923076923077,-0.261538461538462,-0.246153846153846,
-0.230769230769231,-0.215384615384615,-0.2,-0.184615384615385,-0.169230769230769,
-0.153846153846154,-0.138461538461538,-0.123076923076923,-0.107692307692308,
-0.0923076923076923,-0.0769230769230769,-0.0615384615384615,-0.0461538461538462,
-0.0307692307692308,-0.0153846153846154,0.),(-1.,1.),.UNSPECIFIED.)
GEOMETRIC_REPRESENTATION_ITEM()
RATIONAL_B_SPLINE_SURFACE(((1.,1.),(1.,1.),(1.,1.),(1.,1.),(1.,1.),(1.,
1.),(1.,1.),(1.,1.),(1.,1.),(1.,1.),(1.,1.),(1.,1.),(1.,1.),(1.,1.),(1.,
1.),(1.,1.),(1.,1.),(1.,1.),(1.,1.),(1.,1.),(1.,1.),(1.,1.),(1.,1.),(1.,
1.),(1.,1.),(1.,1.),(1.,1.),(1.,1.),(1.,1.),(1.,1.),(1.,1.),(1.,1.),(1.,
1.),(1.,1.),(1.,1.),(1.,1.),(1.,1.),(1.,1.),(1.,1.),(1.,1.),(1.,1.),(1.,
1.),(1.,1.),(1.,1.),(1.,1.),(1.,1.),(1.,1.),(1.,1.),(1.,1.),(1.,1.),(1.,
1.),(1.,1.),(1.,1.),(1.,1.),(1.,1.),(1.,1.),(1.,1.),(1.,1.),(1.,1.),(1.,
1.),(1.,1.),(1.,1.),(1.,1.),(1.,1.),(1.,1.),(1.,1.),(1.,1.),(1.,1.),(1.,
1.),(1.,1.)))
REPRESENTATION_ITEM('')
SURFACE()
);
#62=(
BOUNDED_SURFACE()
B_SPLINE_SURFACE(5,1,((#38428,#38429),(#38430,#38431),(#38432,#38433),(#38434,
#38435),(#38436,#38437),(#38438,#38439),(#38440,#38441),(#38442,#38443),
(#38444,#38445),(#38446,#38447),(#38448,#38449),(#38450,#38451),(#38452,
#38453),(#38454,#38455),(#38456,#38457),(#38458,#38459),(#38460,#38461),
(#38462,#38463),(#38464,#38465),(#38466,#38467),(#38468,#38469),(#38470,
#38471),(#38472,#38473),(#38474,#38475),(#38476,#38477),(#38478,#38479),
(#38480,#38481),(#38482,#38483),(#38484,#38485),(#38486,#38487),(#38488,
#38489),(#38490,#38491),(#38492,#38493),(#38494,#38495),(#38496,#38497),
(#38498,#38499),(#38500,#38501),(#38502,#38503),(#38504,#38505),(#38506,
#38507),(#38508,#38509),(#38510,#38511),(#38512,#38513),(#38514,#38515),
(#38516,#38517),(#38518,#38519),(#38520,#38521),(#38522,#38523),(#38524,
#38525),(#38526,#38527),(#38528,#38529),(#38530,#38531),(#38532,#38533),
(#38534,#38535),(#38536,#38537),(#38538,#38539),(#38540,#38541),(#38542,
#38543),(#38544,#38545),(#38546,#38547),(#38548,#38549),(#38550,#38551),
(#38552,#38553),(#38554,#38555),(#38556,#38557),(#38558,#38559),(#38560,
#38561),(#38562,#38563),(#38564,#38565),(#38566,#38567)),.UNSPECIFIED.,
 .F.,.F.,.F.)
B_SPLINE_SURFACE_WITH_KNOTS((6,1,1,1,1,1,1,1,1,1,1,1,1,1,1,1,1,1,1,1,1,
1,1,1,1,1,1,1,1,1,1,1,1,1,1,1,1,1,1,1,1,1,1,1,1,1,1,1,1,1,1,1,1,1,1,1,1,
1,1,1,1,1,1,1,1,6),(2,2),(-1.,-0.984615384615383,-0.969230769230768,-0.953846153846152,
-0.938461538461537,-0.923076923076922,-0.907692307692306,-0.892307692307691,
-0.876923076923076,-0.86153846153846,-0.846153846153845,-0.83076923076923,
-0.815384615384614,-0.799999999999999,-0.784615384615384,-0.769230769230768,
-0.753846153846153,-0.738461538461538,-0.723076923076922,-0.707692307692307,
-0.692307692307692,-0.676923076923076,-0.661538461538461,-0.646153846153846,
-0.63076923076923,-0.615384615384615,-0.6,-0.584615384615384,-0.569230769230769,
-0.553846153846154,-0.538461538461538,-0.523076923076923,-0.507692307692308,
-0.492307692307692,-0.476923076923077,-0.461538461538462,-0.446153846153846,
-0.430769230769231,-0.415384615384615,-0.4,-0.384615384615385,-0.369230769230769,
-0.353846153846154,-0.338461538461538,-0.323076923076923,-0.307692307692308,
-0.292307692307692,-0.276923076923077,-0.261538461538462,-0.246153846153846,
-0.230769230769231,-0.215384615384615,-0.2,-0.184615384615385,-0.169230769230769,
-0.153846153846154,-0.138461538461538,-0.123076923076923,-0.107692307692308,
-0.0923076923076923,-0.0769230769230769,-0.0615384615384615,-0.0461538461538462,
-0.0307692307692308,-0.0153846153846154,0.),(-1.,1.),.UNSPECIFIED.)
GEOMETRIC_REPRESENTATION_ITEM()
RATIONAL_B_SPLINE_SURFACE(((1.,1.),(1.,1.),(1.,1.),(1.,1.),(1.,1.),(1.,
1.),(1.,1.),(1.,1.),(1.,1.),(1.,1.),(1.,1.),(1.,1.),(1.,1.),(1.,1.),(1.,
1.),(1.,1.),(1.,1.),(1.,1.),(1.,1.),(1.,1.),(1.,1.),(1.,1.),(1.,1.),(1.,
1.),(1.,1.),(1.,1.),(1.,1.),(1.,1.),(1.,1.),(1.,1.),(1.,1.),(1.,1.),(1.,
1.),(1.,1.),(1.,1.),(1.,1.),(1.,1.),(1.,1.),(1.,1.),(1.,1.),(1.,1.),(1.,
1.),(1.,1.),(1.,1.),(1.,1.),(1.,1.),(1.,1.),(1.,1.),(1.,1.),(1.,1.),(1.,
1.),(1.,1.),(1.,1.),(1.,1.),(1.,1.),(1.,1.),(1.,1.),(1.,1.),(1.,1.),(1.,
1.),(1.,1.),(1.,1.),(1.,1.),(1.,1.),(1.,1.),(1.,1.),(1.,1.),(1.,1.),(1.,
1.),(1.,1.)))
REPRESENTATION_ITEM('')
SURFACE()
);
#63=(
BOUNDED_SURFACE()
B_SPLINE_SURFACE(5,1,((#38658,#38659),(#38660,#38661),(#38662,#38663),(#38664,
#38665),(#38666,#38667),(#38668,#38669),(#38670,#38671),(#38672,#38673),
(#38674,#38675),(#38676,#38677),(#38678,#38679),(#38680,#38681),(#38682,
#38683),(#38684,#38685),(#38686,#38687),(#38688,#38689),(#38690,#38691),
(#38692,#38693),(#38694,#38695),(#38696,#38697),(#38698,#38699),(#38700,
#38701),(#38702,#38703),(#38704,#38705),(#38706,#38707),(#38708,#38709),
(#38710,#38711),(#38712,#38713),(#38714,#38715),(#38716,#38717),(#38718,
#38719),(#38720,#38721),(#38722,#38723),(#38724,#38725),(#38726,#38727),
(#38728,#38729),(#38730,#38731),(#38732,#38733),(#38734,#38735),(#38736,
#38737),(#38738,#38739),(#38740,#38741),(#38742,#38743),(#38744,#38745),
(#38746,#38747),(#38748,#38749),(#38750,#38751),(#38752,#38753),(#38754,
#38755),(#38756,#38757),(#38758,#38759),(#38760,#38761),(#38762,#38763),
(#38764,#38765),(#38766,#38767),(#38768,#38769),(#38770,#38771),(#38772,
#38773),(#38774,#38775),(#38776,#38777),(#38778,#38779),(#38780,#38781),
(#38782,#38783),(#38784,#38785),(#38786,#38787),(#38788,#38789),(#38790,
#38791),(#38792,#38793),(#38794,#38795),(#38796,#38797)),.UNSPECIFIED.,
 .F.,.F.,.F.)
B_SPLINE_SURFACE_WITH_KNOTS((6,1,1,1,1,1,1,1,1,1,1,1,1,1,1,1,1,1,1,1,1,
1,1,1,1,1,1,1,1,1,1,1,1,1,1,1,1,1,1,1,1,1,1,1,1,1,1,1,1,1,1,1,1,1,1,1,1,
1,1,1,1,1,1,1,1,6),(2,2),(-1.,-0.984615384615383,-0.969230769230768,-0.953846153846152,
-0.938461538461537,-0.923076923076922,-0.907692307692306,-0.892307692307691,
-0.876923076923076,-0.86153846153846,-0.846153846153845,-0.83076923076923,
-0.815384615384614,-0.799999999999999,-0.784615384615384,-0.769230769230768,
-0.753846153846153,-0.738461538461538,-0.723076923076922,-0.707692307692307,
-0.692307692307692,-0.676923076923076,-0.661538461538461,-0.646153846153846,
-0.63076923076923,-0.615384615384615,-0.6,-0.584615384615384,-0.569230769230769,
-0.553846153846154,-0.538461538461538,-0.523076923076923,-0.507692307692308,
-0.492307692307692,-0.476923076923077,-0.461538461538462,-0.446153846153846,
-0.430769230769231,-0.415384615384615,-0.4,-0.384615384615385,-0.369230769230769,
-0.353846153846154,-0.338461538461538,-0.323076923076923,-0.307692307692308,
-0.292307692307692,-0.276923076923077,-0.261538461538462,-0.246153846153846,
-0.230769230769231,-0.215384615384615,-0.2,-0.184615384615385,-0.169230769230769,
-0.153846153846154,-0.138461538461538,-0.123076923076923,-0.107692307692308,
-0.0923076923076923,-0.0769230769230769,-0.0615384615384615,-0.0461538461538462,
-0.0307692307692308,-0.0153846153846154,0.),(-1.,1.),.UNSPECIFIED.)
GEOMETRIC_REPRESENTATION_ITEM()
RATIONAL_B_SPLINE_SURFACE(((1.,1.),(1.,1.),(1.,1.),(1.,1.),(1.,1.),(1.,
1.),(1.,1.),(1.,1.),(1.,1.),(1.,1.),(1.,1.),(1.,1.),(1.,1.),(1.,1.),(1.,
1.),(1.,1.),(1.,1.),(1.,1.),(1.,1.),(1.,1.),(1.,1.),(1.,1.),(1.,1.),(1.,
1.),(1.,1.),(1.,1.),(1.,1.),(1.,1.),(1.,1.),(1.,1.),(1.,1.),(1.,1.),(1.,
1.),(1.,1.),(1.,1.),(1.,1.),(1.,1.),(1.,1.),(1.,1.),(1.,1.),(1.,1.),(1.,
1.),(1.,1.),(1.,1.),(1.,1.),(1.,1.),(1.,1.),(1.,1.),(1.,1.),(1.,1.),(1.,
1.),(1.,1.),(1.,1.),(1.,1.),(1.,1.),(1.,1.),(1.,1.),(1.,1.),(1.,1.),(1.,
1.),(1.,1.),(1.,1.),(1.,1.),(1.,1.),(1.,1.),(1.,1.),(1.,1.),(1.,1.),(1.,
1.),(1.,1.)))
REPRESENTATION_ITEM('')
SURFACE()
);
#64=(
BOUNDED_SURFACE()
B_SPLINE_SURFACE(5,1,((#38870,#38871),(#38872,#38873),(#38874,#38875),(#38876,
#38877),(#38878,#38879),(#38880,#38881),(#38882,#38883),(#38884,#38885),
(#38886,#38887),(#38888,#38889),(#38890,#38891),(#38892,#38893),(#38894,
#38895),(#38896,#38897),(#38898,#38899),(#38900,#38901),(#38902,#38903),
(#38904,#38905),(#38906,#38907),(#38908,#38909),(#38910,#38911),(#38912,
#38913),(#38914,#38915),(#38916,#38917),(#38918,#38919),(#38920,#38921),
(#38922,#38923),(#38924,#38925),(#38926,#38927),(#38928,#38929),(#38930,
#38931),(#38932,#38933),(#38934,#38935),(#38936,#38937),(#38938,#38939),
(#38940,#38941),(#38942,#38943),(#38944,#38945),(#38946,#38947),(#38948,
#38949),(#38950,#38951),(#38952,#38953),(#38954,#38955),(#38956,#38957),
(#38958,#38959),(#38960,#38961),(#38962,#38963),(#38964,#38965),(#38966,
#38967),(#38968,#38969),(#38970,#38971),(#38972,#38973),(#38974,#38975),
(#38976,#38977),(#38978,#38979),(#38980,#38981),(#38982,#38983),(#38984,
#38985),(#38986,#38987),(#38988,#38989),(#38990,#38991),(#38992,#38993),
(#38994,#38995),(#38996,#38997),(#38998,#38999),(#39000,#39001),(#39002,
#39003),(#39004,#39005),(#39006,#39007),(#39008,#39009)),.UNSPECIFIED.,
 .F.,.F.,.F.)
B_SPLINE_SURFACE_WITH_KNOTS((6,1,1,1,1,1,1,1,1,1,1,1,1,1,1,1,1,1,1,1,1,
1,1,1,1,1,1,1,1,1,1,1,1,1,1,1,1,1,1,1,1,1,1,1,1,1,1,1,1,1,1,1,1,1,1,1,1,
1,1,1,1,1,1,1,1,6),(2,2),(-1.,-0.984615384615383,-0.969230769230768,-0.953846153846152,
-0.938461538461537,-0.923076923076922,-0.907692307692306,-0.892307692307691,
-0.876923076923076,-0.86153846153846,-0.846153846153845,-0.83076923076923,
-0.815384615384614,-0.799999999999999,-0.784615384615384,-0.769230769230768,
-0.753846153846153,-0.738461538461538,-0.723076923076922,-0.707692307692307,
-0.692307692307692,-0.676923076923076,-0.661538461538461,-0.646153846153846,
-0.63076923076923,-0.615384615384615,-0.6,-0.584615384615384,-0.569230769230769,
-0.553846153846154,-0.538461538461538,-0.523076923076923,-0.507692307692308,
-0.492307692307692,-0.476923076923077,-0.461538461538462,-0.446153846153846,
-0.430769230769231,-0.415384615384615,-0.4,-0.384615384615385,-0.369230769230769,
-0.353846153846154,-0.338461538461538,-0.323076923076923,-0.307692307692308,
-0.292307692307692,-0.276923076923077,-0.261538461538462,-0.246153846153846,
-0.230769230769231,-0.215384615384615,-0.2,-0.184615384615385,-0.169230769230769,
-0.153846153846154,-0.138461538461538,-0.123076923076923,-0.107692307692308,
-0.0923076923076923,-0.0769230769230769,-0.0615384615384615,-0.0461538461538462,
-0.0307692307692308,-0.0153846153846154,0.),(-1.,1.),.UNSPECIFIED.)
GEOMETRIC_REPRESENTATION_ITEM()
RATIONAL_B_SPLINE_SURFACE(((1.,1.),(1.,1.),(1.,1.),(1.,1.),(1.,1.),(1.,
1.),(1.,1.),(1.,1.),(1.,1.),(1.,1.),(1.,1.),(1.,1.),(1.,1.),(1.,1.),(1.,
1.),(1.,1.),(1.,1.),(1.,1.),(1.,1.),(1.,1.),(1.,1.),(1.,1.),(1.,1.),(1.,
1.),(1.,1.),(1.,1.),(1.,1.),(1.,1.),(1.,1.),(1.,1.),(1.,1.),(1.,1.),(1.,
1.),(1.,1.),(1.,1.),(1.,1.),(1.,1.),(1.,1.),(1.,1.),(1.,1.),(1.,1.),(1.,
1.),(1.,1.),(1.,1.),(1.,1.),(1.,1.),(1.,1.),(1.,1.),(1.,1.),(1.,1.),(1.,
1.),(1.,1.),(1.,1.),(1.,1.),(1.,1.),(1.,1.),(1.,1.),(1.,1.),(1.,1.),(1.,
1.),(1.,1.),(1.,1.),(1.,1.),(1.,1.),(1.,1.),(1.,1.),(1.,1.),(1.,1.),(1.,
1.),(1.,1.)))
REPRESENTATION_ITEM('')
SURFACE()
);
#65=(
BOUNDED_SURFACE()
B_SPLINE_SURFACE(5,1,((#39100,#39101),(#39102,#39103),(#39104,#39105),(#39106,
#39107),(#39108,#39109),(#39110,#39111),(#39112,#39113),(#39114,#39115),
(#39116,#39117),(#39118,#39119),(#39120,#39121),(#39122,#39123),(#39124,
#39125),(#39126,#39127),(#39128,#39129),(#39130,#39131),(#39132,#39133),
(#39134,#39135),(#39136,#39137),(#39138,#39139),(#39140,#39141),(#39142,
#39143),(#39144,#39145),(#39146,#39147),(#39148,#39149),(#39150,#39151),
(#39152,#39153),(#39154,#39155),(#39156,#39157),(#39158,#39159),(#39160,
#39161),(#39162,#39163),(#39164,#39165),(#39166,#39167),(#39168,#39169),
(#39170,#39171),(#39172,#39173),(#39174,#39175),(#39176,#39177),(#39178,
#39179),(#39180,#39181),(#39182,#39183),(#39184,#39185),(#39186,#39187),
(#39188,#39189),(#39190,#39191),(#39192,#39193),(#39194,#39195),(#39196,
#39197),(#39198,#39199),(#39200,#39201),(#39202,#39203),(#39204,#39205),
(#39206,#39207),(#39208,#39209),(#39210,#39211),(#39212,#39213),(#39214,
#39215),(#39216,#39217),(#39218,#39219),(#39220,#39221),(#39222,#39223),
(#39224,#39225),(#39226,#39227),(#39228,#39229),(#39230,#39231),(#39232,
#39233),(#39234,#39235),(#39236,#39237),(#39238,#39239)),.UNSPECIFIED.,
 .F.,.F.,.F.)
B_SPLINE_SURFACE_WITH_KNOTS((6,1,1,1,1,1,1,1,1,1,1,1,1,1,1,1,1,1,1,1,1,
1,1,1,1,1,1,1,1,1,1,1,1,1,1,1,1,1,1,1,1,1,1,1,1,1,1,1,1,1,1,1,1,1,1,1,1,
1,1,1,1,1,1,1,1,6),(2,2),(-1.,-0.984615384615383,-0.969230769230768,-0.953846153846152,
-0.938461538461537,-0.923076923076922,-0.907692307692306,-0.892307692307691,
-0.876923076923076,-0.86153846153846,-0.846153846153845,-0.83076923076923,
-0.815384615384614,-0.799999999999999,-0.784615384615384,-0.769230769230768,
-0.753846153846153,-0.738461538461538,-0.723076923076922,-0.707692307692307,
-0.692307692307692,-0.676923076923076,-0.661538461538461,-0.646153846153846,
-0.63076923076923,-0.615384615384615,-0.6,-0.584615384615384,-0.569230769230769,
-0.553846153846154,-0.538461538461538,-0.523076923076923,-0.507692307692308,
-0.492307692307692,-0.476923076923077,-0.461538461538462,-0.446153846153846,
-0.430769230769231,-0.415384615384615,-0.4,-0.384615384615385,-0.369230769230769,
-0.353846153846154,-0.338461538461538,-0.323076923076923,-0.307692307692308,
-0.292307692307692,-0.276923076923077,-0.261538461538462,-0.246153846153846,
-0.230769230769231,-0.215384615384615,-0.2,-0.184615384615385,-0.169230769230769,
-0.153846153846154,-0.138461538461538,-0.123076923076923,-0.107692307692308,
-0.0923076923076923,-0.0769230769230769,-0.0615384615384615,-0.0461538461538462,
-0.0307692307692308,-0.0153846153846154,0.),(-1.,1.),.UNSPECIFIED.)
GEOMETRIC_REPRESENTATION_ITEM()
RATIONAL_B_SPLINE_SURFACE(((1.,1.),(1.,1.),(1.,1.),(1.,1.),(1.,1.),(1.,
1.),(1.,1.),(1.,1.),(1.,1.),(1.,1.),(1.,1.),(1.,1.),(1.,1.),(1.,1.),(1.,
1.),(1.,1.),(1.,1.),(1.,1.),(1.,1.),(1.,1.),(1.,1.),(1.,1.),(1.,1.),(1.,
1.),(1.,1.),(1.,1.),(1.,1.),(1.,1.),(1.,1.),(1.,1.),(1.,1.),(1.,1.),(1.,
1.),(1.,1.),(1.,1.),(1.,1.),(1.,1.),(1.,1.),(1.,1.),(1.,1.),(1.,1.),(1.,
1.),(1.,1.),(1.,1.),(1.,1.),(1.,1.),(1.,1.),(1.,1.),(1.,1.),(1.,1.),(1.,
1.),(1.,1.),(1.,1.),(1.,1.),(1.,1.),(1.,1.),(1.,1.),(1.,1.),(1.,1.),(1.,
1.),(1.,1.),(1.,1.),(1.,1.),(1.,1.),(1.,1.),(1.,1.),(1.,1.),(1.,1.),(1.,
1.),(1.,1.)))
REPRESENTATION_ITEM('')
SURFACE()
);
#66=(
BOUNDED_SURFACE()
B_SPLINE_SURFACE(5,1,((#39312,#39313),(#39314,#39315),(#39316,#39317),(#39318,
#39319),(#39320,#39321),(#39322,#39323),(#39324,#39325),(#39326,#39327),
(#39328,#39329),(#39330,#39331),(#39332,#39333),(#39334,#39335),(#39336,
#39337),(#39338,#39339),(#39340,#39341),(#39342,#39343),(#39344,#39345),
(#39346,#39347),(#39348,#39349),(#39350,#39351),(#39352,#39353),(#39354,
#39355),(#39356,#39357),(#39358,#39359),(#39360,#39361),(#39362,#39363),
(#39364,#39365),(#39366,#39367),(#39368,#39369),(#39370,#39371),(#39372,
#39373),(#39374,#39375),(#39376,#39377),(#39378,#39379),(#39380,#39381),
(#39382,#39383),(#39384,#39385),(#39386,#39387),(#39388,#39389),(#39390,
#39391),(#39392,#39393),(#39394,#39395),(#39396,#39397),(#39398,#39399),
(#39400,#39401),(#39402,#39403),(#39404,#39405),(#39406,#39407),(#39408,
#39409),(#39410,#39411),(#39412,#39413),(#39414,#39415),(#39416,#39417),
(#39418,#39419),(#39420,#39421),(#39422,#39423),(#39424,#39425),(#39426,
#39427),(#39428,#39429),(#39430,#39431),(#39432,#39433),(#39434,#39435),
(#39436,#39437),(#39438,#39439),(#39440,#39441),(#39442,#39443),(#39444,
#39445),(#39446,#39447),(#39448,#39449),(#39450,#39451)),.UNSPECIFIED.,
 .F.,.F.,.F.)
B_SPLINE_SURFACE_WITH_KNOTS((6,1,1,1,1,1,1,1,1,1,1,1,1,1,1,1,1,1,1,1,1,
1,1,1,1,1,1,1,1,1,1,1,1,1,1,1,1,1,1,1,1,1,1,1,1,1,1,1,1,1,1,1,1,1,1,1,1,
1,1,1,1,1,1,1,1,6),(2,2),(-1.,-0.984615384615383,-0.969230769230768,-0.953846153846152,
-0.938461538461537,-0.923076923076922,-0.907692307692306,-0.892307692307691,
-0.876923076923076,-0.86153846153846,-0.846153846153845,-0.83076923076923,
-0.815384615384614,-0.799999999999999,-0.784615384615384,-0.769230769230768,
-0.753846153846153,-0.738461538461538,-0.723076923076922,-0.707692307692307,
-0.692307692307692,-0.676923076923076,-0.661538461538461,-0.646153846153846,
-0.63076923076923,-0.615384615384615,-0.6,-0.584615384615384,-0.569230769230769,
-0.553846153846154,-0.538461538461538,-0.523076923076923,-0.507692307692308,
-0.492307692307692,-0.476923076923077,-0.461538461538462,-0.446153846153846,
-0.430769230769231,-0.415384615384615,-0.4,-0.384615384615385,-0.369230769230769,
-0.353846153846154,-0.338461538461538,-0.323076923076923,-0.307692307692308,
-0.292307692307692,-0.276923076923077,-0.261538461538462,-0.246153846153846,
-0.230769230769231,-0.215384615384615,-0.2,-0.184615384615385,-0.169230769230769,
-0.153846153846154,-0.138461538461538,-0.123076923076923,-0.107692307692308,
-0.0923076923076923,-0.0769230769230769,-0.0615384615384615,-0.0461538461538462,
-0.0307692307692308,-0.0153846153846154,0.),(-1.,1.),.UNSPECIFIED.)
GEOMETRIC_REPRESENTATION_ITEM()
RATIONAL_B_SPLINE_SURFACE(((1.,1.),(1.,1.),(1.,1.),(1.,1.),(1.,1.),(1.,
1.),(1.,1.),(1.,1.),(1.,1.),(1.,1.),(1.,1.),(1.,1.),(1.,1.),(1.,1.),(1.,
1.),(1.,1.),(1.,1.),(1.,1.),(1.,1.),(1.,1.),(1.,1.),(1.,1.),(1.,1.),(1.,
1.),(1.,1.),(1.,1.),(1.,1.),(1.,1.),(1.,1.),(1.,1.),(1.,1.),(1.,1.),(1.,
1.),(1.,1.),(1.,1.),(1.,1.),(1.,1.),(1.,1.),(1.,1.),(1.,1.),(1.,1.),(1.,
1.),(1.,1.),(1.,1.),(1.,1.),(1.,1.),(1.,1.),(1.,1.),(1.,1.),(1.,1.),(1.,
1.),(1.,1.),(1.,1.),(1.,1.),(1.,1.),(1.,1.),(1.,1.),(1.,1.),(1.,1.),(1.,
1.),(1.,1.),(1.,1.),(1.,1.),(1.,1.),(1.,1.),(1.,1.),(1.,1.),(1.,1.),(1.,
1.),(1.,1.)))
REPRESENTATION_ITEM('')
SURFACE()
);
#67=(
BOUNDED_SURFACE()
B_SPLINE_SURFACE(5,1,((#39542,#39543),(#39544,#39545),(#39546,#39547),(#39548,
#39549),(#39550,#39551),(#39552,#39553),(#39554,#39555),(#39556,#39557),
(#39558,#39559),(#39560,#39561),(#39562,#39563),(#39564,#39565),(#39566,
#39567),(#39568,#39569),(#39570,#39571),(#39572,#39573),(#39574,#39575),
(#39576,#39577),(#39578,#39579),(#39580,#39581),(#39582,#39583),(#39584,
#39585),(#39586,#39587),(#39588,#39589),(#39590,#39591),(#39592,#39593),
(#39594,#39595),(#39596,#39597),(#39598,#39599),(#39600,#39601),(#39602,
#39603),(#39604,#39605),(#39606,#39607),(#39608,#39609),(#39610,#39611),
(#39612,#39613),(#39614,#39615),(#39616,#39617),(#39618,#39619),(#39620,
#39621),(#39622,#39623),(#39624,#39625),(#39626,#39627),(#39628,#39629),
(#39630,#39631),(#39632,#39633),(#39634,#39635),(#39636,#39637),(#39638,
#39639),(#39640,#39641),(#39642,#39643),(#39644,#39645),(#39646,#39647),
(#39648,#39649),(#39650,#39651),(#39652,#39653),(#39654,#39655),(#39656,
#39657),(#39658,#39659),(#39660,#39661),(#39662,#39663),(#39664,#39665),
(#39666,#39667),(#39668,#39669),(#39670,#39671),(#39672,#39673),(#39674,
#39675),(#39676,#39677),(#39678,#39679),(#39680,#39681)),.UNSPECIFIED.,
 .F.,.F.,.F.)
B_SPLINE_SURFACE_WITH_KNOTS((6,1,1,1,1,1,1,1,1,1,1,1,1,1,1,1,1,1,1,1,1,
1,1,1,1,1,1,1,1,1,1,1,1,1,1,1,1,1,1,1,1,1,1,1,1,1,1,1,1,1,1,1,1,1,1,1,1,
1,1,1,1,1,1,1,1,6),(2,2),(-1.,-0.984615384615383,-0.969230769230768,-0.953846153846152,
-0.938461538461537,-0.923076923076922,-0.907692307692306,-0.892307692307691,
-0.876923076923076,-0.86153846153846,-0.846153846153845,-0.83076923076923,
-0.815384615384614,-0.799999999999999,-0.784615384615384,-0.769230769230768,
-0.753846153846153,-0.738461538461538,-0.723076923076922,-0.707692307692307,
-0.692307692307692,-0.676923076923076,-0.661538461538461,-0.646153846153846,
-0.63076923076923,-0.615384615384615,-0.6,-0.584615384615384,-0.569230769230769,
-0.553846153846154,-0.538461538461538,-0.523076923076923,-0.507692307692308,
-0.492307692307692,-0.476923076923077,-0.461538461538462,-0.446153846153846,
-0.430769230769231,-0.415384615384615,-0.4,-0.384615384615385,-0.369230769230769,
-0.353846153846154,-0.338461538461538,-0.323076923076923,-0.307692307692308,
-0.292307692307692,-0.276923076923077,-0.261538461538462,-0.246153846153846,
-0.230769230769231,-0.215384615384615,-0.2,-0.184615384615385,-0.169230769230769,
-0.153846153846154,-0.138461538461538,-0.123076923076923,-0.107692307692308,
-0.0923076923076923,-0.0769230769230769,-0.0615384615384615,-0.0461538461538462,
-0.0307692307692308,-0.0153846153846154,0.),(-1.,1.),.UNSPECIFIED.)
GEOMETRIC_REPRESENTATION_ITEM()
RATIONAL_B_SPLINE_SURFACE(((1.,1.),(1.,1.),(1.,1.),(1.,1.),(1.,1.),(1.,
1.),(1.,1.),(1.,1.),(1.,1.),(1.,1.),(1.,1.),(1.,1.),(1.,1.),(1.,1.),(1.,
1.),(1.,1.),(1.,1.),(1.,1.),(1.,1.),(1.,1.),(1.,1.),(1.,1.),(1.,1.),(1.,
1.),(1.,1.),(1.,1.),(1.,1.),(1.,1.),(1.,1.),(1.,1.),(1.,1.),(1.,1.),(1.,
1.),(1.,1.),(1.,1.),(1.,1.),(1.,1.),(1.,1.),(1.,1.),(1.,1.),(1.,1.),(1.,
1.),(1.,1.),(1.,1.),(1.,1.),(1.,1.),(1.,1.),(1.,1.),(1.,1.),(1.,1.),(1.,
1.),(1.,1.),(1.,1.),(1.,1.),(1.,1.),(1.,1.),(1.,1.),(1.,1.),(1.,1.),(1.,
1.),(1.,1.),(1.,1.),(1.,1.),(1.,1.),(1.,1.),(1.,1.),(1.,1.),(1.,1.),(1.,
1.),(1.,1.)))
REPRESENTATION_ITEM('')
SURFACE()
);
#68=(
BOUNDED_SURFACE()
B_SPLINE_SURFACE(5,1,((#39754,#39755),(#39756,#39757),(#39758,#39759),(#39760,
#39761),(#39762,#39763),(#39764,#39765),(#39766,#39767),(#39768,#39769),
(#39770,#39771),(#39772,#39773),(#39774,#39775),(#39776,#39777),(#39778,
#39779),(#39780,#39781),(#39782,#39783),(#39784,#39785),(#39786,#39787),
(#39788,#39789),(#39790,#39791),(#39792,#39793),(#39794,#39795),(#39796,
#39797),(#39798,#39799),(#39800,#39801),(#39802,#39803),(#39804,#39805),
(#39806,#39807),(#39808,#39809),(#39810,#39811),(#39812,#39813),(#39814,
#39815),(#39816,#39817),(#39818,#39819),(#39820,#39821),(#39822,#39823),
(#39824,#39825),(#39826,#39827),(#39828,#39829),(#39830,#39831),(#39832,
#39833),(#39834,#39835),(#39836,#39837),(#39838,#39839),(#39840,#39841),
(#39842,#39843),(#39844,#39845),(#39846,#39847),(#39848,#39849),(#39850,
#39851),(#39852,#39853),(#39854,#39855),(#39856,#39857),(#39858,#39859),
(#39860,#39861),(#39862,#39863),(#39864,#39865),(#39866,#39867),(#39868,
#39869),(#39870,#39871),(#39872,#39873),(#39874,#39875),(#39876,#39877),
(#39878,#39879),(#39880,#39881),(#39882,#39883),(#39884,#39885),(#39886,
#39887),(#39888,#39889),(#39890,#39891),(#39892,#39893)),.UNSPECIFIED.,
 .F.,.F.,.F.)
B_SPLINE_SURFACE_WITH_KNOTS((6,1,1,1,1,1,1,1,1,1,1,1,1,1,1,1,1,1,1,1,1,
1,1,1,1,1,1,1,1,1,1,1,1,1,1,1,1,1,1,1,1,1,1,1,1,1,1,1,1,1,1,1,1,1,1,1,1,
1,1,1,1,1,1,1,1,6),(2,2),(-1.,-0.984615384615383,-0.969230769230768,-0.953846153846152,
-0.938461538461537,-0.923076923076922,-0.907692307692306,-0.892307692307691,
-0.876923076923076,-0.86153846153846,-0.846153846153845,-0.83076923076923,
-0.815384615384614,-0.799999999999999,-0.784615384615384,-0.769230769230768,
-0.753846153846153,-0.738461538461538,-0.723076923076922,-0.707692307692307,
-0.692307692307692,-0.676923076923076,-0.661538461538461,-0.646153846153846,
-0.63076923076923,-0.615384615384615,-0.6,-0.584615384615384,-0.569230769230769,
-0.553846153846154,-0.538461538461538,-0.523076923076923,-0.507692307692308,
-0.492307692307692,-0.476923076923077,-0.461538461538462,-0.446153846153846,
-0.430769230769231,-0.415384615384615,-0.4,-0.384615384615385,-0.369230769230769,
-0.353846153846154,-0.338461538461538,-0.323076923076923,-0.307692307692308,
-0.292307692307692,-0.276923076923077,-0.261538461538462,-0.246153846153846,
-0.230769230769231,-0.215384615384615,-0.2,-0.184615384615385,-0.169230769230769,
-0.153846153846154,-0.138461538461538,-0.123076923076923,-0.107692307692308,
-0.0923076923076923,-0.0769230769230769,-0.0615384615384615,-0.0461538461538462,
-0.0307692307692308,-0.0153846153846154,0.),(-1.,1.),.UNSPECIFIED.)
GEOMETRIC_REPRESENTATION_ITEM()
RATIONAL_B_SPLINE_SURFACE(((1.,1.),(1.,1.),(1.,1.),(1.,1.),(1.,1.),(1.,
1.),(1.,1.),(1.,1.),(1.,1.),(1.,1.),(1.,1.),(1.,1.),(1.,1.),(1.,1.),(1.,
1.),(1.,1.),(1.,1.),(1.,1.),(1.,1.),(1.,1.),(1.,1.),(1.,1.),(1.,1.),(1.,
1.),(1.,1.),(1.,1.),(1.,1.),(1.,1.),(1.,1.),(1.,1.),(1.,1.),(1.,1.),(1.,
1.),(1.,1.),(1.,1.),(1.,1.),(1.,1.),(1.,1.),(1.,1.),(1.,1.),(1.,1.),(1.,
1.),(1.,1.),(1.,1.),(1.,1.),(1.,1.),(1.,1.),(1.,1.),(1.,1.),(1.,1.),(1.,
1.),(1.,1.),(1.,1.),(1.,1.),(1.,1.),(1.,1.),(1.,1.),(1.,1.),(1.,1.),(1.,
1.),(1.,1.),(1.,1.),(1.,1.),(1.,1.),(1.,1.),(1.,1.),(1.,1.),(1.,1.),(1.,
1.),(1.,1.)))
REPRESENTATION_ITEM('')
SURFACE()
);
#69=(
BOUNDED_SURFACE()
B_SPLINE_SURFACE(5,1,((#39984,#39985),(#39986,#39987),(#39988,#39989),(#39990,
#39991),(#39992,#39993),(#39994,#39995),(#39996,#39997),(#39998,#39999),
(#40000,#40001),(#40002,#40003),(#40004,#40005),(#40006,#40007),(#40008,
#40009),(#40010,#40011),(#40012,#40013),(#40014,#40015),(#40016,#40017),
(#40018,#40019),(#40020,#40021),(#40022,#40023),(#40024,#40025),(#40026,
#40027),(#40028,#40029),(#40030,#40031),(#40032,#40033),(#40034,#40035),
(#40036,#40037),(#40038,#40039),(#40040,#40041),(#40042,#40043),(#40044,
#40045),(#40046,#40047),(#40048,#40049),(#40050,#40051),(#40052,#40053),
(#40054,#40055),(#40056,#40057),(#40058,#40059),(#40060,#40061),(#40062,
#40063),(#40064,#40065),(#40066,#40067),(#40068,#40069),(#40070,#40071),
(#40072,#40073),(#40074,#40075),(#40076,#40077),(#40078,#40079),(#40080,
#40081),(#40082,#40083),(#40084,#40085),(#40086,#40087),(#40088,#40089),
(#40090,#40091),(#40092,#40093),(#40094,#40095),(#40096,#40097),(#40098,
#40099),(#40100,#40101),(#40102,#40103),(#40104,#40105),(#40106,#40107),
(#40108,#40109),(#40110,#40111),(#40112,#40113),(#40114,#40115),(#40116,
#40117),(#40118,#40119),(#40120,#40121),(#40122,#40123)),.UNSPECIFIED.,
 .F.,.F.,.F.)
B_SPLINE_SURFACE_WITH_KNOTS((6,1,1,1,1,1,1,1,1,1,1,1,1,1,1,1,1,1,1,1,1,
1,1,1,1,1,1,1,1,1,1,1,1,1,1,1,1,1,1,1,1,1,1,1,1,1,1,1,1,1,1,1,1,1,1,1,1,
1,1,1,1,1,1,1,1,6),(2,2),(-1.,-0.984615384615383,-0.969230769230768,-0.953846153846152,
-0.938461538461537,-0.923076923076922,-0.907692307692306,-0.892307692307691,
-0.876923076923076,-0.86153846153846,-0.846153846153845,-0.83076923076923,
-0.815384615384614,-0.799999999999999,-0.784615384615384,-0.769230769230768,
-0.753846153846153,-0.738461538461538,-0.723076923076922,-0.707692307692307,
-0.692307692307692,-0.676923076923076,-0.661538461538461,-0.646153846153846,
-0.63076923076923,-0.615384615384615,-0.6,-0.584615384615384,-0.569230769230769,
-0.553846153846154,-0.538461538461538,-0.523076923076923,-0.507692307692308,
-0.492307692307692,-0.476923076923077,-0.461538461538462,-0.446153846153846,
-0.430769230769231,-0.415384615384615,-0.4,-0.384615384615385,-0.369230769230769,
-0.353846153846154,-0.338461538461538,-0.323076923076923,-0.307692307692308,
-0.292307692307692,-0.276923076923077,-0.261538461538462,-0.246153846153846,
-0.230769230769231,-0.215384615384615,-0.2,-0.184615384615385,-0.169230769230769,
-0.153846153846154,-0.138461538461538,-0.123076923076923,-0.107692307692308,
-0.0923076923076923,-0.0769230769230769,-0.0615384615384615,-0.0461538461538462,
-0.0307692307692308,-0.0153846153846154,0.),(-1.,1.),.UNSPECIFIED.)
GEOMETRIC_REPRESENTATION_ITEM()
RATIONAL_B_SPLINE_SURFACE(((1.,1.),(1.,1.),(1.,1.),(1.,1.),(1.,1.),(1.,
1.),(1.,1.),(1.,1.),(1.,1.),(1.,1.),(1.,1.),(1.,1.),(1.,1.),(1.,1.),(1.,
1.),(1.,1.),(1.,1.),(1.,1.),(1.,1.),(1.,1.),(1.,1.),(1.,1.),(1.,1.),(1.,
1.),(1.,1.),(1.,1.),(1.,1.),(1.,1.),(1.,1.),(1.,1.),(1.,1.),(1.,1.),(1.,
1.),(1.,1.),(1.,1.),(1.,1.),(1.,1.),(1.,1.),(1.,1.),(1.,1.),(1.,1.),(1.,
1.),(1.,1.),(1.,1.),(1.,1.),(1.,1.),(1.,1.),(1.,1.),(1.,1.),(1.,1.),(1.,
1.),(1.,1.),(1.,1.),(1.,1.),(1.,1.),(1.,1.),(1.,1.),(1.,1.),(1.,1.),(1.,
1.),(1.,1.),(1.,1.),(1.,1.),(1.,1.),(1.,1.),(1.,1.),(1.,1.),(1.,1.),(1.,
1.),(1.,1.)))
REPRESENTATION_ITEM('')
SURFACE()
);
#70=(
BOUNDED_SURFACE()
B_SPLINE_SURFACE(5,1,((#40196,#40197),(#40198,#40199),(#40200,#40201),(#40202,
#40203),(#40204,#40205),(#40206,#40207),(#40208,#40209),(#40210,#40211),
(#40212,#40213),(#40214,#40215),(#40216,#40217),(#40218,#40219),(#40220,
#40221),(#40222,#40223),(#40224,#40225),(#40226,#40227),(#40228,#40229),
(#40230,#40231),(#40232,#40233),(#40234,#40235),(#40236,#40237),(#40238,
#40239),(#40240,#40241),(#40242,#40243),(#40244,#40245),(#40246,#40247),
(#40248,#40249),(#40250,#40251),(#40252,#40253),(#40254,#40255),(#40256,
#40257),(#40258,#40259),(#40260,#40261),(#40262,#40263),(#40264,#40265),
(#40266,#40267),(#40268,#40269),(#40270,#40271),(#40272,#40273),(#40274,
#40275),(#40276,#40277),(#40278,#40279),(#40280,#40281),(#40282,#40283),
(#40284,#40285),(#40286,#40287),(#40288,#40289),(#40290,#40291),(#40292,
#40293),(#40294,#40295),(#40296,#40297),(#40298,#40299),(#40300,#40301),
(#40302,#40303),(#40304,#40305),(#40306,#40307),(#40308,#40309),(#40310,
#40311),(#40312,#40313),(#40314,#40315),(#40316,#40317),(#40318,#40319),
(#40320,#40321),(#40322,#40323),(#40324,#40325),(#40326,#40327),(#40328,
#40329),(#40330,#40331),(#40332,#40333),(#40334,#40335)),.UNSPECIFIED.,
 .F.,.F.,.F.)
B_SPLINE_SURFACE_WITH_KNOTS((6,1,1,1,1,1,1,1,1,1,1,1,1,1,1,1,1,1,1,1,1,
1,1,1,1,1,1,1,1,1,1,1,1,1,1,1,1,1,1,1,1,1,1,1,1,1,1,1,1,1,1,1,1,1,1,1,1,
1,1,1,1,1,1,1,1,6),(2,2),(-1.,-0.984615384615383,-0.969230769230768,-0.953846153846152,
-0.938461538461537,-0.923076923076922,-0.907692307692306,-0.892307692307691,
-0.876923076923076,-0.86153846153846,-0.846153846153845,-0.83076923076923,
-0.815384615384614,-0.799999999999999,-0.784615384615384,-0.769230769230768,
-0.753846153846153,-0.738461538461538,-0.723076923076922,-0.707692307692307,
-0.692307692307692,-0.676923076923076,-0.661538461538461,-0.646153846153846,
-0.63076923076923,-0.615384615384615,-0.6,-0.584615384615384,-0.569230769230769,
-0.553846153846154,-0.538461538461538,-0.523076923076923,-0.507692307692308,
-0.492307692307692,-0.476923076923077,-0.461538461538462,-0.446153846153846,
-0.430769230769231,-0.415384615384615,-0.4,-0.384615384615385,-0.369230769230769,
-0.353846153846154,-0.338461538461538,-0.323076923076923,-0.307692307692308,
-0.292307692307692,-0.276923076923077,-0.261538461538462,-0.246153846153846,
-0.230769230769231,-0.215384615384615,-0.2,-0.184615384615385,-0.169230769230769,
-0.153846153846154,-0.138461538461538,-0.123076923076923,-0.107692307692308,
-0.0923076923076923,-0.0769230769230769,-0.0615384615384615,-0.0461538461538462,
-0.0307692307692308,-0.0153846153846154,0.),(-1.,1.),.UNSPECIFIED.)
GEOMETRIC_REPRESENTATION_ITEM()
RATIONAL_B_SPLINE_SURFACE(((1.,1.),(1.,1.),(1.,1.),(1.,1.),(1.,1.),(1.,
1.),(1.,1.),(1.,1.),(1.,1.),(1.,1.),(1.,1.),(1.,1.),(1.,1.),(1.,1.),(1.,
1.),(1.,1.),(1.,1.),(1.,1.),(1.,1.),(1.,1.),(1.,1.),(1.,1.),(1.,1.),(1.,
1.),(1.,1.),(1.,1.),(1.,1.),(1.,1.),(1.,1.),(1.,1.),(1.,1.),(1.,1.),(1.,
1.),(1.,1.),(1.,1.),(1.,1.),(1.,1.),(1.,1.),(1.,1.),(1.,1.),(1.,1.),(1.,
1.),(1.,1.),(1.,1.),(1.,1.),(1.,1.),(1.,1.),(1.,1.),(1.,1.),(1.,1.),(1.,
1.),(1.,1.),(1.,1.),(1.,1.),(1.,1.),(1.,1.),(1.,1.),(1.,1.),(1.,1.),(1.,
1.),(1.,1.),(1.,1.),(1.,1.),(1.,1.),(1.,1.),(1.,1.),(1.,1.),(1.,1.),(1.,
1.),(1.,1.)))
REPRESENTATION_ITEM('')
SURFACE()
);
#71=(
BOUNDED_SURFACE()
B_SPLINE_SURFACE(5,1,((#40426,#40427),(#40428,#40429),(#40430,#40431),(#40432,
#40433),(#40434,#40435),(#40436,#40437),(#40438,#40439),(#40440,#40441),
(#40442,#40443),(#40444,#40445),(#40446,#40447),(#40448,#40449),(#40450,
#40451),(#40452,#40453),(#40454,#40455),(#40456,#40457),(#40458,#40459),
(#40460,#40461),(#40462,#40463),(#40464,#40465),(#40466,#40467),(#40468,
#40469),(#40470,#40471),(#40472,#40473),(#40474,#40475),(#40476,#40477),
(#40478,#40479),(#40480,#40481),(#40482,#40483),(#40484,#40485),(#40486,
#40487),(#40488,#40489),(#40490,#40491),(#40492,#40493),(#40494,#40495),
(#40496,#40497),(#40498,#40499),(#40500,#40501),(#40502,#40503),(#40504,
#40505),(#40506,#40507),(#40508,#40509),(#40510,#40511),(#40512,#40513),
(#40514,#40515),(#40516,#40517),(#40518,#40519),(#40520,#40521),(#40522,
#40523),(#40524,#40525),(#40526,#40527),(#40528,#40529),(#40530,#40531),
(#40532,#40533),(#40534,#40535),(#40536,#40537),(#40538,#40539),(#40540,
#40541),(#40542,#40543),(#40544,#40545),(#40546,#40547),(#40548,#40549),
(#40550,#40551),(#40552,#40553),(#40554,#40555),(#40556,#40557),(#40558,
#40559),(#40560,#40561),(#40562,#40563),(#40564,#40565)),.UNSPECIFIED.,
 .F.,.F.,.F.)
B_SPLINE_SURFACE_WITH_KNOTS((6,1,1,1,1,1,1,1,1,1,1,1,1,1,1,1,1,1,1,1,1,
1,1,1,1,1,1,1,1,1,1,1,1,1,1,1,1,1,1,1,1,1,1,1,1,1,1,1,1,1,1,1,1,1,1,1,1,
1,1,1,1,1,1,1,1,6),(2,2),(-1.,-0.984615384615383,-0.969230769230768,-0.953846153846152,
-0.938461538461537,-0.923076923076922,-0.907692307692306,-0.892307692307691,
-0.876923076923076,-0.86153846153846,-0.846153846153845,-0.83076923076923,
-0.815384615384614,-0.799999999999999,-0.784615384615384,-0.769230769230768,
-0.753846153846153,-0.738461538461538,-0.723076923076922,-0.707692307692307,
-0.692307692307692,-0.676923076923076,-0.661538461538461,-0.646153846153846,
-0.63076923076923,-0.615384615384615,-0.6,-0.584615384615384,-0.569230769230769,
-0.553846153846154,-0.538461538461538,-0.523076923076923,-0.507692307692308,
-0.492307692307692,-0.476923076923077,-0.461538461538462,-0.446153846153846,
-0.430769230769231,-0.415384615384615,-0.4,-0.384615384615385,-0.369230769230769,
-0.353846153846154,-0.338461538461538,-0.323076923076923,-0.307692307692308,
-0.292307692307692,-0.276923076923077,-0.261538461538462,-0.246153846153846,
-0.230769230769231,-0.215384615384615,-0.2,-0.184615384615385,-0.169230769230769,
-0.153846153846154,-0.138461538461538,-0.123076923076923,-0.107692307692308,
-0.0923076923076923,-0.0769230769230769,-0.0615384615384615,-0.0461538461538462,
-0.0307692307692308,-0.0153846153846154,0.),(-1.,1.),.UNSPECIFIED.)
GEOMETRIC_REPRESENTATION_ITEM()
RATIONAL_B_SPLINE_SURFACE(((1.,1.),(1.,1.),(1.,1.),(1.,1.),(1.,1.),(1.,
1.),(1.,1.),(1.,1.),(1.,1.),(1.,1.),(1.,1.),(1.,1.),(1.,1.),(1.,1.),(1.,
1.),(1.,1.),(1.,1.),(1.,1.),(1.,1.),(1.,1.),(1.,1.),(1.,1.),(1.,1.),(1.,
1.),(1.,1.),(1.,1.),(1.,1.),(1.,1.),(1.,1.),(1.,1.),(1.,1.),(1.,1.),(1.,
1.),(1.,1.),(1.,1.),(1.,1.),(1.,1.),(1.,1.),(1.,1.),(1.,1.),(1.,1.),(1.,
1.),(1.,1.),(1.,1.),(1.,1.),(1.,1.),(1.,1.),(1.,1.),(1.,1.),(1.,1.),(1.,
1.),(1.,1.),(1.,1.),(1.,1.),(1.,1.),(1.,1.),(1.,1.),(1.,1.),(1.,1.),(1.,
1.),(1.,1.),(1.,1.),(1.,1.),(1.,1.),(1.,1.),(1.,1.),(1.,1.),(1.,1.),(1.,
1.),(1.,1.)))
REPRESENTATION_ITEM('')
SURFACE()
);
#72=(
BOUNDED_SURFACE()
B_SPLINE_SURFACE(5,1,((#40638,#40639),(#40640,#40641),(#40642,#40643),(#40644,
#40645),(#40646,#40647),(#40648,#40649),(#40650,#40651),(#40652,#40653),
(#40654,#40655),(#40656,#40657),(#40658,#40659),(#40660,#40661),(#40662,
#40663),(#40664,#40665),(#40666,#40667),(#40668,#40669),(#40670,#40671),
(#40672,#40673),(#40674,#40675),(#40676,#40677),(#40678,#40679),(#40680,
#40681),(#40682,#40683),(#40684,#40685),(#40686,#40687),(#40688,#40689),
(#40690,#40691),(#40692,#40693),(#40694,#40695),(#40696,#40697),(#40698,
#40699),(#40700,#40701),(#40702,#40703),(#40704,#40705),(#40706,#40707),
(#40708,#40709),(#40710,#40711),(#40712,#40713),(#40714,#40715),(#40716,
#40717),(#40718,#40719),(#40720,#40721),(#40722,#40723),(#40724,#40725),
(#40726,#40727),(#40728,#40729),(#40730,#40731),(#40732,#40733),(#40734,
#40735),(#40736,#40737),(#40738,#40739),(#40740,#40741),(#40742,#40743),
(#40744,#40745),(#40746,#40747),(#40748,#40749),(#40750,#40751),(#40752,
#40753),(#40754,#40755),(#40756,#40757),(#40758,#40759),(#40760,#40761),
(#40762,#40763),(#40764,#40765),(#40766,#40767),(#40768,#40769),(#40770,
#40771),(#40772,#40773),(#40774,#40775),(#40776,#40777)),.UNSPECIFIED.,
 .F.,.F.,.F.)
B_SPLINE_SURFACE_WITH_KNOTS((6,1,1,1,1,1,1,1,1,1,1,1,1,1,1,1,1,1,1,1,1,
1,1,1,1,1,1,1,1,1,1,1,1,1,1,1,1,1,1,1,1,1,1,1,1,1,1,1,1,1,1,1,1,1,1,1,1,
1,1,1,1,1,1,1,1,6),(2,2),(-1.,-0.984615384615383,-0.969230769230768,-0.953846153846152,
-0.938461538461537,-0.923076923076922,-0.907692307692306,-0.892307692307691,
-0.876923076923076,-0.86153846153846,-0.846153846153845,-0.83076923076923,
-0.815384615384614,-0.799999999999999,-0.784615384615384,-0.769230769230768,
-0.753846153846153,-0.738461538461538,-0.723076923076922,-0.707692307692307,
-0.692307692307692,-0.676923076923076,-0.661538461538461,-0.646153846153846,
-0.63076923076923,-0.615384615384615,-0.6,-0.584615384615384,-0.569230769230769,
-0.553846153846154,-0.538461538461538,-0.523076923076923,-0.507692307692308,
-0.492307692307692,-0.476923076923077,-0.461538461538462,-0.446153846153846,
-0.430769230769231,-0.415384615384615,-0.4,-0.384615384615385,-0.369230769230769,
-0.353846153846154,-0.338461538461538,-0.323076923076923,-0.307692307692308,
-0.292307692307692,-0.276923076923077,-0.261538461538462,-0.246153846153846,
-0.230769230769231,-0.215384615384615,-0.2,-0.184615384615385,-0.169230769230769,
-0.153846153846154,-0.138461538461538,-0.123076923076923,-0.107692307692308,
-0.0923076923076923,-0.0769230769230769,-0.0615384615384615,-0.0461538461538462,
-0.0307692307692308,-0.0153846153846154,0.),(-1.,1.),.UNSPECIFIED.)
GEOMETRIC_REPRESENTATION_ITEM()
RATIONAL_B_SPLINE_SURFACE(((1.,1.),(1.,1.),(1.,1.),(1.,1.),(1.,1.),(1.,
1.),(1.,1.),(1.,1.),(1.,1.),(1.,1.),(1.,1.),(1.,1.),(1.,1.),(1.,1.),(1.,
1.),(1.,1.),(1.,1.),(1.,1.),(1.,1.),(1.,1.),(1.,1.),(1.,1.),(1.,1.),(1.,
1.),(1.,1.),(1.,1.),(1.,1.),(1.,1.),(1.,1.),(1.,1.),(1.,1.),(1.,1.),(1.,
1.),(1.,1.),(1.,1.),(1.,1.),(1.,1.),(1.,1.),(1.,1.),(1.,1.),(1.,1.),(1.,
1.),(1.,1.),(1.,1.),(1.,1.),(1.,1.),(1.,1.),(1.,1.),(1.,1.),(1.,1.),(1.,
1.),(1.,1.),(1.,1.),(1.,1.),(1.,1.),(1.,1.),(1.,1.),(1.,1.),(1.,1.),(1.,
1.),(1.,1.),(1.,1.),(1.,1.),(1.,1.),(1.,1.),(1.,1.),(1.,1.),(1.,1.),(1.,
1.),(1.,1.)))
REPRESENTATION_ITEM('')
SURFACE()
);
#73=(
BOUNDED_SURFACE()
B_SPLINE_SURFACE(5,1,((#40868,#40869),(#40870,#40871),(#40872,#40873),(#40874,
#40875),(#40876,#40877),(#40878,#40879),(#40880,#40881),(#40882,#40883),
(#40884,#40885),(#40886,#40887),(#40888,#40889),(#40890,#40891),(#40892,
#40893),(#40894,#40895),(#40896,#40897),(#40898,#40899),(#40900,#40901),
(#40902,#40903),(#40904,#40905),(#40906,#40907),(#40908,#40909),(#40910,
#40911),(#40912,#40913),(#40914,#40915),(#40916,#40917),(#40918,#40919),
(#40920,#40921),(#40922,#40923),(#40924,#40925),(#40926,#40927),(#40928,
#40929),(#40930,#40931),(#40932,#40933),(#40934,#40935),(#40936,#40937),
(#40938,#40939),(#40940,#40941),(#40942,#40943),(#40944,#40945),(#40946,
#40947),(#40948,#40949),(#40950,#40951),(#40952,#40953),(#40954,#40955),
(#40956,#40957),(#40958,#40959),(#40960,#40961),(#40962,#40963),(#40964,
#40965),(#40966,#40967),(#40968,#40969),(#40970,#40971),(#40972,#40973),
(#40974,#40975),(#40976,#40977),(#40978,#40979),(#40980,#40981),(#40982,
#40983),(#40984,#40985),(#40986,#40987),(#40988,#40989),(#40990,#40991),
(#40992,#40993),(#40994,#40995),(#40996,#40997),(#40998,#40999),(#41000,
#41001),(#41002,#41003),(#41004,#41005),(#41006,#41007)),.UNSPECIFIED.,
 .F.,.F.,.F.)
B_SPLINE_SURFACE_WITH_KNOTS((6,1,1,1,1,1,1,1,1,1,1,1,1,1,1,1,1,1,1,1,1,
1,1,1,1,1,1,1,1,1,1,1,1,1,1,1,1,1,1,1,1,1,1,1,1,1,1,1,1,1,1,1,1,1,1,1,1,
1,1,1,1,1,1,1,1,6),(2,2),(-1.,-0.984615384615383,-0.969230769230768,-0.953846153846152,
-0.938461538461537,-0.923076923076922,-0.907692307692306,-0.892307692307691,
-0.876923076923076,-0.86153846153846,-0.846153846153845,-0.83076923076923,
-0.815384615384614,-0.799999999999999,-0.784615384615384,-0.769230769230768,
-0.753846153846153,-0.738461538461538,-0.723076923076922,-0.707692307692307,
-0.692307692307692,-0.676923076923076,-0.661538461538461,-0.646153846153846,
-0.63076923076923,-0.615384615384615,-0.6,-0.584615384615384,-0.569230769230769,
-0.553846153846154,-0.538461538461538,-0.523076923076923,-0.507692307692308,
-0.492307692307692,-0.476923076923077,-0.461538461538462,-0.446153846153846,
-0.430769230769231,-0.415384615384615,-0.4,-0.384615384615385,-0.369230769230769,
-0.353846153846154,-0.338461538461538,-0.323076923076923,-0.307692307692308,
-0.292307692307692,-0.276923076923077,-0.261538461538462,-0.246153846153846,
-0.230769230769231,-0.215384615384615,-0.2,-0.184615384615385,-0.169230769230769,
-0.153846153846154,-0.138461538461538,-0.123076923076923,-0.107692307692308,
-0.0923076923076923,-0.0769230769230769,-0.0615384615384615,-0.0461538461538462,
-0.0307692307692308,-0.0153846153846154,0.),(-1.,1.),.UNSPECIFIED.)
GEOMETRIC_REPRESENTATION_ITEM()
RATIONAL_B_SPLINE_SURFACE(((1.,1.),(1.,1.),(1.,1.),(1.,1.),(1.,1.),(1.,
1.),(1.,1.),(1.,1.),(1.,1.),(1.,1.),(1.,1.),(1.,1.),(1.,1.),(1.,1.),(1.,
1.),(1.,1.),(1.,1.),(1.,1.),(1.,1.),(1.,1.),(1.,1.),(1.,1.),(1.,1.),(1.,
1.),(1.,1.),(1.,1.),(1.,1.),(1.,1.),(1.,1.),(1.,1.),(1.,1.),(1.,1.),(1.,
1.),(1.,1.),(1.,1.),(1.,1.),(1.,1.),(1.,1.),(1.,1.),(1.,1.),(1.,1.),(1.,
1.),(1.,1.),(1.,1.),(1.,1.),(1.,1.),(1.,1.),(1.,1.),(1.,1.),(1.,1.),(1.,
1.),(1.,1.),(1.,1.),(1.,1.),(1.,1.),(1.,1.),(1.,1.),(1.,1.),(1.,1.),(1.,
1.),(1.,1.),(1.,1.),(1.,1.),(1.,1.),(1.,1.),(1.,1.),(1.,1.),(1.,1.),(1.,
1.),(1.,1.)))
REPRESENTATION_ITEM('')
SURFACE()
);
#74=(
BOUNDED_SURFACE()
B_SPLINE_SURFACE(5,1,((#41080,#41081),(#41082,#41083),(#41084,#41085),(#41086,
#41087),(#41088,#41089),(#41090,#41091),(#41092,#41093),(#41094,#41095),
(#41096,#41097),(#41098,#41099),(#41100,#41101),(#41102,#41103),(#41104,
#41105),(#41106,#41107),(#41108,#41109),(#41110,#41111),(#41112,#41113),
(#41114,#41115),(#41116,#41117),(#41118,#41119),(#41120,#41121),(#41122,
#41123),(#41124,#41125),(#41126,#41127),(#41128,#41129),(#41130,#41131),
(#41132,#41133),(#41134,#41135),(#41136,#41137),(#41138,#41139),(#41140,
#41141),(#41142,#41143),(#41144,#41145),(#41146,#41147),(#41148,#41149),
(#41150,#41151),(#41152,#41153),(#41154,#41155),(#41156,#41157),(#41158,
#41159),(#41160,#41161),(#41162,#41163),(#41164,#41165),(#41166,#41167),
(#41168,#41169),(#41170,#41171),(#41172,#41173),(#41174,#41175),(#41176,
#41177),(#41178,#41179),(#41180,#41181),(#41182,#41183),(#41184,#41185),
(#41186,#41187),(#41188,#41189),(#41190,#41191),(#41192,#41193),(#41194,
#41195),(#41196,#41197),(#41198,#41199),(#41200,#41201),(#41202,#41203),
(#41204,#41205),(#41206,#41207),(#41208,#41209),(#41210,#41211),(#41212,
#41213),(#41214,#41215),(#41216,#41217),(#41218,#41219)),.UNSPECIFIED.,
 .F.,.F.,.F.)
B_SPLINE_SURFACE_WITH_KNOTS((6,1,1,1,1,1,1,1,1,1,1,1,1,1,1,1,1,1,1,1,1,
1,1,1,1,1,1,1,1,1,1,1,1,1,1,1,1,1,1,1,1,1,1,1,1,1,1,1,1,1,1,1,1,1,1,1,1,
1,1,1,1,1,1,1,1,6),(2,2),(-1.,-0.984615384615383,-0.969230769230768,-0.953846153846152,
-0.938461538461537,-0.923076923076922,-0.907692307692306,-0.892307692307691,
-0.876923076923076,-0.86153846153846,-0.846153846153845,-0.83076923076923,
-0.815384615384614,-0.799999999999999,-0.784615384615384,-0.769230769230768,
-0.753846153846153,-0.738461538461538,-0.723076923076922,-0.707692307692307,
-0.692307692307692,-0.676923076923076,-0.661538461538461,-0.646153846153846,
-0.63076923076923,-0.615384615384615,-0.6,-0.584615384615384,-0.569230769230769,
-0.553846153846154,-0.538461538461538,-0.523076923076923,-0.507692307692308,
-0.492307692307692,-0.476923076923077,-0.461538461538462,-0.446153846153846,
-0.430769230769231,-0.415384615384615,-0.4,-0.384615384615385,-0.369230769230769,
-0.353846153846154,-0.338461538461538,-0.323076923076923,-0.307692307692308,
-0.292307692307692,-0.276923076923077,-0.261538461538462,-0.246153846153846,
-0.230769230769231,-0.215384615384615,-0.2,-0.184615384615385,-0.169230769230769,
-0.153846153846154,-0.138461538461538,-0.123076923076923,-0.107692307692308,
-0.0923076923076923,-0.0769230769230769,-0.0615384615384615,-0.0461538461538462,
-0.0307692307692308,-0.0153846153846154,0.),(-1.,1.),.UNSPECIFIED.)
GEOMETRIC_REPRESENTATION_ITEM()
RATIONAL_B_SPLINE_SURFACE(((1.,1.),(1.,1.),(1.,1.),(1.,1.),(1.,1.),(1.,
1.),(1.,1.),(1.,1.),(1.,1.),(1.,1.),(1.,1.),(1.,1.),(1.,1.),(1.,1.),(1.,
1.),(1.,1.),(1.,1.),(1.,1.),(1.,1.),(1.,1.),(1.,1.),(1.,1.),(1.,1.),(1.,
1.),(1.,1.),(1.,1.),(1.,1.),(1.,1.),(1.,1.),(1.,1.),(1.,1.),(1.,1.),(1.,
1.),(1.,1.),(1.,1.),(1.,1.),(1.,1.),(1.,1.),(1.,1.),(1.,1.),(1.,1.),(1.,
1.),(1.,1.),(1.,1.),(1.,1.),(1.,1.),(1.,1.),(1.,1.),(1.,1.),(1.,1.),(1.,
1.),(1.,1.),(1.,1.),(1.,1.),(1.,1.),(1.,1.),(1.,1.),(1.,1.),(1.,1.),(1.,
1.),(1.,1.),(1.,1.),(1.,1.),(1.,1.),(1.,1.),(1.,1.),(1.,1.),(1.,1.),(1.,
1.),(1.,1.)))
REPRESENTATION_ITEM('')
SURFACE()
);
#75=(
BOUNDED_SURFACE()
B_SPLINE_SURFACE(5,1,((#41310,#41311),(#41312,#41313),(#41314,#41315),(#41316,
#41317),(#41318,#41319),(#41320,#41321),(#41322,#41323),(#41324,#41325),
(#41326,#41327),(#41328,#41329),(#41330,#41331),(#41332,#41333),(#41334,
#41335),(#41336,#41337),(#41338,#41339),(#41340,#41341),(#41342,#41343),
(#41344,#41345),(#41346,#41347),(#41348,#41349),(#41350,#41351),(#41352,
#41353),(#41354,#41355),(#41356,#41357),(#41358,#41359),(#41360,#41361),
(#41362,#41363),(#41364,#41365),(#41366,#41367),(#41368,#41369),(#41370,
#41371),(#41372,#41373),(#41374,#41375),(#41376,#41377),(#41378,#41379),
(#41380,#41381),(#41382,#41383),(#41384,#41385),(#41386,#41387),(#41388,
#41389),(#41390,#41391),(#41392,#41393),(#41394,#41395),(#41396,#41397),
(#41398,#41399),(#41400,#41401),(#41402,#41403),(#41404,#41405),(#41406,
#41407),(#41408,#41409),(#41410,#41411),(#41412,#41413),(#41414,#41415),
(#41416,#41417),(#41418,#41419),(#41420,#41421),(#41422,#41423),(#41424,
#41425),(#41426,#41427),(#41428,#41429),(#41430,#41431),(#41432,#41433),
(#41434,#41435),(#41436,#41437),(#41438,#41439),(#41440,#41441),(#41442,
#41443),(#41444,#41445),(#41446,#41447),(#41448,#41449)),.UNSPECIFIED.,
 .F.,.F.,.F.)
B_SPLINE_SURFACE_WITH_KNOTS((6,1,1,1,1,1,1,1,1,1,1,1,1,1,1,1,1,1,1,1,1,
1,1,1,1,1,1,1,1,1,1,1,1,1,1,1,1,1,1,1,1,1,1,1,1,1,1,1,1,1,1,1,1,1,1,1,1,
1,1,1,1,1,1,1,1,6),(2,2),(-1.,-0.984615384615383,-0.969230769230768,-0.953846153846152,
-0.938461538461537,-0.923076923076922,-0.907692307692306,-0.892307692307691,
-0.876923076923076,-0.86153846153846,-0.846153846153845,-0.83076923076923,
-0.815384615384614,-0.799999999999999,-0.784615384615384,-0.769230769230768,
-0.753846153846153,-0.738461538461538,-0.723076923076922,-0.707692307692307,
-0.692307692307692,-0.676923076923076,-0.661538461538461,-0.646153846153846,
-0.63076923076923,-0.615384615384615,-0.6,-0.584615384615384,-0.569230769230769,
-0.553846153846154,-0.538461538461538,-0.523076923076923,-0.507692307692308,
-0.492307692307692,-0.476923076923077,-0.461538461538462,-0.446153846153846,
-0.430769230769231,-0.415384615384615,-0.4,-0.384615384615385,-0.369230769230769,
-0.353846153846154,-0.338461538461538,-0.323076923076923,-0.307692307692308,
-0.292307692307692,-0.276923076923077,-0.261538461538462,-0.246153846153846,
-0.230769230769231,-0.215384615384615,-0.2,-0.184615384615385,-0.169230769230769,
-0.153846153846154,-0.138461538461538,-0.123076923076923,-0.107692307692308,
-0.0923076923076923,-0.0769230769230769,-0.0615384615384615,-0.0461538461538462,
-0.0307692307692308,-0.0153846153846154,0.),(-1.,1.),.UNSPECIFIED.)
GEOMETRIC_REPRESENTATION_ITEM()
RATIONAL_B_SPLINE_SURFACE(((1.,1.),(1.,1.),(1.,1.),(1.,1.),(1.,1.),(1.,
1.),(1.,1.),(1.,1.),(1.,1.),(1.,1.),(1.,1.),(1.,1.),(1.,1.),(1.,1.),(1.,
1.),(1.,1.),(1.,1.),(1.,1.),(1.,1.),(1.,1.),(1.,1.),(1.,1.),(1.,1.),(1.,
1.),(1.,1.),(1.,1.),(1.,1.),(1.,1.),(1.,1.),(1.,1.),(1.,1.),(1.,1.),(1.,
1.),(1.,1.),(1.,1.),(1.,1.),(1.,1.),(1.,1.),(1.,1.),(1.,1.),(1.,1.),(1.,
1.),(1.,1.),(1.,1.),(1.,1.),(1.,1.),(1.,1.),(1.,1.),(1.,1.),(1.,1.),(1.,
1.),(1.,1.),(1.,1.),(1.,1.),(1.,1.),(1.,1.),(1.,1.),(1.,1.),(1.,1.),(1.,
1.),(1.,1.),(1.,1.),(1.,1.),(1.,1.),(1.,1.),(1.,1.),(1.,1.),(1.,1.),(1.,
1.),(1.,1.)))
REPRESENTATION_ITEM('')
SURFACE()
);
#76=(
BOUNDED_SURFACE()
B_SPLINE_SURFACE(5,1,((#41522,#41523),(#41524,#41525),(#41526,#41527),(#41528,
#41529),(#41530,#41531),(#41532,#41533),(#41534,#41535),(#41536,#41537),
(#41538,#41539),(#41540,#41541),(#41542,#41543),(#41544,#41545),(#41546,
#41547),(#41548,#41549),(#41550,#41551),(#41552,#41553),(#41554,#41555),
(#41556,#41557),(#41558,#41559),(#41560,#41561),(#41562,#41563),(#41564,
#41565),(#41566,#41567),(#41568,#41569),(#41570,#41571),(#41572,#41573),
(#41574,#41575),(#41576,#41577),(#41578,#41579),(#41580,#41581),(#41582,
#41583),(#41584,#41585),(#41586,#41587),(#41588,#41589),(#41590,#41591),
(#41592,#41593),(#41594,#41595),(#41596,#41597),(#41598,#41599),(#41600,
#41601),(#41602,#41603),(#41604,#41605),(#41606,#41607),(#41608,#41609),
(#41610,#41611),(#41612,#41613),(#41614,#41615),(#41616,#41617),(#41618,
#41619),(#41620,#41621),(#41622,#41623),(#41624,#41625),(#41626,#41627),
(#41628,#41629),(#41630,#41631),(#41632,#41633),(#41634,#41635),(#41636,
#41637),(#41638,#41639),(#41640,#41641),(#41642,#41643),(#41644,#41645),
(#41646,#41647),(#41648,#41649),(#41650,#41651),(#41652,#41653),(#41654,
#41655),(#41656,#41657),(#41658,#41659),(#41660,#41661)),.UNSPECIFIED.,
 .F.,.F.,.F.)
B_SPLINE_SURFACE_WITH_KNOTS((6,1,1,1,1,1,1,1,1,1,1,1,1,1,1,1,1,1,1,1,1,
1,1,1,1,1,1,1,1,1,1,1,1,1,1,1,1,1,1,1,1,1,1,1,1,1,1,1,1,1,1,1,1,1,1,1,1,
1,1,1,1,1,1,1,1,6),(2,2),(-1.,-0.984615384615383,-0.969230769230768,-0.953846153846152,
-0.938461538461537,-0.923076923076922,-0.907692307692306,-0.892307692307691,
-0.876923076923076,-0.86153846153846,-0.846153846153845,-0.83076923076923,
-0.815384615384614,-0.799999999999999,-0.784615384615384,-0.769230769230768,
-0.753846153846153,-0.738461538461538,-0.723076923076922,-0.707692307692307,
-0.692307692307692,-0.676923076923076,-0.661538461538461,-0.646153846153846,
-0.63076923076923,-0.615384615384615,-0.6,-0.584615384615384,-0.569230769230769,
-0.553846153846154,-0.538461538461538,-0.523076923076923,-0.507692307692308,
-0.492307692307692,-0.476923076923077,-0.461538461538462,-0.446153846153846,
-0.430769230769231,-0.415384615384615,-0.4,-0.384615384615385,-0.369230769230769,
-0.353846153846154,-0.338461538461538,-0.323076923076923,-0.307692307692308,
-0.292307692307692,-0.276923076923077,-0.261538461538462,-0.246153846153846,
-0.230769230769231,-0.215384615384615,-0.2,-0.184615384615385,-0.169230769230769,
-0.153846153846154,-0.138461538461538,-0.123076923076923,-0.107692307692308,
-0.0923076923076923,-0.0769230769230769,-0.0615384615384615,-0.0461538461538462,
-0.0307692307692308,-0.0153846153846154,0.),(-1.,1.),.UNSPECIFIED.)
GEOMETRIC_REPRESENTATION_ITEM()
RATIONAL_B_SPLINE_SURFACE(((1.,1.),(1.,1.),(1.,1.),(1.,1.),(1.,1.),(1.,
1.),(1.,1.),(1.,1.),(1.,1.),(1.,1.),(1.,1.),(1.,1.),(1.,1.),(1.,1.),(1.,
1.),(1.,1.),(1.,1.),(1.,1.),(1.,1.),(1.,1.),(1.,1.),(1.,1.),(1.,1.),(1.,
1.),(1.,1.),(1.,1.),(1.,1.),(1.,1.),(1.,1.),(1.,1.),(1.,1.),(1.,1.),(1.,
1.),(1.,1.),(1.,1.),(1.,1.),(1.,1.),(1.,1.),(1.,1.),(1.,1.),(1.,1.),(1.,
1.),(1.,1.),(1.,1.),(1.,1.),(1.,1.),(1.,1.),(1.,1.),(1.,1.),(1.,1.),(1.,
1.),(1.,1.),(1.,1.),(1.,1.),(1.,1.),(1.,1.),(1.,1.),(1.,1.),(1.,1.),(1.,
1.),(1.,1.),(1.,1.),(1.,1.),(1.,1.),(1.,1.),(1.,1.),(1.,1.),(1.,1.),(1.,
1.),(1.,1.)))
REPRESENTATION_ITEM('')
SURFACE()
);
#77=(
BOUNDED_SURFACE()
B_SPLINE_SURFACE(5,1,((#41752,#41753),(#41754,#41755),(#41756,#41757),(#41758,
#41759),(#41760,#41761),(#41762,#41763),(#41764,#41765),(#41766,#41767),
(#41768,#41769),(#41770,#41771),(#41772,#41773),(#41774,#41775),(#41776,
#41777),(#41778,#41779),(#41780,#41781),(#41782,#41783),(#41784,#41785),
(#41786,#41787),(#41788,#41789),(#41790,#41791),(#41792,#41793),(#41794,
#41795),(#41796,#41797),(#41798,#41799),(#41800,#41801),(#41802,#41803),
(#41804,#41805),(#41806,#41807),(#41808,#41809),(#41810,#41811),(#41812,
#41813),(#41814,#41815),(#41816,#41817),(#41818,#41819),(#41820,#41821),
(#41822,#41823),(#41824,#41825),(#41826,#41827),(#41828,#41829),(#41830,
#41831),(#41832,#41833),(#41834,#41835),(#41836,#41837),(#41838,#41839),
(#41840,#41841),(#41842,#41843),(#41844,#41845),(#41846,#41847),(#41848,
#41849),(#41850,#41851),(#41852,#41853),(#41854,#41855),(#41856,#41857),
(#41858,#41859),(#41860,#41861),(#41862,#41863),(#41864,#41865),(#41866,
#41867),(#41868,#41869),(#41870,#41871),(#41872,#41873),(#41874,#41875),
(#41876,#41877),(#41878,#41879),(#41880,#41881),(#41882,#41883),(#41884,
#41885),(#41886,#41887),(#41888,#41889),(#41890,#41891)),.UNSPECIFIED.,
 .F.,.F.,.F.)
B_SPLINE_SURFACE_WITH_KNOTS((6,1,1,1,1,1,1,1,1,1,1,1,1,1,1,1,1,1,1,1,1,
1,1,1,1,1,1,1,1,1,1,1,1,1,1,1,1,1,1,1,1,1,1,1,1,1,1,1,1,1,1,1,1,1,1,1,1,
1,1,1,1,1,1,1,1,6),(2,2),(-1.,-0.984615384615383,-0.969230769230768,-0.953846153846152,
-0.938461538461537,-0.923076923076922,-0.907692307692306,-0.892307692307691,
-0.876923076923076,-0.86153846153846,-0.846153846153845,-0.83076923076923,
-0.815384615384614,-0.799999999999999,-0.784615384615384,-0.769230769230768,
-0.753846153846153,-0.738461538461538,-0.723076923076922,-0.707692307692307,
-0.692307692307692,-0.676923076923076,-0.661538461538461,-0.646153846153846,
-0.63076923076923,-0.615384615384615,-0.6,-0.584615384615384,-0.569230769230769,
-0.553846153846154,-0.538461538461538,-0.523076923076923,-0.507692307692308,
-0.492307692307692,-0.476923076923077,-0.461538461538462,-0.446153846153846,
-0.430769230769231,-0.415384615384615,-0.4,-0.384615384615385,-0.369230769230769,
-0.353846153846154,-0.338461538461538,-0.323076923076923,-0.307692307692308,
-0.292307692307692,-0.276923076923077,-0.261538461538462,-0.246153846153846,
-0.230769230769231,-0.215384615384615,-0.2,-0.184615384615385,-0.169230769230769,
-0.153846153846154,-0.138461538461538,-0.123076923076923,-0.107692307692308,
-0.0923076923076923,-0.0769230769230769,-0.0615384615384615,-0.0461538461538462,
-0.0307692307692308,-0.0153846153846154,0.),(-1.,1.),.UNSPECIFIED.)
GEOMETRIC_REPRESENTATION_ITEM()
RATIONAL_B_SPLINE_SURFACE(((1.,1.),(1.,1.),(1.,1.),(1.,1.),(1.,1.),(1.,
1.),(1.,1.),(1.,1.),(1.,1.),(1.,1.),(1.,1.),(1.,1.),(1.,1.),(1.,1.),(1.,
1.),(1.,1.),(1.,1.),(1.,1.),(1.,1.),(1.,1.),(1.,1.),(1.,1.),(1.,1.),(1.,
1.),(1.,1.),(1.,1.),(1.,1.),(1.,1.),(1.,1.),(1.,1.),(1.,1.),(1.,1.),(1.,
1.),(1.,1.),(1.,1.),(1.,1.),(1.,1.),(1.,1.),(1.,1.),(1.,1.),(1.,1.),(1.,
1.),(1.,1.),(1.,1.),(1.,1.),(1.,1.),(1.,1.),(1.,1.),(1.,1.),(1.,1.),(1.,
1.),(1.,1.),(1.,1.),(1.,1.),(1.,1.),(1.,1.),(1.,1.),(1.,1.),(1.,1.),(1.,
1.),(1.,1.),(1.,1.),(1.,1.),(1.,1.),(1.,1.),(1.,1.),(1.,1.),(1.,1.),(1.,
1.),(1.,1.)))
REPRESENTATION_ITEM('')
SURFACE()
);
#78=(
BOUNDED_SURFACE()
B_SPLINE_SURFACE(5,1,((#41964,#41965),(#41966,#41967),(#41968,#41969),(#41970,
#41971),(#41972,#41973),(#41974,#41975),(#41976,#41977),(#41978,#41979),
(#41980,#41981),(#41982,#41983),(#41984,#41985),(#41986,#41987),(#41988,
#41989),(#41990,#41991),(#41992,#41993),(#41994,#41995),(#41996,#41997),
(#41998,#41999),(#42000,#42001),(#42002,#42003),(#42004,#42005),(#42006,
#42007),(#42008,#42009),(#42010,#42011),(#42012,#42013),(#42014,#42015),
(#42016,#42017),(#42018,#42019),(#42020,#42021),(#42022,#42023),(#42024,
#42025),(#42026,#42027),(#42028,#42029),(#42030,#42031),(#42032,#42033),
(#42034,#42035),(#42036,#42037),(#42038,#42039),(#42040,#42041),(#42042,
#42043),(#42044,#42045),(#42046,#42047),(#42048,#42049),(#42050,#42051),
(#42052,#42053),(#42054,#42055),(#42056,#42057),(#42058,#42059),(#42060,
#42061),(#42062,#42063),(#42064,#42065),(#42066,#42067),(#42068,#42069),
(#42070,#42071),(#42072,#42073),(#42074,#42075),(#42076,#42077),(#42078,
#42079),(#42080,#42081),(#42082,#42083),(#42084,#42085),(#42086,#42087),
(#42088,#42089),(#42090,#42091),(#42092,#42093),(#42094,#42095),(#42096,
#42097),(#42098,#42099),(#42100,#42101),(#42102,#42103)),.UNSPECIFIED.,
 .F.,.F.,.F.)
B_SPLINE_SURFACE_WITH_KNOTS((6,1,1,1,1,1,1,1,1,1,1,1,1,1,1,1,1,1,1,1,1,
1,1,1,1,1,1,1,1,1,1,1,1,1,1,1,1,1,1,1,1,1,1,1,1,1,1,1,1,1,1,1,1,1,1,1,1,
1,1,1,1,1,1,1,1,6),(2,2),(-1.,-0.984615384615383,-0.969230769230768,-0.953846153846152,
-0.938461538461537,-0.923076923076922,-0.907692307692306,-0.892307692307691,
-0.876923076923076,-0.86153846153846,-0.846153846153845,-0.83076923076923,
-0.815384615384614,-0.799999999999999,-0.784615384615384,-0.769230769230768,
-0.753846153846153,-0.738461538461538,-0.723076923076922,-0.707692307692307,
-0.692307692307692,-0.676923076923076,-0.661538461538461,-0.646153846153846,
-0.63076923076923,-0.615384615384615,-0.6,-0.584615384615384,-0.569230769230769,
-0.553846153846154,-0.538461538461538,-0.523076923076923,-0.507692307692308,
-0.492307692307692,-0.476923076923077,-0.461538461538462,-0.446153846153846,
-0.430769230769231,-0.415384615384615,-0.4,-0.384615384615385,-0.369230769230769,
-0.353846153846154,-0.338461538461538,-0.323076923076923,-0.307692307692308,
-0.292307692307692,-0.276923076923077,-0.261538461538462,-0.246153846153846,
-0.230769230769231,-0.215384615384615,-0.2,-0.184615384615385,-0.169230769230769,
-0.153846153846154,-0.138461538461538,-0.123076923076923,-0.107692307692308,
-0.0923076923076923,-0.0769230769230769,-0.0615384615384615,-0.0461538461538462,
-0.0307692307692308,-0.0153846153846154,0.),(-1.,1.),.UNSPECIFIED.)
GEOMETRIC_REPRESENTATION_ITEM()
RATIONAL_B_SPLINE_SURFACE(((1.,1.),(1.,1.),(1.,1.),(1.,1.),(1.,1.),(1.,
1.),(1.,1.),(1.,1.),(1.,1.),(1.,1.),(1.,1.),(1.,1.),(1.,1.),(1.,1.),(1.,
1.),(1.,1.),(1.,1.),(1.,1.),(1.,1.),(1.,1.),(1.,1.),(1.,1.),(1.,1.),(1.,
1.),(1.,1.),(1.,1.),(1.,1.),(1.,1.),(1.,1.),(1.,1.),(1.,1.),(1.,1.),(1.,
1.),(1.,1.),(1.,1.),(1.,1.),(1.,1.),(1.,1.),(1.,1.),(1.,1.),(1.,1.),(1.,
1.),(1.,1.),(1.,1.),(1.,1.),(1.,1.),(1.,1.),(1.,1.),(1.,1.),(1.,1.),(1.,
1.),(1.,1.),(1.,1.),(1.,1.),(1.,1.),(1.,1.),(1.,1.),(1.,1.),(1.,1.),(1.,
1.),(1.,1.),(1.,1.),(1.,1.),(1.,1.),(1.,1.),(1.,1.),(1.,1.),(1.,1.),(1.,
1.),(1.,1.)))
REPRESENTATION_ITEM('')
SURFACE()
);
#79=(
BOUNDED_SURFACE()
B_SPLINE_SURFACE(5,1,((#42194,#42195),(#42196,#42197),(#42198,#42199),(#42200,
#42201),(#42202,#42203),(#42204,#42205),(#42206,#42207),(#42208,#42209),
(#42210,#42211),(#42212,#42213),(#42214,#42215),(#42216,#42217),(#42218,
#42219),(#42220,#42221),(#42222,#42223),(#42224,#42225),(#42226,#42227),
(#42228,#42229),(#42230,#42231),(#42232,#42233),(#42234,#42235),(#42236,
#42237),(#42238,#42239),(#42240,#42241),(#42242,#42243),(#42244,#42245),
(#42246,#42247),(#42248,#42249),(#42250,#42251),(#42252,#42253),(#42254,
#42255),(#42256,#42257),(#42258,#42259),(#42260,#42261),(#42262,#42263),
(#42264,#42265),(#42266,#42267),(#42268,#42269),(#42270,#42271),(#42272,
#42273),(#42274,#42275),(#42276,#42277),(#42278,#42279),(#42280,#42281),
(#42282,#42283),(#42284,#42285),(#42286,#42287),(#42288,#42289),(#42290,
#42291),(#42292,#42293),(#42294,#42295),(#42296,#42297),(#42298,#42299),
(#42300,#42301),(#42302,#42303),(#42304,#42305),(#42306,#42307),(#42308,
#42309),(#42310,#42311),(#42312,#42313),(#42314,#42315),(#42316,#42317),
(#42318,#42319),(#42320,#42321),(#42322,#42323),(#42324,#42325),(#42326,
#42327),(#42328,#42329),(#42330,#42331),(#42332,#42333)),.UNSPECIFIED.,
 .F.,.F.,.F.)
B_SPLINE_SURFACE_WITH_KNOTS((6,1,1,1,1,1,1,1,1,1,1,1,1,1,1,1,1,1,1,1,1,
1,1,1,1,1,1,1,1,1,1,1,1,1,1,1,1,1,1,1,1,1,1,1,1,1,1,1,1,1,1,1,1,1,1,1,1,
1,1,1,1,1,1,1,1,6),(2,2),(-1.,-0.984615384615383,-0.969230769230768,-0.953846153846152,
-0.938461538461537,-0.923076923076922,-0.907692307692306,-0.892307692307691,
-0.876923076923076,-0.86153846153846,-0.846153846153845,-0.83076923076923,
-0.815384615384614,-0.799999999999999,-0.784615384615384,-0.769230769230768,
-0.753846153846153,-0.738461538461538,-0.723076923076922,-0.707692307692307,
-0.692307692307692,-0.676923076923076,-0.661538461538461,-0.646153846153846,
-0.63076923076923,-0.615384615384615,-0.6,-0.584615384615384,-0.569230769230769,
-0.553846153846154,-0.538461538461538,-0.523076923076923,-0.507692307692308,
-0.492307692307692,-0.476923076923077,-0.461538461538462,-0.446153846153846,
-0.430769230769231,-0.415384615384615,-0.4,-0.384615384615385,-0.369230769230769,
-0.353846153846154,-0.338461538461538,-0.323076923076923,-0.307692307692308,
-0.292307692307692,-0.276923076923077,-0.261538461538462,-0.246153846153846,
-0.230769230769231,-0.215384615384615,-0.2,-0.184615384615385,-0.169230769230769,
-0.153846153846154,-0.138461538461538,-0.123076923076923,-0.107692307692308,
-0.0923076923076923,-0.0769230769230769,-0.0615384615384615,-0.0461538461538462,
-0.0307692307692308,-0.0153846153846154,0.),(-1.,1.),.UNSPECIFIED.)
GEOMETRIC_REPRESENTATION_ITEM()
RATIONAL_B_SPLINE_SURFACE(((1.,1.),(1.,1.),(1.,1.),(1.,1.),(1.,1.),(1.,
1.),(1.,1.),(1.,1.),(1.,1.),(1.,1.),(1.,1.),(1.,1.),(1.,1.),(1.,1.),(1.,
1.),(1.,1.),(1.,1.),(1.,1.),(1.,1.),(1.,1.),(1.,1.),(1.,1.),(1.,1.),(1.,
1.),(1.,1.),(1.,1.),(1.,1.),(1.,1.),(1.,1.),(1.,1.),(1.,1.),(1.,1.),(1.,
1.),(1.,1.),(1.,1.),(1.,1.),(1.,1.),(1.,1.),(1.,1.),(1.,1.),(1.,1.),(1.,
1.),(1.,1.),(1.,1.),(1.,1.),(1.,1.),(1.,1.),(1.,1.),(1.,1.),(1.,1.),(1.,
1.),(1.,1.),(1.,1.),(1.,1.),(1.,1.),(1.,1.),(1.,1.),(1.,1.),(1.,1.),(1.,
1.),(1.,1.),(1.,1.),(1.,1.),(1.,1.),(1.,1.),(1.,1.),(1.,1.),(1.,1.),(1.,
1.),(1.,1.)))
REPRESENTATION_ITEM('')
SURFACE()
);
#80=(
BOUNDED_SURFACE()
B_SPLINE_SURFACE(5,1,((#42406,#42407),(#42408,#42409),(#42410,#42411),(#42412,
#42413),(#42414,#42415),(#42416,#42417),(#42418,#42419),(#42420,#42421),
(#42422,#42423),(#42424,#42425),(#42426,#42427),(#42428,#42429),(#42430,
#42431),(#42432,#42433),(#42434,#42435),(#42436,#42437),(#42438,#42439),
(#42440,#42441),(#42442,#42443),(#42444,#42445),(#42446,#42447),(#42448,
#42449),(#42450,#42451),(#42452,#42453),(#42454,#42455),(#42456,#42457),
(#42458,#42459),(#42460,#42461),(#42462,#42463),(#42464,#42465),(#42466,
#42467),(#42468,#42469),(#42470,#42471),(#42472,#42473),(#42474,#42475),
(#42476,#42477),(#42478,#42479),(#42480,#42481),(#42482,#42483),(#42484,
#42485),(#42486,#42487),(#42488,#42489),(#42490,#42491),(#42492,#42493),
(#42494,#42495),(#42496,#42497),(#42498,#42499),(#42500,#42501),(#42502,
#42503),(#42504,#42505),(#42506,#42507),(#42508,#42509),(#42510,#42511),
(#42512,#42513),(#42514,#42515),(#42516,#42517),(#42518,#42519),(#42520,
#42521),(#42522,#42523),(#42524,#42525),(#42526,#42527),(#42528,#42529),
(#42530,#42531),(#42532,#42533),(#42534,#42535),(#42536,#42537),(#42538,
#42539),(#42540,#42541),(#42542,#42543),(#42544,#42545)),.UNSPECIFIED.,
 .F.,.F.,.F.)
B_SPLINE_SURFACE_WITH_KNOTS((6,1,1,1,1,1,1,1,1,1,1,1,1,1,1,1,1,1,1,1,1,
1,1,1,1,1,1,1,1,1,1,1,1,1,1,1,1,1,1,1,1,1,1,1,1,1,1,1,1,1,1,1,1,1,1,1,1,
1,1,1,1,1,1,1,1,6),(2,2),(-1.,-0.984615384615383,-0.969230769230768,-0.953846153846152,
-0.938461538461537,-0.923076923076922,-0.907692307692306,-0.892307692307691,
-0.876923076923076,-0.86153846153846,-0.846153846153845,-0.83076923076923,
-0.815384615384614,-0.799999999999999,-0.784615384615384,-0.769230769230768,
-0.753846153846153,-0.738461538461538,-0.723076923076922,-0.707692307692307,
-0.692307692307692,-0.676923076923076,-0.661538461538461,-0.646153846153846,
-0.63076923076923,-0.615384615384615,-0.6,-0.584615384615384,-0.569230769230769,
-0.553846153846154,-0.538461538461538,-0.523076923076923,-0.507692307692308,
-0.492307692307692,-0.476923076923077,-0.461538461538462,-0.446153846153846,
-0.430769230769231,-0.415384615384615,-0.4,-0.384615384615385,-0.369230769230769,
-0.353846153846154,-0.338461538461538,-0.323076923076923,-0.307692307692308,
-0.292307692307692,-0.276923076923077,-0.261538461538462,-0.246153846153846,
-0.230769230769231,-0.215384615384615,-0.2,-0.184615384615385,-0.169230769230769,
-0.153846153846154,-0.138461538461538,-0.123076923076923,-0.107692307692308,
-0.0923076923076923,-0.0769230769230769,-0.0615384615384615,-0.0461538461538462,
-0.0307692307692308,-0.0153846153846154,0.),(-1.,1.),.UNSPECIFIED.)
GEOMETRIC_REPRESENTATION_ITEM()
RATIONAL_B_SPLINE_SURFACE(((1.,1.),(1.,1.),(1.,1.),(1.,1.),(1.,1.),(1.,
1.),(1.,1.),(1.,1.),(1.,1.),(1.,1.),(1.,1.),(1.,1.),(1.,1.),(1.,1.),(1.,
1.),(1.,1.),(1.,1.),(1.,1.),(1.,1.),(1.,1.),(1.,1.),(1.,1.),(1.,1.),(1.,
1.),(1.,1.),(1.,1.),(1.,1.),(1.,1.),(1.,1.),(1.,1.),(1.,1.),(1.,1.),(1.,
1.),(1.,1.),(1.,1.),(1.,1.),(1.,1.),(1.,1.),(1.,1.),(1.,1.),(1.,1.),(1.,
1.),(1.,1.),(1.,1.),(1.,1.),(1.,1.),(1.,1.),(1.,1.),(1.,1.),(1.,1.),(1.,
1.),(1.,1.),(1.,1.),(1.,1.),(1.,1.),(1.,1.),(1.,1.),(1.,1.),(1.,1.),(1.,
1.),(1.,1.),(1.,1.),(1.,1.),(1.,1.),(1.,1.),(1.,1.),(1.,1.),(1.,1.),(1.,
1.),(1.,1.)))
REPRESENTATION_ITEM('')
SURFACE()
);
#81=(
BOUNDED_SURFACE()
B_SPLINE_SURFACE(5,1,((#42636,#42637),(#42638,#42639),(#42640,#42641),(#42642,
#42643),(#42644,#42645),(#42646,#42647),(#42648,#42649),(#42650,#42651),
(#42652,#42653),(#42654,#42655),(#42656,#42657),(#42658,#42659),(#42660,
#42661),(#42662,#42663),(#42664,#42665),(#42666,#42667),(#42668,#42669),
(#42670,#42671),(#42672,#42673),(#42674,#42675),(#42676,#42677),(#42678,
#42679),(#42680,#42681),(#42682,#42683),(#42684,#42685),(#42686,#42687),
(#42688,#42689),(#42690,#42691),(#42692,#42693),(#42694,#42695),(#42696,
#42697),(#42698,#42699),(#42700,#42701),(#42702,#42703),(#42704,#42705),
(#42706,#42707),(#42708,#42709),(#42710,#42711),(#42712,#42713),(#42714,
#42715),(#42716,#42717),(#42718,#42719),(#42720,#42721),(#42722,#42723),
(#42724,#42725),(#42726,#42727),(#42728,#42729),(#42730,#42731),(#42732,
#42733),(#42734,#42735),(#42736,#42737),(#42738,#42739),(#42740,#42741),
(#42742,#42743),(#42744,#42745),(#42746,#42747),(#42748,#42749),(#42750,
#42751),(#42752,#42753),(#42754,#42755),(#42756,#42757),(#42758,#42759),
(#42760,#42761),(#42762,#42763),(#42764,#42765),(#42766,#42767),(#42768,
#42769),(#42770,#42771),(#42772,#42773),(#42774,#42775)),.UNSPECIFIED.,
 .F.,.F.,.F.)
B_SPLINE_SURFACE_WITH_KNOTS((6,1,1,1,1,1,1,1,1,1,1,1,1,1,1,1,1,1,1,1,1,
1,1,1,1,1,1,1,1,1,1,1,1,1,1,1,1,1,1,1,1,1,1,1,1,1,1,1,1,1,1,1,1,1,1,1,1,
1,1,1,1,1,1,1,1,6),(2,2),(-1.,-0.984615384615383,-0.969230769230768,-0.953846153846152,
-0.938461538461537,-0.923076923076922,-0.907692307692306,-0.892307692307691,
-0.876923076923076,-0.86153846153846,-0.846153846153845,-0.83076923076923,
-0.815384615384614,-0.799999999999999,-0.784615384615384,-0.769230769230768,
-0.753846153846153,-0.738461538461538,-0.723076923076922,-0.707692307692307,
-0.692307692307692,-0.676923076923076,-0.661538461538461,-0.646153846153846,
-0.63076923076923,-0.615384615384615,-0.6,-0.584615384615384,-0.569230769230769,
-0.553846153846154,-0.538461538461538,-0.523076923076923,-0.507692307692308,
-0.492307692307692,-0.476923076923077,-0.461538461538462,-0.446153846153846,
-0.430769230769231,-0.415384615384615,-0.4,-0.384615384615385,-0.369230769230769,
-0.353846153846154,-0.338461538461538,-0.323076923076923,-0.307692307692308,
-0.292307692307692,-0.276923076923077,-0.261538461538462,-0.246153846153846,
-0.230769230769231,-0.215384615384615,-0.2,-0.184615384615385,-0.169230769230769,
-0.153846153846154,-0.138461538461538,-0.123076923076923,-0.107692307692308,
-0.0923076923076923,-0.0769230769230769,-0.0615384615384615,-0.0461538461538462,
-0.0307692307692308,-0.0153846153846154,0.),(-1.,1.),.UNSPECIFIED.)
GEOMETRIC_REPRESENTATION_ITEM()
RATIONAL_B_SPLINE_SURFACE(((1.,1.),(1.,1.),(1.,1.),(1.,1.),(1.,1.),(1.,
1.),(1.,1.),(1.,1.),(1.,1.),(1.,1.),(1.,1.),(1.,1.),(1.,1.),(1.,1.),(1.,
1.),(1.,1.),(1.,1.),(1.,1.),(1.,1.),(1.,1.),(1.,1.),(1.,1.),(1.,1.),(1.,
1.),(1.,1.),(1.,1.),(1.,1.),(1.,1.),(1.,1.),(1.,1.),(1.,1.),(1.,1.),(1.,
1.),(1.,1.),(1.,1.),(1.,1.),(1.,1.),(1.,1.),(1.,1.),(1.,1.),(1.,1.),(1.,
1.),(1.,1.),(1.,1.),(1.,1.),(1.,1.),(1.,1.),(1.,1.),(1.,1.),(1.,1.),(1.,
1.),(1.,1.),(1.,1.),(1.,1.),(1.,1.),(1.,1.),(1.,1.),(1.,1.),(1.,1.),(1.,
1.),(1.,1.),(1.,1.),(1.,1.),(1.,1.),(1.,1.),(1.,1.),(1.,1.),(1.,1.),(1.,
1.),(1.,1.)))
REPRESENTATION_ITEM('')
SURFACE()
);
#82=(
BOUNDED_SURFACE()
B_SPLINE_SURFACE(5,1,((#42848,#42849),(#42850,#42851),(#42852,#42853),(#42854,
#42855),(#42856,#42857),(#42858,#42859),(#42860,#42861),(#42862,#42863),
(#42864,#42865),(#42866,#42867),(#42868,#42869),(#42870,#42871),(#42872,
#42873),(#42874,#42875),(#42876,#42877),(#42878,#42879),(#42880,#42881),
(#42882,#42883),(#42884,#42885),(#42886,#42887),(#42888,#42889),(#42890,
#42891),(#42892,#42893),(#42894,#42895),(#42896,#42897),(#42898,#42899),
(#42900,#42901),(#42902,#42903),(#42904,#42905),(#42906,#42907),(#42908,
#42909),(#42910,#42911),(#42912,#42913),(#42914,#42915),(#42916,#42917),
(#42918,#42919),(#42920,#42921),(#42922,#42923),(#42924,#42925),(#42926,
#42927),(#42928,#42929),(#42930,#42931),(#42932,#42933),(#42934,#42935),
(#42936,#42937),(#42938,#42939),(#42940,#42941),(#42942,#42943),(#42944,
#42945),(#42946,#42947),(#42948,#42949),(#42950,#42951),(#42952,#42953),
(#42954,#42955),(#42956,#42957),(#42958,#42959),(#42960,#42961),(#42962,
#42963),(#42964,#42965),(#42966,#42967),(#42968,#42969),(#42970,#42971),
(#42972,#42973),(#42974,#42975),(#42976,#42977),(#42978,#42979),(#42980,
#42981),(#42982,#42983),(#42984,#42985),(#42986,#42987)),.UNSPECIFIED.,
 .F.,.F.,.F.)
B_SPLINE_SURFACE_WITH_KNOTS((6,1,1,1,1,1,1,1,1,1,1,1,1,1,1,1,1,1,1,1,1,
1,1,1,1,1,1,1,1,1,1,1,1,1,1,1,1,1,1,1,1,1,1,1,1,1,1,1,1,1,1,1,1,1,1,1,1,
1,1,1,1,1,1,1,1,6),(2,2),(-1.,-0.984615384615383,-0.969230769230768,-0.953846153846152,
-0.938461538461537,-0.923076923076922,-0.907692307692306,-0.892307692307691,
-0.876923076923076,-0.86153846153846,-0.846153846153845,-0.83076923076923,
-0.815384615384614,-0.799999999999999,-0.784615384615384,-0.769230769230768,
-0.753846153846153,-0.738461538461538,-0.723076923076922,-0.707692307692307,
-0.692307692307692,-0.676923076923076,-0.661538461538461,-0.646153846153846,
-0.63076923076923,-0.615384615384615,-0.6,-0.584615384615384,-0.569230769230769,
-0.553846153846154,-0.538461538461538,-0.523076923076923,-0.507692307692308,
-0.492307692307692,-0.476923076923077,-0.461538461538462,-0.446153846153846,
-0.430769230769231,-0.415384615384615,-0.4,-0.384615384615385,-0.369230769230769,
-0.353846153846154,-0.338461538461538,-0.323076923076923,-0.307692307692308,
-0.292307692307692,-0.276923076923077,-0.261538461538462,-0.246153846153846,
-0.230769230769231,-0.215384615384615,-0.2,-0.184615384615385,-0.169230769230769,
-0.153846153846154,-0.138461538461538,-0.123076923076923,-0.107692307692308,
-0.0923076923076923,-0.0769230769230769,-0.0615384615384615,-0.0461538461538462,
-0.0307692307692308,-0.0153846153846154,0.),(-1.,1.),.UNSPECIFIED.)
GEOMETRIC_REPRESENTATION_ITEM()
RATIONAL_B_SPLINE_SURFACE(((1.,1.),(1.,1.),(1.,1.),(1.,1.),(1.,1.),(1.,
1.),(1.,1.),(1.,1.),(1.,1.),(1.,1.),(1.,1.),(1.,1.),(1.,1.),(1.,1.),(1.,
1.),(1.,1.),(1.,1.),(1.,1.),(1.,1.),(1.,1.),(1.,1.),(1.,1.),(1.,1.),(1.,
1.),(1.,1.),(1.,1.),(1.,1.),(1.,1.),(1.,1.),(1.,1.),(1.,1.),(1.,1.),(1.,
1.),(1.,1.),(1.,1.),(1.,1.),(1.,1.),(1.,1.),(1.,1.),(1.,1.),(1.,1.),(1.,
1.),(1.,1.),(1.,1.),(1.,1.),(1.,1.),(1.,1.),(1.,1.),(1.,1.),(1.,1.),(1.,
1.),(1.,1.),(1.,1.),(1.,1.),(1.,1.),(1.,1.),(1.,1.),(1.,1.),(1.,1.),(1.,
1.),(1.,1.),(1.,1.),(1.,1.),(1.,1.),(1.,1.),(1.,1.),(1.,1.),(1.,1.),(1.,
1.),(1.,1.)))
REPRESENTATION_ITEM('')
SURFACE()
);
#83=(
BOUNDED_SURFACE()
B_SPLINE_SURFACE(5,1,((#43078,#43079),(#43080,#43081),(#43082,#43083),(#43084,
#43085),(#43086,#43087),(#43088,#43089),(#43090,#43091),(#43092,#43093),
(#43094,#43095),(#43096,#43097),(#43098,#43099),(#43100,#43101),(#43102,
#43103),(#43104,#43105),(#43106,#43107),(#43108,#43109),(#43110,#43111),
(#43112,#43113),(#43114,#43115),(#43116,#43117),(#43118,#43119),(#43120,
#43121),(#43122,#43123),(#43124,#43125),(#43126,#43127),(#43128,#43129),
(#43130,#43131),(#43132,#43133),(#43134,#43135),(#43136,#43137),(#43138,
#43139),(#43140,#43141),(#43142,#43143),(#43144,#43145),(#43146,#43147),
(#43148,#43149),(#43150,#43151),(#43152,#43153),(#43154,#43155),(#43156,
#43157),(#43158,#43159),(#43160,#43161),(#43162,#43163),(#43164,#43165),
(#43166,#43167),(#43168,#43169),(#43170,#43171),(#43172,#43173),(#43174,
#43175),(#43176,#43177),(#43178,#43179),(#43180,#43181),(#43182,#43183),
(#43184,#43185),(#43186,#43187),(#43188,#43189),(#43190,#43191),(#43192,
#43193),(#43194,#43195),(#43196,#43197),(#43198,#43199),(#43200,#43201),
(#43202,#43203),(#43204,#43205),(#43206,#43207),(#43208,#43209),(#43210,
#43211),(#43212,#43213),(#43214,#43215),(#43216,#43217)),.UNSPECIFIED.,
 .F.,.F.,.F.)
B_SPLINE_SURFACE_WITH_KNOTS((6,1,1,1,1,1,1,1,1,1,1,1,1,1,1,1,1,1,1,1,1,
1,1,1,1,1,1,1,1,1,1,1,1,1,1,1,1,1,1,1,1,1,1,1,1,1,1,1,1,1,1,1,1,1,1,1,1,
1,1,1,1,1,1,1,1,6),(2,2),(-1.,-0.984615384615383,-0.969230769230768,-0.953846153846152,
-0.938461538461537,-0.923076923076922,-0.907692307692306,-0.892307692307691,
-0.876923076923076,-0.86153846153846,-0.846153846153845,-0.83076923076923,
-0.815384615384614,-0.799999999999999,-0.784615384615384,-0.769230769230768,
-0.753846153846153,-0.738461538461538,-0.723076923076922,-0.707692307692307,
-0.692307692307692,-0.676923076923076,-0.661538461538461,-0.646153846153846,
-0.63076923076923,-0.615384615384615,-0.6,-0.584615384615384,-0.569230769230769,
-0.553846153846154,-0.538461538461538,-0.523076923076923,-0.507692307692308,
-0.492307692307692,-0.476923076923077,-0.461538461538462,-0.446153846153846,
-0.430769230769231,-0.415384615384615,-0.4,-0.384615384615385,-0.369230769230769,
-0.353846153846154,-0.338461538461538,-0.323076923076923,-0.307692307692308,
-0.292307692307692,-0.276923076923077,-0.261538461538462,-0.246153846153846,
-0.230769230769231,-0.215384615384615,-0.2,-0.184615384615385,-0.169230769230769,
-0.153846153846154,-0.138461538461538,-0.123076923076923,-0.107692307692308,
-0.0923076923076923,-0.0769230769230769,-0.0615384615384615,-0.0461538461538462,
-0.0307692307692308,-0.0153846153846154,0.),(-1.,1.),.UNSPECIFIED.)
GEOMETRIC_REPRESENTATION_ITEM()
RATIONAL_B_SPLINE_SURFACE(((1.,1.),(1.,1.),(1.,1.),(1.,1.),(1.,1.),(1.,
1.),(1.,1.),(1.,1.),(1.,1.),(1.,1.),(1.,1.),(1.,1.),(1.,1.),(1.,1.),(1.,
1.),(1.,1.),(1.,1.),(1.,1.),(1.,1.),(1.,1.),(1.,1.),(1.,1.),(1.,1.),(1.,
1.),(1.,1.),(1.,1.),(1.,1.),(1.,1.),(1.,1.),(1.,1.),(1.,1.),(1.,1.),(1.,
1.),(1.,1.),(1.,1.),(1.,1.),(1.,1.),(1.,1.),(1.,1.),(1.,1.),(1.,1.),(1.,
1.),(1.,1.),(1.,1.),(1.,1.),(1.,1.),(1.,1.),(1.,1.),(1.,1.),(1.,1.),(1.,
1.),(1.,1.),(1.,1.),(1.,1.),(1.,1.),(1.,1.),(1.,1.),(1.,1.),(1.,1.),(1.,
1.),(1.,1.),(1.,1.),(1.,1.),(1.,1.),(1.,1.),(1.,1.),(1.,1.),(1.,1.),(1.,
1.),(1.,1.)))
REPRESENTATION_ITEM('')
SURFACE()
);
#84=(
BOUNDED_SURFACE()
B_SPLINE_SURFACE(5,1,((#43290,#43291),(#43292,#43293),(#43294,#43295),(#43296,
#43297),(#43298,#43299),(#43300,#43301),(#43302,#43303),(#43304,#43305),
(#43306,#43307),(#43308,#43309),(#43310,#43311),(#43312,#43313),(#43314,
#43315),(#43316,#43317),(#43318,#43319),(#43320,#43321),(#43322,#43323),
(#43324,#43325),(#43326,#43327),(#43328,#43329),(#43330,#43331),(#43332,
#43333),(#43334,#43335),(#43336,#43337),(#43338,#43339),(#43340,#43341),
(#43342,#43343),(#43344,#43345),(#43346,#43347),(#43348,#43349),(#43350,
#43351),(#43352,#43353),(#43354,#43355),(#43356,#43357),(#43358,#43359),
(#43360,#43361),(#43362,#43363),(#43364,#43365),(#43366,#43367),(#43368,
#43369),(#43370,#43371),(#43372,#43373),(#43374,#43375),(#43376,#43377),
(#43378,#43379),(#43380,#43381),(#43382,#43383),(#43384,#43385),(#43386,
#43387),(#43388,#43389),(#43390,#43391),(#43392,#43393),(#43394,#43395),
(#43396,#43397),(#43398,#43399),(#43400,#43401),(#43402,#43403),(#43404,
#43405),(#43406,#43407),(#43408,#43409),(#43410,#43411),(#43412,#43413),
(#43414,#43415),(#43416,#43417),(#43418,#43419),(#43420,#43421),(#43422,
#43423),(#43424,#43425),(#43426,#43427),(#43428,#43429)),.UNSPECIFIED.,
 .F.,.F.,.F.)
B_SPLINE_SURFACE_WITH_KNOTS((6,1,1,1,1,1,1,1,1,1,1,1,1,1,1,1,1,1,1,1,1,
1,1,1,1,1,1,1,1,1,1,1,1,1,1,1,1,1,1,1,1,1,1,1,1,1,1,1,1,1,1,1,1,1,1,1,1,
1,1,1,1,1,1,1,1,6),(2,2),(-1.,-0.984615384615383,-0.969230769230768,-0.953846153846152,
-0.938461538461537,-0.923076923076922,-0.907692307692306,-0.892307692307691,
-0.876923076923076,-0.86153846153846,-0.846153846153845,-0.83076923076923,
-0.815384615384614,-0.799999999999999,-0.784615384615384,-0.769230769230768,
-0.753846153846153,-0.738461538461538,-0.723076923076922,-0.707692307692307,
-0.692307692307692,-0.676923076923076,-0.661538461538461,-0.646153846153846,
-0.63076923076923,-0.615384615384615,-0.6,-0.584615384615384,-0.569230769230769,
-0.553846153846154,-0.538461538461538,-0.523076923076923,-0.507692307692308,
-0.492307692307692,-0.476923076923077,-0.461538461538462,-0.446153846153846,
-0.430769230769231,-0.415384615384615,-0.4,-0.384615384615385,-0.369230769230769,
-0.353846153846154,-0.338461538461538,-0.323076923076923,-0.307692307692308,
-0.292307692307692,-0.276923076923077,-0.261538461538462,-0.246153846153846,
-0.230769230769231,-0.215384615384615,-0.2,-0.184615384615385,-0.169230769230769,
-0.153846153846154,-0.138461538461538,-0.123076923076923,-0.107692307692308,
-0.0923076923076923,-0.0769230769230769,-0.0615384615384615,-0.0461538461538462,
-0.0307692307692308,-0.0153846153846154,0.),(-1.,1.),.UNSPECIFIED.)
GEOMETRIC_REPRESENTATION_ITEM()
RATIONAL_B_SPLINE_SURFACE(((1.,1.),(1.,1.),(1.,1.),(1.,1.),(1.,1.),(1.,
1.),(1.,1.),(1.,1.),(1.,1.),(1.,1.),(1.,1.),(1.,1.),(1.,1.),(1.,1.),(1.,
1.),(1.,1.),(1.,1.),(1.,1.),(1.,1.),(1.,1.),(1.,1.),(1.,1.),(1.,1.),(1.,
1.),(1.,1.),(1.,1.),(1.,1.),(1.,1.),(1.,1.),(1.,1.),(1.,1.),(1.,1.),(1.,
1.),(1.,1.),(1.,1.),(1.,1.),(1.,1.),(1.,1.),(1.,1.),(1.,1.),(1.,1.),(1.,
1.),(1.,1.),(1.,1.),(1.,1.),(1.,1.),(1.,1.),(1.,1.),(1.,1.),(1.,1.),(1.,
1.),(1.,1.),(1.,1.),(1.,1.),(1.,1.),(1.,1.),(1.,1.),(1.,1.),(1.,1.),(1.,
1.),(1.,1.),(1.,1.),(1.,1.),(1.,1.),(1.,1.),(1.,1.),(1.,1.),(1.,1.),(1.,
1.),(1.,1.)))
REPRESENTATION_ITEM('')
SURFACE()
);
#85=(
BOUNDED_SURFACE()
B_SPLINE_SURFACE(5,1,((#43520,#43521),(#43522,#43523),(#43524,#43525),(#43526,
#43527),(#43528,#43529),(#43530,#43531),(#43532,#43533),(#43534,#43535),
(#43536,#43537),(#43538,#43539),(#43540,#43541),(#43542,#43543),(#43544,
#43545),(#43546,#43547),(#43548,#43549),(#43550,#43551),(#43552,#43553),
(#43554,#43555),(#43556,#43557),(#43558,#43559),(#43560,#43561),(#43562,
#43563),(#43564,#43565),(#43566,#43567),(#43568,#43569),(#43570,#43571),
(#43572,#43573),(#43574,#43575),(#43576,#43577),(#43578,#43579),(#43580,
#43581),(#43582,#43583),(#43584,#43585),(#43586,#43587),(#43588,#43589),
(#43590,#43591),(#43592,#43593),(#43594,#43595),(#43596,#43597),(#43598,
#43599),(#43600,#43601),(#43602,#43603),(#43604,#43605),(#43606,#43607),
(#43608,#43609),(#43610,#43611),(#43612,#43613),(#43614,#43615),(#43616,
#43617),(#43618,#43619),(#43620,#43621),(#43622,#43623),(#43624,#43625),
(#43626,#43627),(#43628,#43629),(#43630,#43631),(#43632,#43633),(#43634,
#43635),(#43636,#43637),(#43638,#43639),(#43640,#43641),(#43642,#43643),
(#43644,#43645),(#43646,#43647),(#43648,#43649),(#43650,#43651),(#43652,
#43653),(#43654,#43655),(#43656,#43657),(#43658,#43659)),.UNSPECIFIED.,
 .F.,.F.,.F.)
B_SPLINE_SURFACE_WITH_KNOTS((6,1,1,1,1,1,1,1,1,1,1,1,1,1,1,1,1,1,1,1,1,
1,1,1,1,1,1,1,1,1,1,1,1,1,1,1,1,1,1,1,1,1,1,1,1,1,1,1,1,1,1,1,1,1,1,1,1,
1,1,1,1,1,1,1,1,6),(2,2),(-1.,-0.984615384615383,-0.969230769230768,-0.953846153846152,
-0.938461538461537,-0.923076923076922,-0.907692307692306,-0.892307692307691,
-0.876923076923076,-0.86153846153846,-0.846153846153845,-0.83076923076923,
-0.815384615384614,-0.799999999999999,-0.784615384615384,-0.769230769230768,
-0.753846153846153,-0.738461538461538,-0.723076923076922,-0.707692307692307,
-0.692307692307692,-0.676923076923076,-0.661538461538461,-0.646153846153846,
-0.63076923076923,-0.615384615384615,-0.6,-0.584615384615384,-0.569230769230769,
-0.553846153846154,-0.538461538461538,-0.523076923076923,-0.507692307692308,
-0.492307692307692,-0.476923076923077,-0.461538461538462,-0.446153846153846,
-0.430769230769231,-0.415384615384615,-0.4,-0.384615384615385,-0.369230769230769,
-0.353846153846154,-0.338461538461538,-0.323076923076923,-0.307692307692308,
-0.292307692307692,-0.276923076923077,-0.261538461538462,-0.246153846153846,
-0.230769230769231,-0.215384615384615,-0.2,-0.184615384615385,-0.169230769230769,
-0.153846153846154,-0.138461538461538,-0.123076923076923,-0.107692307692308,
-0.0923076923076923,-0.0769230769230769,-0.0615384615384615,-0.0461538461538462,
-0.0307692307692308,-0.0153846153846154,0.),(-1.,1.),.UNSPECIFIED.)
GEOMETRIC_REPRESENTATION_ITEM()
RATIONAL_B_SPLINE_SURFACE(((1.,1.),(1.,1.),(1.,1.),(1.,1.),(1.,1.),(1.,
1.),(1.,1.),(1.,1.),(1.,1.),(1.,1.),(1.,1.),(1.,1.),(1.,1.),(1.,1.),(1.,
1.),(1.,1.),(1.,1.),(1.,1.),(1.,1.),(1.,1.),(1.,1.),(1.,1.),(1.,1.),(1.,
1.),(1.,1.),(1.,1.),(1.,1.),(1.,1.),(1.,1.),(1.,1.),(1.,1.),(1.,1.),(1.,
1.),(1.,1.),(1.,1.),(1.,1.),(1.,1.),(1.,1.),(1.,1.),(1.,1.),(1.,1.),(1.,
1.),(1.,1.),(1.,1.),(1.,1.),(1.,1.),(1.,1.),(1.,1.),(1.,1.),(1.,1.),(1.,
1.),(1.,1.),(1.,1.),(1.,1.),(1.,1.),(1.,1.),(1.,1.),(1.,1.),(1.,1.),(1.,
1.),(1.,1.),(1.,1.),(1.,1.),(1.,1.),(1.,1.),(1.,1.),(1.,1.),(1.,1.),(1.,
1.),(1.,1.)))
REPRESENTATION_ITEM('')
SURFACE()
);
#86=(
BOUNDED_SURFACE()
B_SPLINE_SURFACE(5,1,((#43732,#43733),(#43734,#43735),(#43736,#43737),(#43738,
#43739),(#43740,#43741),(#43742,#43743),(#43744,#43745),(#43746,#43747),
(#43748,#43749),(#43750,#43751),(#43752,#43753),(#43754,#43755),(#43756,
#43757),(#43758,#43759),(#43760,#43761),(#43762,#43763),(#43764,#43765),
(#43766,#43767),(#43768,#43769),(#43770,#43771),(#43772,#43773),(#43774,
#43775),(#43776,#43777),(#43778,#43779),(#43780,#43781),(#43782,#43783),
(#43784,#43785),(#43786,#43787),(#43788,#43789),(#43790,#43791),(#43792,
#43793),(#43794,#43795),(#43796,#43797),(#43798,#43799),(#43800,#43801),
(#43802,#43803),(#43804,#43805),(#43806,#43807),(#43808,#43809),(#43810,
#43811),(#43812,#43813),(#43814,#43815),(#43816,#43817),(#43818,#43819),
(#43820,#43821),(#43822,#43823),(#43824,#43825),(#43826,#43827),(#43828,
#43829),(#43830,#43831),(#43832,#43833),(#43834,#43835),(#43836,#43837),
(#43838,#43839),(#43840,#43841),(#43842,#43843),(#43844,#43845),(#43846,
#43847),(#43848,#43849),(#43850,#43851),(#43852,#43853),(#43854,#43855),
(#43856,#43857),(#43858,#43859),(#43860,#43861),(#43862,#43863),(#43864,
#43865),(#43866,#43867),(#43868,#43869),(#43870,#43871)),.UNSPECIFIED.,
 .F.,.F.,.F.)
B_SPLINE_SURFACE_WITH_KNOTS((6,1,1,1,1,1,1,1,1,1,1,1,1,1,1,1,1,1,1,1,1,
1,1,1,1,1,1,1,1,1,1,1,1,1,1,1,1,1,1,1,1,1,1,1,1,1,1,1,1,1,1,1,1,1,1,1,1,
1,1,1,1,1,1,1,1,6),(2,2),(-1.,-0.984615384615383,-0.969230769230768,-0.953846153846152,
-0.938461538461537,-0.923076923076922,-0.907692307692306,-0.892307692307691,
-0.876923076923076,-0.86153846153846,-0.846153846153845,-0.83076923076923,
-0.815384615384614,-0.799999999999999,-0.784615384615384,-0.769230769230768,
-0.753846153846153,-0.738461538461538,-0.723076923076922,-0.707692307692307,
-0.692307692307692,-0.676923076923076,-0.661538461538461,-0.646153846153846,
-0.63076923076923,-0.615384615384615,-0.6,-0.584615384615384,-0.569230769230769,
-0.553846153846154,-0.538461538461538,-0.523076923076923,-0.507692307692308,
-0.492307692307692,-0.476923076923077,-0.461538461538462,-0.446153846153846,
-0.430769230769231,-0.415384615384615,-0.4,-0.384615384615385,-0.369230769230769,
-0.353846153846154,-0.338461538461538,-0.323076923076923,-0.307692307692308,
-0.292307692307692,-0.276923076923077,-0.261538461538462,-0.246153846153846,
-0.230769230769231,-0.215384615384615,-0.2,-0.184615384615385,-0.169230769230769,
-0.153846153846154,-0.138461538461538,-0.123076923076923,-0.107692307692308,
-0.0923076923076923,-0.0769230769230769,-0.0615384615384615,-0.0461538461538462,
-0.0307692307692308,-0.0153846153846154,0.),(-1.,1.),.UNSPECIFIED.)
GEOMETRIC_REPRESENTATION_ITEM()
RATIONAL_B_SPLINE_SURFACE(((1.,1.),(1.,1.),(1.,1.),(1.,1.),(1.,1.),(1.,
1.),(1.,1.),(1.,1.),(1.,1.),(1.,1.),(1.,1.),(1.,1.),(1.,1.),(1.,1.),(1.,
1.),(1.,1.),(1.,1.),(1.,1.),(1.,1.),(1.,1.),(1.,1.),(1.,1.),(1.,1.),(1.,
1.),(1.,1.),(1.,1.),(1.,1.),(1.,1.),(1.,1.),(1.,1.),(1.,1.),(1.,1.),(1.,
1.),(1.,1.),(1.,1.),(1.,1.),(1.,1.),(1.,1.),(1.,1.),(1.,1.),(1.,1.),(1.,
1.),(1.,1.),(1.,1.),(1.,1.),(1.,1.),(1.,1.),(1.,1.),(1.,1.),(1.,1.),(1.,
1.),(1.,1.),(1.,1.),(1.,1.),(1.,1.),(1.,1.),(1.,1.),(1.,1.),(1.,1.),(1.,
1.),(1.,1.),(1.,1.),(1.,1.),(1.,1.),(1.,1.),(1.,1.),(1.,1.),(1.,1.),(1.,
1.),(1.,1.)))
REPRESENTATION_ITEM('')
SURFACE()
);
#87=(
BOUNDED_SURFACE()
B_SPLINE_SURFACE(5,1,((#43962,#43963),(#43964,#43965),(#43966,#43967),(#43968,
#43969),(#43970,#43971),(#43972,#43973),(#43974,#43975),(#43976,#43977),
(#43978,#43979),(#43980,#43981),(#43982,#43983),(#43984,#43985),(#43986,
#43987),(#43988,#43989),(#43990,#43991),(#43992,#43993),(#43994,#43995),
(#43996,#43997),(#43998,#43999),(#44000,#44001),(#44002,#44003),(#44004,
#44005),(#44006,#44007),(#44008,#44009),(#44010,#44011),(#44012,#44013),
(#44014,#44015),(#44016,#44017),(#44018,#44019),(#44020,#44021),(#44022,
#44023),(#44024,#44025),(#44026,#44027),(#44028,#44029),(#44030,#44031),
(#44032,#44033),(#44034,#44035),(#44036,#44037),(#44038,#44039),(#44040,
#44041),(#44042,#44043),(#44044,#44045),(#44046,#44047),(#44048,#44049),
(#44050,#44051),(#44052,#44053),(#44054,#44055),(#44056,#44057),(#44058,
#44059),(#44060,#44061),(#44062,#44063),(#44064,#44065),(#44066,#44067),
(#44068,#44069),(#44070,#44071),(#44072,#44073),(#44074,#44075),(#44076,
#44077),(#44078,#44079),(#44080,#44081),(#44082,#44083),(#44084,#44085),
(#44086,#44087),(#44088,#44089),(#44090,#44091),(#44092,#44093),(#44094,
#44095),(#44096,#44097),(#44098,#44099),(#44100,#44101)),.UNSPECIFIED.,
 .F.,.F.,.F.)
B_SPLINE_SURFACE_WITH_KNOTS((6,1,1,1,1,1,1,1,1,1,1,1,1,1,1,1,1,1,1,1,1,
1,1,1,1,1,1,1,1,1,1,1,1,1,1,1,1,1,1,1,1,1,1,1,1,1,1,1,1,1,1,1,1,1,1,1,1,
1,1,1,1,1,1,1,1,6),(2,2),(-1.,-0.984615384615383,-0.969230769230768,-0.953846153846152,
-0.938461538461537,-0.923076923076922,-0.907692307692306,-0.892307692307691,
-0.876923076923076,-0.86153846153846,-0.846153846153845,-0.83076923076923,
-0.815384615384614,-0.799999999999999,-0.784615384615384,-0.769230769230768,
-0.753846153846153,-0.738461538461538,-0.723076923076922,-0.707692307692307,
-0.692307692307692,-0.676923076923076,-0.661538461538461,-0.646153846153846,
-0.63076923076923,-0.615384615384615,-0.6,-0.584615384615384,-0.569230769230769,
-0.553846153846154,-0.538461538461538,-0.523076923076923,-0.507692307692308,
-0.492307692307692,-0.476923076923077,-0.461538461538462,-0.446153846153846,
-0.430769230769231,-0.415384615384615,-0.4,-0.384615384615385,-0.369230769230769,
-0.353846153846154,-0.338461538461538,-0.323076923076923,-0.307692307692308,
-0.292307692307692,-0.276923076923077,-0.261538461538462,-0.246153846153846,
-0.230769230769231,-0.215384615384615,-0.2,-0.184615384615385,-0.169230769230769,
-0.153846153846154,-0.138461538461538,-0.123076923076923,-0.107692307692308,
-0.0923076923076923,-0.0769230769230769,-0.0615384615384615,-0.0461538461538462,
-0.0307692307692308,-0.0153846153846154,0.),(-1.,1.),.UNSPECIFIED.)
GEOMETRIC_REPRESENTATION_ITEM()
RATIONAL_B_SPLINE_SURFACE(((1.,1.),(1.,1.),(1.,1.),(1.,1.),(1.,1.),(1.,
1.),(1.,1.),(1.,1.),(1.,1.),(1.,1.),(1.,1.),(1.,1.),(1.,1.),(1.,1.),(1.,
1.),(1.,1.),(1.,1.),(1.,1.),(1.,1.),(1.,1.),(1.,1.),(1.,1.),(1.,1.),(1.,
1.),(1.,1.),(1.,1.),(1.,1.),(1.,1.),(1.,1.),(1.,1.),(1.,1.),(1.,1.),(1.,
1.),(1.,1.),(1.,1.),(1.,1.),(1.,1.),(1.,1.),(1.,1.),(1.,1.),(1.,1.),(1.,
1.),(1.,1.),(1.,1.),(1.,1.),(1.,1.),(1.,1.),(1.,1.),(1.,1.),(1.,1.),(1.,
1.),(1.,1.),(1.,1.),(1.,1.),(1.,1.),(1.,1.),(1.,1.),(1.,1.),(1.,1.),(1.,
1.),(1.,1.),(1.,1.),(1.,1.),(1.,1.),(1.,1.),(1.,1.),(1.,1.),(1.,1.),(1.,
1.),(1.,1.)))
REPRESENTATION_ITEM('')
SURFACE()
);
#88=(
BOUNDED_SURFACE()
B_SPLINE_SURFACE(5,1,((#44174,#44175),(#44176,#44177),(#44178,#44179),(#44180,
#44181),(#44182,#44183),(#44184,#44185),(#44186,#44187),(#44188,#44189),
(#44190,#44191),(#44192,#44193),(#44194,#44195),(#44196,#44197),(#44198,
#44199),(#44200,#44201),(#44202,#44203),(#44204,#44205),(#44206,#44207),
(#44208,#44209),(#44210,#44211),(#44212,#44213),(#44214,#44215),(#44216,
#44217),(#44218,#44219),(#44220,#44221),(#44222,#44223),(#44224,#44225),
(#44226,#44227),(#44228,#44229),(#44230,#44231),(#44232,#44233),(#44234,
#44235),(#44236,#44237),(#44238,#44239),(#44240,#44241),(#44242,#44243),
(#44244,#44245),(#44246,#44247),(#44248,#44249),(#44250,#44251),(#44252,
#44253),(#44254,#44255),(#44256,#44257),(#44258,#44259),(#44260,#44261),
(#44262,#44263),(#44264,#44265),(#44266,#44267),(#44268,#44269),(#44270,
#44271),(#44272,#44273),(#44274,#44275),(#44276,#44277),(#44278,#44279),
(#44280,#44281),(#44282,#44283),(#44284,#44285),(#44286,#44287),(#44288,
#44289),(#44290,#44291),(#44292,#44293),(#44294,#44295),(#44296,#44297),
(#44298,#44299),(#44300,#44301),(#44302,#44303),(#44304,#44305),(#44306,
#44307),(#44308,#44309),(#44310,#44311),(#44312,#44313)),.UNSPECIFIED.,
 .F.,.F.,.F.)
B_SPLINE_SURFACE_WITH_KNOTS((6,1,1,1,1,1,1,1,1,1,1,1,1,1,1,1,1,1,1,1,1,
1,1,1,1,1,1,1,1,1,1,1,1,1,1,1,1,1,1,1,1,1,1,1,1,1,1,1,1,1,1,1,1,1,1,1,1,
1,1,1,1,1,1,1,1,6),(2,2),(-1.,-0.984615384615383,-0.969230769230768,-0.953846153846152,
-0.938461538461537,-0.923076923076922,-0.907692307692306,-0.892307692307691,
-0.876923076923076,-0.86153846153846,-0.846153846153845,-0.83076923076923,
-0.815384615384614,-0.799999999999999,-0.784615384615384,-0.769230769230768,
-0.753846153846153,-0.738461538461538,-0.723076923076922,-0.707692307692307,
-0.692307692307692,-0.676923076923076,-0.661538461538461,-0.646153846153846,
-0.63076923076923,-0.615384615384615,-0.6,-0.584615384615384,-0.569230769230769,
-0.553846153846154,-0.538461538461538,-0.523076923076923,-0.507692307692308,
-0.492307692307692,-0.476923076923077,-0.461538461538462,-0.446153846153846,
-0.430769230769231,-0.415384615384615,-0.4,-0.384615384615385,-0.369230769230769,
-0.353846153846154,-0.338461538461538,-0.323076923076923,-0.307692307692308,
-0.292307692307692,-0.276923076923077,-0.261538461538462,-0.246153846153846,
-0.230769230769231,-0.215384615384615,-0.2,-0.184615384615385,-0.169230769230769,
-0.153846153846154,-0.138461538461538,-0.123076923076923,-0.107692307692308,
-0.0923076923076923,-0.0769230769230769,-0.0615384615384615,-0.0461538461538462,
-0.0307692307692308,-0.0153846153846154,0.),(-1.,1.),.UNSPECIFIED.)
GEOMETRIC_REPRESENTATION_ITEM()
RATIONAL_B_SPLINE_SURFACE(((1.,1.),(1.,1.),(1.,1.),(1.,1.),(1.,1.),(1.,
1.),(1.,1.),(1.,1.),(1.,1.),(1.,1.),(1.,1.),(1.,1.),(1.,1.),(1.,1.),(1.,
1.),(1.,1.),(1.,1.),(1.,1.),(1.,1.),(1.,1.),(1.,1.),(1.,1.),(1.,1.),(1.,
1.),(1.,1.),(1.,1.),(1.,1.),(1.,1.),(1.,1.),(1.,1.),(1.,1.),(1.,1.),(1.,
1.),(1.,1.),(1.,1.),(1.,1.),(1.,1.),(1.,1.),(1.,1.),(1.,1.),(1.,1.),(1.,
1.),(1.,1.),(1.,1.),(1.,1.),(1.,1.),(1.,1.),(1.,1.),(1.,1.),(1.,1.),(1.,
1.),(1.,1.),(1.,1.),(1.,1.),(1.,1.),(1.,1.),(1.,1.),(1.,1.),(1.,1.),(1.,
1.),(1.,1.),(1.,1.),(1.,1.),(1.,1.),(1.,1.),(1.,1.),(1.,1.),(1.,1.),(1.,
1.),(1.,1.)))
REPRESENTATION_ITEM('')
SURFACE()
);
#89=(
BOUNDED_SURFACE()
B_SPLINE_SURFACE(5,1,((#44404,#44405),(#44406,#44407),(#44408,#44409),(#44410,
#44411),(#44412,#44413),(#44414,#44415),(#44416,#44417),(#44418,#44419),
(#44420,#44421),(#44422,#44423),(#44424,#44425),(#44426,#44427),(#44428,
#44429),(#44430,#44431),(#44432,#44433),(#44434,#44435),(#44436,#44437),
(#44438,#44439),(#44440,#44441),(#44442,#44443),(#44444,#44445),(#44446,
#44447),(#44448,#44449),(#44450,#44451),(#44452,#44453),(#44454,#44455),
(#44456,#44457),(#44458,#44459),(#44460,#44461),(#44462,#44463),(#44464,
#44465),(#44466,#44467),(#44468,#44469),(#44470,#44471),(#44472,#44473),
(#44474,#44475),(#44476,#44477),(#44478,#44479),(#44480,#44481),(#44482,
#44483),(#44484,#44485),(#44486,#44487),(#44488,#44489),(#44490,#44491),
(#44492,#44493),(#44494,#44495),(#44496,#44497),(#44498,#44499),(#44500,
#44501),(#44502,#44503),(#44504,#44505),(#44506,#44507),(#44508,#44509),
(#44510,#44511),(#44512,#44513),(#44514,#44515),(#44516,#44517),(#44518,
#44519),(#44520,#44521),(#44522,#44523),(#44524,#44525),(#44526,#44527),
(#44528,#44529),(#44530,#44531),(#44532,#44533),(#44534,#44535),(#44536,
#44537),(#44538,#44539),(#44540,#44541),(#44542,#44543)),.UNSPECIFIED.,
 .F.,.F.,.F.)
B_SPLINE_SURFACE_WITH_KNOTS((6,1,1,1,1,1,1,1,1,1,1,1,1,1,1,1,1,1,1,1,1,
1,1,1,1,1,1,1,1,1,1,1,1,1,1,1,1,1,1,1,1,1,1,1,1,1,1,1,1,1,1,1,1,1,1,1,1,
1,1,1,1,1,1,1,1,6),(2,2),(-1.,-0.984615384615383,-0.969230769230768,-0.953846153846152,
-0.938461538461537,-0.923076923076922,-0.907692307692306,-0.892307692307691,
-0.876923076923076,-0.86153846153846,-0.846153846153845,-0.83076923076923,
-0.815384615384614,-0.799999999999999,-0.784615384615384,-0.769230769230768,
-0.753846153846153,-0.738461538461538,-0.723076923076922,-0.707692307692307,
-0.692307692307692,-0.676923076923076,-0.661538461538461,-0.646153846153846,
-0.63076923076923,-0.615384615384615,-0.6,-0.584615384615384,-0.569230769230769,
-0.553846153846154,-0.538461538461538,-0.523076923076923,-0.507692307692308,
-0.492307692307692,-0.476923076923077,-0.461538461538462,-0.446153846153846,
-0.430769230769231,-0.415384615384615,-0.4,-0.384615384615385,-0.369230769230769,
-0.353846153846154,-0.338461538461538,-0.323076923076923,-0.307692307692308,
-0.292307692307692,-0.276923076923077,-0.261538461538462,-0.246153846153846,
-0.230769230769231,-0.215384615384615,-0.2,-0.184615384615385,-0.169230769230769,
-0.153846153846154,-0.138461538461538,-0.123076923076923,-0.107692307692308,
-0.0923076923076923,-0.0769230769230769,-0.0615384615384615,-0.0461538461538462,
-0.0307692307692308,-0.0153846153846154,0.),(-1.,1.),.UNSPECIFIED.)
GEOMETRIC_REPRESENTATION_ITEM()
RATIONAL_B_SPLINE_SURFACE(((1.,1.),(1.,1.),(1.,1.),(1.,1.),(1.,1.),(1.,
1.),(1.,1.),(1.,1.),(1.,1.),(1.,1.),(1.,1.),(1.,1.),(1.,1.),(1.,1.),(1.,
1.),(1.,1.),(1.,1.),(1.,1.),(1.,1.),(1.,1.),(1.,1.),(1.,1.),(1.,1.),(1.,
1.),(1.,1.),(1.,1.),(1.,1.),(1.,1.),(1.,1.),(1.,1.),(1.,1.),(1.,1.),(1.,
1.),(1.,1.),(1.,1.),(1.,1.),(1.,1.),(1.,1.),(1.,1.),(1.,1.),(1.,1.),(1.,
1.),(1.,1.),(1.,1.),(1.,1.),(1.,1.),(1.,1.),(1.,1.),(1.,1.),(1.,1.),(1.,
1.),(1.,1.),(1.,1.),(1.,1.),(1.,1.),(1.,1.),(1.,1.),(1.,1.),(1.,1.),(1.,
1.),(1.,1.),(1.,1.),(1.,1.),(1.,1.),(1.,1.),(1.,1.),(1.,1.),(1.,1.),(1.,
1.),(1.,1.)))
REPRESENTATION_ITEM('')
SURFACE()
);
#90=(
BOUNDED_SURFACE()
B_SPLINE_SURFACE(5,1,((#44616,#44617),(#44618,#44619),(#44620,#44621),(#44622,
#44623),(#44624,#44625),(#44626,#44627),(#44628,#44629),(#44630,#44631),
(#44632,#44633),(#44634,#44635),(#44636,#44637),(#44638,#44639),(#44640,
#44641),(#44642,#44643),(#44644,#44645),(#44646,#44647),(#44648,#44649),
(#44650,#44651),(#44652,#44653),(#44654,#44655),(#44656,#44657),(#44658,
#44659),(#44660,#44661),(#44662,#44663),(#44664,#44665),(#44666,#44667),
(#44668,#44669),(#44670,#44671),(#44672,#44673),(#44674,#44675),(#44676,
#44677),(#44678,#44679),(#44680,#44681),(#44682,#44683),(#44684,#44685),
(#44686,#44687),(#44688,#44689),(#44690,#44691),(#44692,#44693),(#44694,
#44695),(#44696,#44697),(#44698,#44699),(#44700,#44701),(#44702,#44703),
(#44704,#44705),(#44706,#44707),(#44708,#44709),(#44710,#44711),(#44712,
#44713),(#44714,#44715),(#44716,#44717),(#44718,#44719),(#44720,#44721),
(#44722,#44723),(#44724,#44725),(#44726,#44727),(#44728,#44729),(#44730,
#44731),(#44732,#44733),(#44734,#44735),(#44736,#44737),(#44738,#44739),
(#44740,#44741),(#44742,#44743),(#44744,#44745),(#44746,#44747),(#44748,
#44749),(#44750,#44751),(#44752,#44753),(#44754,#44755)),.UNSPECIFIED.,
 .F.,.F.,.F.)
B_SPLINE_SURFACE_WITH_KNOTS((6,1,1,1,1,1,1,1,1,1,1,1,1,1,1,1,1,1,1,1,1,
1,1,1,1,1,1,1,1,1,1,1,1,1,1,1,1,1,1,1,1,1,1,1,1,1,1,1,1,1,1,1,1,1,1,1,1,
1,1,1,1,1,1,1,1,6),(2,2),(-1.,-0.984615384615383,-0.969230769230768,-0.953846153846152,
-0.938461538461537,-0.923076923076922,-0.907692307692306,-0.892307692307691,
-0.876923076923076,-0.86153846153846,-0.846153846153845,-0.83076923076923,
-0.815384615384614,-0.799999999999999,-0.784615384615384,-0.769230769230768,
-0.753846153846153,-0.738461538461538,-0.723076923076922,-0.707692307692307,
-0.692307692307692,-0.676923076923076,-0.661538461538461,-0.646153846153846,
-0.63076923076923,-0.615384615384615,-0.6,-0.584615384615384,-0.569230769230769,
-0.553846153846154,-0.538461538461538,-0.523076923076923,-0.507692307692308,
-0.492307692307692,-0.476923076923077,-0.461538461538462,-0.446153846153846,
-0.430769230769231,-0.415384615384615,-0.4,-0.384615384615385,-0.369230769230769,
-0.353846153846154,-0.338461538461538,-0.323076923076923,-0.307692307692308,
-0.292307692307692,-0.276923076923077,-0.261538461538462,-0.246153846153846,
-0.230769230769231,-0.215384615384615,-0.2,-0.184615384615385,-0.169230769230769,
-0.153846153846154,-0.138461538461538,-0.123076923076923,-0.107692307692308,
-0.0923076923076923,-0.0769230769230769,-0.0615384615384615,-0.0461538461538462,
-0.0307692307692308,-0.0153846153846154,0.),(-1.,1.),.UNSPECIFIED.)
GEOMETRIC_REPRESENTATION_ITEM()
RATIONAL_B_SPLINE_SURFACE(((1.,1.),(1.,1.),(1.,1.),(1.,1.),(1.,1.),(1.,
1.),(1.,1.),(1.,1.),(1.,1.),(1.,1.),(1.,1.),(1.,1.),(1.,1.),(1.,1.),(1.,
1.),(1.,1.),(1.,1.),(1.,1.),(1.,1.),(1.,1.),(1.,1.),(1.,1.),(1.,1.),(1.,
1.),(1.,1.),(1.,1.),(1.,1.),(1.,1.),(1.,1.),(1.,1.),(1.,1.),(1.,1.),(1.,
1.),(1.,1.),(1.,1.),(1.,1.),(1.,1.),(1.,1.),(1.,1.),(1.,1.),(1.,1.),(1.,
1.),(1.,1.),(1.,1.),(1.,1.),(1.,1.),(1.,1.),(1.,1.),(1.,1.),(1.,1.),(1.,
1.),(1.,1.),(1.,1.),(1.,1.),(1.,1.),(1.,1.),(1.,1.),(1.,1.),(1.,1.),(1.,
1.),(1.,1.),(1.,1.),(1.,1.),(1.,1.),(1.,1.),(1.,1.),(1.,1.),(1.,1.),(1.,
1.),(1.,1.)))
REPRESENTATION_ITEM('')
SURFACE()
);
#91=(
BOUNDED_SURFACE()
B_SPLINE_SURFACE(5,1,((#44846,#44847),(#44848,#44849),(#44850,#44851),(#44852,
#44853),(#44854,#44855),(#44856,#44857),(#44858,#44859),(#44860,#44861),
(#44862,#44863),(#44864,#44865),(#44866,#44867),(#44868,#44869),(#44870,
#44871),(#44872,#44873),(#44874,#44875),(#44876,#44877),(#44878,#44879),
(#44880,#44881),(#44882,#44883),(#44884,#44885),(#44886,#44887),(#44888,
#44889),(#44890,#44891),(#44892,#44893),(#44894,#44895),(#44896,#44897),
(#44898,#44899),(#44900,#44901),(#44902,#44903),(#44904,#44905),(#44906,
#44907),(#44908,#44909),(#44910,#44911),(#44912,#44913),(#44914,#44915),
(#44916,#44917),(#44918,#44919),(#44920,#44921),(#44922,#44923),(#44924,
#44925),(#44926,#44927),(#44928,#44929),(#44930,#44931),(#44932,#44933),
(#44934,#44935),(#44936,#44937),(#44938,#44939),(#44940,#44941),(#44942,
#44943),(#44944,#44945),(#44946,#44947),(#44948,#44949),(#44950,#44951),
(#44952,#44953),(#44954,#44955),(#44956,#44957),(#44958,#44959),(#44960,
#44961),(#44962,#44963),(#44964,#44965),(#44966,#44967),(#44968,#44969),
(#44970,#44971),(#44972,#44973),(#44974,#44975),(#44976,#44977),(#44978,
#44979),(#44980,#44981),(#44982,#44983),(#44984,#44985)),.UNSPECIFIED.,
 .F.,.F.,.F.)
B_SPLINE_SURFACE_WITH_KNOTS((6,1,1,1,1,1,1,1,1,1,1,1,1,1,1,1,1,1,1,1,1,
1,1,1,1,1,1,1,1,1,1,1,1,1,1,1,1,1,1,1,1,1,1,1,1,1,1,1,1,1,1,1,1,1,1,1,1,
1,1,1,1,1,1,1,1,6),(2,2),(-1.,-0.984615384615383,-0.969230769230768,-0.953846153846152,
-0.938461538461537,-0.923076923076922,-0.907692307692306,-0.892307692307691,
-0.876923076923076,-0.86153846153846,-0.846153846153845,-0.83076923076923,
-0.815384615384614,-0.799999999999999,-0.784615384615384,-0.769230769230768,
-0.753846153846153,-0.738461538461538,-0.723076923076922,-0.707692307692307,
-0.692307692307692,-0.676923076923076,-0.661538461538461,-0.646153846153846,
-0.63076923076923,-0.615384615384615,-0.6,-0.584615384615384,-0.569230769230769,
-0.553846153846154,-0.538461538461538,-0.523076923076923,-0.507692307692308,
-0.492307692307692,-0.476923076923077,-0.461538461538462,-0.446153846153846,
-0.430769230769231,-0.415384615384615,-0.4,-0.384615384615385,-0.369230769230769,
-0.353846153846154,-0.338461538461538,-0.323076923076923,-0.307692307692308,
-0.292307692307692,-0.276923076923077,-0.261538461538462,-0.246153846153846,
-0.230769230769231,-0.215384615384615,-0.2,-0.184615384615385,-0.169230769230769,
-0.153846153846154,-0.138461538461538,-0.123076923076923,-0.107692307692308,
-0.0923076923076923,-0.0769230769230769,-0.0615384615384615,-0.0461538461538462,
-0.0307692307692308,-0.0153846153846154,0.),(-1.,1.),.UNSPECIFIED.)
GEOMETRIC_REPRESENTATION_ITEM()
RATIONAL_B_SPLINE_SURFACE(((1.,1.),(1.,1.),(1.,1.),(1.,1.),(1.,1.),(1.,
1.),(1.,1.),(1.,1.),(1.,1.),(1.,1.),(1.,1.),(1.,1.),(1.,1.),(1.,1.),(1.,
1.),(1.,1.),(1.,1.),(1.,1.),(1.,1.),(1.,1.),(1.,1.),(1.,1.),(1.,1.),(1.,
1.),(1.,1.),(1.,1.),(1.,1.),(1.,1.),(1.,1.),(1.,1.),(1.,1.),(1.,1.),(1.,
1.),(1.,1.),(1.,1.),(1.,1.),(1.,1.),(1.,1.),(1.,1.),(1.,1.),(1.,1.),(1.,
1.),(1.,1.),(1.,1.),(1.,1.),(1.,1.),(1.,1.),(1.,1.),(1.,1.),(1.,1.),(1.,
1.),(1.,1.),(1.,1.),(1.,1.),(1.,1.),(1.,1.),(1.,1.),(1.,1.),(1.,1.),(1.,
1.),(1.,1.),(1.,1.),(1.,1.),(1.,1.),(1.,1.),(1.,1.),(1.,1.),(1.,1.),(1.,
1.),(1.,1.)))
REPRESENTATION_ITEM('')
SURFACE()
);
#92=(
BOUNDED_SURFACE()
B_SPLINE_SURFACE(5,1,((#45058,#45059),(#45060,#45061),(#45062,#45063),(#45064,
#45065),(#45066,#45067),(#45068,#45069),(#45070,#45071),(#45072,#45073),
(#45074,#45075),(#45076,#45077),(#45078,#45079),(#45080,#45081),(#45082,
#45083),(#45084,#45085),(#45086,#45087),(#45088,#45089),(#45090,#45091),
(#45092,#45093),(#45094,#45095),(#45096,#45097),(#45098,#45099),(#45100,
#45101),(#45102,#45103),(#45104,#45105),(#45106,#45107),(#45108,#45109),
(#45110,#45111),(#45112,#45113),(#45114,#45115),(#45116,#45117),(#45118,
#45119),(#45120,#45121),(#45122,#45123),(#45124,#45125),(#45126,#45127),
(#45128,#45129),(#45130,#45131),(#45132,#45133),(#45134,#45135),(#45136,
#45137),(#45138,#45139),(#45140,#45141),(#45142,#45143),(#45144,#45145),
(#45146,#45147),(#45148,#45149),(#45150,#45151),(#45152,#45153),(#45154,
#45155),(#45156,#45157),(#45158,#45159),(#45160,#45161),(#45162,#45163),
(#45164,#45165),(#45166,#45167),(#45168,#45169),(#45170,#45171),(#45172,
#45173),(#45174,#45175),(#45176,#45177),(#45178,#45179),(#45180,#45181),
(#45182,#45183),(#45184,#45185),(#45186,#45187),(#45188,#45189),(#45190,
#45191),(#45192,#45193),(#45194,#45195),(#45196,#45197)),.UNSPECIFIED.,
 .F.,.F.,.F.)
B_SPLINE_SURFACE_WITH_KNOTS((6,1,1,1,1,1,1,1,1,1,1,1,1,1,1,1,1,1,1,1,1,
1,1,1,1,1,1,1,1,1,1,1,1,1,1,1,1,1,1,1,1,1,1,1,1,1,1,1,1,1,1,1,1,1,1,1,1,
1,1,1,1,1,1,1,1,6),(2,2),(-1.,-0.984615384615383,-0.969230769230768,-0.953846153846152,
-0.938461538461537,-0.923076923076922,-0.907692307692306,-0.892307692307691,
-0.876923076923076,-0.86153846153846,-0.846153846153845,-0.83076923076923,
-0.815384615384614,-0.799999999999999,-0.784615384615384,-0.769230769230768,
-0.753846153846153,-0.738461538461538,-0.723076923076922,-0.707692307692307,
-0.692307692307692,-0.676923076923076,-0.661538461538461,-0.646153846153846,
-0.63076923076923,-0.615384615384615,-0.6,-0.584615384615384,-0.569230769230769,
-0.553846153846154,-0.538461538461538,-0.523076923076923,-0.507692307692308,
-0.492307692307692,-0.476923076923077,-0.461538461538462,-0.446153846153846,
-0.430769230769231,-0.415384615384615,-0.4,-0.384615384615385,-0.369230769230769,
-0.353846153846154,-0.338461538461538,-0.323076923076923,-0.307692307692308,
-0.292307692307692,-0.276923076923077,-0.261538461538462,-0.246153846153846,
-0.230769230769231,-0.215384615384615,-0.2,-0.184615384615385,-0.169230769230769,
-0.153846153846154,-0.138461538461538,-0.123076923076923,-0.107692307692308,
-0.0923076923076923,-0.0769230769230769,-0.0615384615384615,-0.0461538461538462,
-0.0307692307692308,-0.0153846153846154,0.),(-1.,1.),.UNSPECIFIED.)
GEOMETRIC_REPRESENTATION_ITEM()
RATIONAL_B_SPLINE_SURFACE(((1.,1.),(1.,1.),(1.,1.),(1.,1.),(1.,1.),(1.,
1.),(1.,1.),(1.,1.),(1.,1.),(1.,1.),(1.,1.),(1.,1.),(1.,1.),(1.,1.),(1.,
1.),(1.,1.),(1.,1.),(1.,1.),(1.,1.),(1.,1.),(1.,1.),(1.,1.),(1.,1.),(1.,
1.),(1.,1.),(1.,1.),(1.,1.),(1.,1.),(1.,1.),(1.,1.),(1.,1.),(1.,1.),(1.,
1.),(1.,1.),(1.,1.),(1.,1.),(1.,1.),(1.,1.),(1.,1.),(1.,1.),(1.,1.),(1.,
1.),(1.,1.),(1.,1.),(1.,1.),(1.,1.),(1.,1.),(1.,1.),(1.,1.),(1.,1.),(1.,
1.),(1.,1.),(1.,1.),(1.,1.),(1.,1.),(1.,1.),(1.,1.),(1.,1.),(1.,1.),(1.,
1.),(1.,1.),(1.,1.),(1.,1.),(1.,1.),(1.,1.),(1.,1.),(1.,1.),(1.,1.),(1.,
1.),(1.,1.)))
REPRESENTATION_ITEM('')
SURFACE()
);
#93=(
BOUNDED_SURFACE()
B_SPLINE_SURFACE(5,1,((#45288,#45289),(#45290,#45291),(#45292,#45293),(#45294,
#45295),(#45296,#45297),(#45298,#45299),(#45300,#45301),(#45302,#45303),
(#45304,#45305),(#45306,#45307),(#45308,#45309),(#45310,#45311),(#45312,
#45313),(#45314,#45315),(#45316,#45317),(#45318,#45319),(#45320,#45321),
(#45322,#45323),(#45324,#45325),(#45326,#45327),(#45328,#45329),(#45330,
#45331),(#45332,#45333),(#45334,#45335),(#45336,#45337),(#45338,#45339),
(#45340,#45341),(#45342,#45343),(#45344,#45345),(#45346,#45347),(#45348,
#45349),(#45350,#45351),(#45352,#45353),(#45354,#45355),(#45356,#45357),
(#45358,#45359),(#45360,#45361),(#45362,#45363),(#45364,#45365),(#45366,
#45367),(#45368,#45369),(#45370,#45371),(#45372,#45373),(#45374,#45375),
(#45376,#45377),(#45378,#45379),(#45380,#45381),(#45382,#45383),(#45384,
#45385),(#45386,#45387),(#45388,#45389),(#45390,#45391),(#45392,#45393),
(#45394,#45395),(#45396,#45397),(#45398,#45399),(#45400,#45401),(#45402,
#45403),(#45404,#45405),(#45406,#45407),(#45408,#45409),(#45410,#45411),
(#45412,#45413),(#45414,#45415),(#45416,#45417),(#45418,#45419),(#45420,
#45421),(#45422,#45423),(#45424,#45425),(#45426,#45427)),.UNSPECIFIED.,
 .F.,.F.,.F.)
B_SPLINE_SURFACE_WITH_KNOTS((6,1,1,1,1,1,1,1,1,1,1,1,1,1,1,1,1,1,1,1,1,
1,1,1,1,1,1,1,1,1,1,1,1,1,1,1,1,1,1,1,1,1,1,1,1,1,1,1,1,1,1,1,1,1,1,1,1,
1,1,1,1,1,1,1,1,6),(2,2),(-1.,-0.984615384615383,-0.969230769230768,-0.953846153846152,
-0.938461538461537,-0.923076923076922,-0.907692307692306,-0.892307692307691,
-0.876923076923076,-0.86153846153846,-0.846153846153845,-0.83076923076923,
-0.815384615384614,-0.799999999999999,-0.784615384615384,-0.769230769230768,
-0.753846153846153,-0.738461538461538,-0.723076923076922,-0.707692307692307,
-0.692307692307692,-0.676923076923076,-0.661538461538461,-0.646153846153846,
-0.63076923076923,-0.615384615384615,-0.6,-0.584615384615384,-0.569230769230769,
-0.553846153846154,-0.538461538461538,-0.523076923076923,-0.507692307692308,
-0.492307692307692,-0.476923076923077,-0.461538461538462,-0.446153846153846,
-0.430769230769231,-0.415384615384615,-0.4,-0.384615384615385,-0.369230769230769,
-0.353846153846154,-0.338461538461538,-0.323076923076923,-0.307692307692308,
-0.292307692307692,-0.276923076923077,-0.261538461538462,-0.246153846153846,
-0.230769230769231,-0.215384615384615,-0.2,-0.184615384615385,-0.169230769230769,
-0.153846153846154,-0.138461538461538,-0.123076923076923,-0.107692307692308,
-0.0923076923076923,-0.0769230769230769,-0.0615384615384615,-0.0461538461538462,
-0.0307692307692308,-0.0153846153846154,0.),(-1.,1.),.UNSPECIFIED.)
GEOMETRIC_REPRESENTATION_ITEM()
RATIONAL_B_SPLINE_SURFACE(((1.,1.),(1.,1.),(1.,1.),(1.,1.),(1.,1.),(1.,
1.),(1.,1.),(1.,1.),(1.,1.),(1.,1.),(1.,1.),(1.,1.),(1.,1.),(1.,1.),(1.,
1.),(1.,1.),(1.,1.),(1.,1.),(1.,1.),(1.,1.),(1.,1.),(1.,1.),(1.,1.),(1.,
1.),(1.,1.),(1.,1.),(1.,1.),(1.,1.),(1.,1.),(1.,1.),(1.,1.),(1.,1.),(1.,
1.),(1.,1.),(1.,1.),(1.,1.),(1.,1.),(1.,1.),(1.,1.),(1.,1.),(1.,1.),(1.,
1.),(1.,1.),(1.,1.),(1.,1.),(1.,1.),(1.,1.),(1.,1.),(1.,1.),(1.,1.),(1.,
1.),(1.,1.),(1.,1.),(1.,1.),(1.,1.),(1.,1.),(1.,1.),(1.,1.),(1.,1.),(1.,
1.),(1.,1.),(1.,1.),(1.,1.),(1.,1.),(1.,1.),(1.,1.),(1.,1.),(1.,1.),(1.,
1.),(1.,1.)))
REPRESENTATION_ITEM('')
SURFACE()
);
#94=(
BOUNDED_SURFACE()
B_SPLINE_SURFACE(5,1,((#45500,#45501),(#45502,#45503),(#45504,#45505),(#45506,
#45507),(#45508,#45509),(#45510,#45511),(#45512,#45513),(#45514,#45515),
(#45516,#45517),(#45518,#45519),(#45520,#45521),(#45522,#45523),(#45524,
#45525),(#45526,#45527),(#45528,#45529),(#45530,#45531),(#45532,#45533),
(#45534,#45535),(#45536,#45537),(#45538,#45539),(#45540,#45541),(#45542,
#45543),(#45544,#45545),(#45546,#45547),(#45548,#45549),(#45550,#45551),
(#45552,#45553),(#45554,#45555),(#45556,#45557),(#45558,#45559),(#45560,
#45561),(#45562,#45563),(#45564,#45565),(#45566,#45567),(#45568,#45569),
(#45570,#45571),(#45572,#45573),(#45574,#45575),(#45576,#45577),(#45578,
#45579),(#45580,#45581),(#45582,#45583),(#45584,#45585),(#45586,#45587),
(#45588,#45589),(#45590,#45591),(#45592,#45593),(#45594,#45595),(#45596,
#45597),(#45598,#45599),(#45600,#45601),(#45602,#45603),(#45604,#45605),
(#45606,#45607),(#45608,#45609),(#45610,#45611),(#45612,#45613),(#45614,
#45615),(#45616,#45617),(#45618,#45619),(#45620,#45621),(#45622,#45623),
(#45624,#45625),(#45626,#45627),(#45628,#45629),(#45630,#45631),(#45632,
#45633),(#45634,#45635),(#45636,#45637),(#45638,#45639)),.UNSPECIFIED.,
 .F.,.F.,.F.)
B_SPLINE_SURFACE_WITH_KNOTS((6,1,1,1,1,1,1,1,1,1,1,1,1,1,1,1,1,1,1,1,1,
1,1,1,1,1,1,1,1,1,1,1,1,1,1,1,1,1,1,1,1,1,1,1,1,1,1,1,1,1,1,1,1,1,1,1,1,
1,1,1,1,1,1,1,1,6),(2,2),(-1.,-0.984615384615383,-0.969230769230768,-0.953846153846152,
-0.938461538461537,-0.923076923076922,-0.907692307692306,-0.892307692307691,
-0.876923076923076,-0.86153846153846,-0.846153846153845,-0.83076923076923,
-0.815384615384614,-0.799999999999999,-0.784615384615384,-0.769230769230768,
-0.753846153846153,-0.738461538461538,-0.723076923076922,-0.707692307692307,
-0.692307692307692,-0.676923076923076,-0.661538461538461,-0.646153846153846,
-0.63076923076923,-0.615384615384615,-0.6,-0.584615384615384,-0.569230769230769,
-0.553846153846154,-0.538461538461538,-0.523076923076923,-0.507692307692308,
-0.492307692307692,-0.476923076923077,-0.461538461538462,-0.446153846153846,
-0.430769230769231,-0.415384615384615,-0.4,-0.384615384615385,-0.369230769230769,
-0.353846153846154,-0.338461538461538,-0.323076923076923,-0.307692307692308,
-0.292307692307692,-0.276923076923077,-0.261538461538462,-0.246153846153846,
-0.230769230769231,-0.215384615384615,-0.2,-0.184615384615385,-0.169230769230769,
-0.153846153846154,-0.138461538461538,-0.123076923076923,-0.107692307692308,
-0.0923076923076923,-0.0769230769230769,-0.0615384615384615,-0.0461538461538462,
-0.0307692307692308,-0.0153846153846154,0.),(-1.,1.),.UNSPECIFIED.)
GEOMETRIC_REPRESENTATION_ITEM()
RATIONAL_B_SPLINE_SURFACE(((1.,1.),(1.,1.),(1.,1.),(1.,1.),(1.,1.),(1.,
1.),(1.,1.),(1.,1.),(1.,1.),(1.,1.),(1.,1.),(1.,1.),(1.,1.),(1.,1.),(1.,
1.),(1.,1.),(1.,1.),(1.,1.),(1.,1.),(1.,1.),(1.,1.),(1.,1.),(1.,1.),(1.,
1.),(1.,1.),(1.,1.),(1.,1.),(1.,1.),(1.,1.),(1.,1.),(1.,1.),(1.,1.),(1.,
1.),(1.,1.),(1.,1.),(1.,1.),(1.,1.),(1.,1.),(1.,1.),(1.,1.),(1.,1.),(1.,
1.),(1.,1.),(1.,1.),(1.,1.),(1.,1.),(1.,1.),(1.,1.),(1.,1.),(1.,1.),(1.,
1.),(1.,1.),(1.,1.),(1.,1.),(1.,1.),(1.,1.),(1.,1.),(1.,1.),(1.,1.),(1.,
1.),(1.,1.),(1.,1.),(1.,1.),(1.,1.),(1.,1.),(1.,1.),(1.,1.),(1.,1.),(1.,
1.),(1.,1.)))
REPRESENTATION_ITEM('')
SURFACE()
);
#95=(
BOUNDED_SURFACE()
B_SPLINE_SURFACE(5,1,((#45730,#45731),(#45732,#45733),(#45734,#45735),(#45736,
#45737),(#45738,#45739),(#45740,#45741),(#45742,#45743),(#45744,#45745),
(#45746,#45747),(#45748,#45749),(#45750,#45751),(#45752,#45753),(#45754,
#45755),(#45756,#45757),(#45758,#45759),(#45760,#45761),(#45762,#45763),
(#45764,#45765),(#45766,#45767),(#45768,#45769),(#45770,#45771),(#45772,
#45773),(#45774,#45775),(#45776,#45777),(#45778,#45779),(#45780,#45781),
(#45782,#45783),(#45784,#45785),(#45786,#45787),(#45788,#45789),(#45790,
#45791),(#45792,#45793),(#45794,#45795),(#45796,#45797),(#45798,#45799),
(#45800,#45801),(#45802,#45803),(#45804,#45805),(#45806,#45807),(#45808,
#45809),(#45810,#45811),(#45812,#45813),(#45814,#45815),(#45816,#45817),
(#45818,#45819),(#45820,#45821),(#45822,#45823),(#45824,#45825),(#45826,
#45827),(#45828,#45829),(#45830,#45831),(#45832,#45833),(#45834,#45835),
(#45836,#45837),(#45838,#45839),(#45840,#45841),(#45842,#45843),(#45844,
#45845),(#45846,#45847),(#45848,#45849),(#45850,#45851),(#45852,#45853),
(#45854,#45855),(#45856,#45857),(#45858,#45859),(#45860,#45861),(#45862,
#45863),(#45864,#45865),(#45866,#45867),(#45868,#45869)),.UNSPECIFIED.,
 .F.,.F.,.F.)
B_SPLINE_SURFACE_WITH_KNOTS((6,1,1,1,1,1,1,1,1,1,1,1,1,1,1,1,1,1,1,1,1,
1,1,1,1,1,1,1,1,1,1,1,1,1,1,1,1,1,1,1,1,1,1,1,1,1,1,1,1,1,1,1,1,1,1,1,1,
1,1,1,1,1,1,1,1,6),(2,2),(-1.,-0.984615384615383,-0.969230769230768,-0.953846153846152,
-0.938461538461537,-0.923076923076922,-0.907692307692306,-0.892307692307691,
-0.876923076923076,-0.86153846153846,-0.846153846153845,-0.83076923076923,
-0.815384615384614,-0.799999999999999,-0.784615384615384,-0.769230769230768,
-0.753846153846153,-0.738461538461538,-0.723076923076922,-0.707692307692307,
-0.692307692307692,-0.676923076923076,-0.661538461538461,-0.646153846153846,
-0.63076923076923,-0.615384615384615,-0.6,-0.584615384615384,-0.569230769230769,
-0.553846153846154,-0.538461538461538,-0.523076923076923,-0.507692307692308,
-0.492307692307692,-0.476923076923077,-0.461538461538462,-0.446153846153846,
-0.430769230769231,-0.415384615384615,-0.4,-0.384615384615385,-0.369230769230769,
-0.353846153846154,-0.338461538461538,-0.323076923076923,-0.307692307692308,
-0.292307692307692,-0.276923076923077,-0.261538461538462,-0.246153846153846,
-0.230769230769231,-0.215384615384615,-0.2,-0.184615384615385,-0.169230769230769,
-0.153846153846154,-0.138461538461538,-0.123076923076923,-0.107692307692308,
-0.0923076923076923,-0.0769230769230769,-0.0615384615384615,-0.0461538461538462,
-0.0307692307692308,-0.0153846153846154,0.),(-1.,1.),.UNSPECIFIED.)
GEOMETRIC_REPRESENTATION_ITEM()
RATIONAL_B_SPLINE_SURFACE(((1.,1.),(1.,1.),(1.,1.),(1.,1.),(1.,1.),(1.,
1.),(1.,1.),(1.,1.),(1.,1.),(1.,1.),(1.,1.),(1.,1.),(1.,1.),(1.,1.),(1.,
1.),(1.,1.),(1.,1.),(1.,1.),(1.,1.),(1.,1.),(1.,1.),(1.,1.),(1.,1.),(1.,
1.),(1.,1.),(1.,1.),(1.,1.),(1.,1.),(1.,1.),(1.,1.),(1.,1.),(1.,1.),(1.,
1.),(1.,1.),(1.,1.),(1.,1.),(1.,1.),(1.,1.),(1.,1.),(1.,1.),(1.,1.),(1.,
1.),(1.,1.),(1.,1.),(1.,1.),(1.,1.),(1.,1.),(1.,1.),(1.,1.),(1.,1.),(1.,
1.),(1.,1.),(1.,1.),(1.,1.),(1.,1.),(1.,1.),(1.,1.),(1.,1.),(1.,1.),(1.,
1.),(1.,1.),(1.,1.),(1.,1.),(1.,1.),(1.,1.),(1.,1.),(1.,1.),(1.,1.),(1.,
1.),(1.,1.)))
REPRESENTATION_ITEM('')
SURFACE()
);
#96=(
BOUNDED_SURFACE()
B_SPLINE_SURFACE(5,1,((#45942,#45943),(#45944,#45945),(#45946,#45947),(#45948,
#45949),(#45950,#45951),(#45952,#45953),(#45954,#45955),(#45956,#45957),
(#45958,#45959),(#45960,#45961),(#45962,#45963),(#45964,#45965),(#45966,
#45967),(#45968,#45969),(#45970,#45971),(#45972,#45973),(#45974,#45975),
(#45976,#45977),(#45978,#45979),(#45980,#45981),(#45982,#45983),(#45984,
#45985),(#45986,#45987),(#45988,#45989),(#45990,#45991),(#45992,#45993),
(#45994,#45995),(#45996,#45997),(#45998,#45999),(#46000,#46001),(#46002,
#46003),(#46004,#46005),(#46006,#46007),(#46008,#46009),(#46010,#46011),
(#46012,#46013),(#46014,#46015),(#46016,#46017),(#46018,#46019),(#46020,
#46021),(#46022,#46023),(#46024,#46025),(#46026,#46027),(#46028,#46029),
(#46030,#46031),(#46032,#46033),(#46034,#46035),(#46036,#46037),(#46038,
#46039),(#46040,#46041),(#46042,#46043),(#46044,#46045),(#46046,#46047),
(#46048,#46049),(#46050,#46051),(#46052,#46053),(#46054,#46055),(#46056,
#46057),(#46058,#46059),(#46060,#46061),(#46062,#46063),(#46064,#46065),
(#46066,#46067),(#46068,#46069),(#46070,#46071),(#46072,#46073),(#46074,
#46075),(#46076,#46077),(#46078,#46079),(#46080,#46081)),.UNSPECIFIED.,
 .F.,.F.,.F.)
B_SPLINE_SURFACE_WITH_KNOTS((6,1,1,1,1,1,1,1,1,1,1,1,1,1,1,1,1,1,1,1,1,
1,1,1,1,1,1,1,1,1,1,1,1,1,1,1,1,1,1,1,1,1,1,1,1,1,1,1,1,1,1,1,1,1,1,1,1,
1,1,1,1,1,1,1,1,6),(2,2),(-1.,-0.984615384615383,-0.969230769230768,-0.953846153846152,
-0.938461538461537,-0.923076923076922,-0.907692307692306,-0.892307692307691,
-0.876923076923076,-0.86153846153846,-0.846153846153845,-0.83076923076923,
-0.815384615384614,-0.799999999999999,-0.784615384615384,-0.769230769230768,
-0.753846153846153,-0.738461538461538,-0.723076923076922,-0.707692307692307,
-0.692307692307692,-0.676923076923076,-0.661538461538461,-0.646153846153846,
-0.63076923076923,-0.615384615384615,-0.6,-0.584615384615384,-0.569230769230769,
-0.553846153846154,-0.538461538461538,-0.523076923076923,-0.507692307692308,
-0.492307692307692,-0.476923076923077,-0.461538461538462,-0.446153846153846,
-0.430769230769231,-0.415384615384615,-0.4,-0.384615384615385,-0.369230769230769,
-0.353846153846154,-0.338461538461538,-0.323076923076923,-0.307692307692308,
-0.292307692307692,-0.276923076923077,-0.261538461538462,-0.246153846153846,
-0.230769230769231,-0.215384615384615,-0.2,-0.184615384615385,-0.169230769230769,
-0.153846153846154,-0.138461538461538,-0.123076923076923,-0.107692307692308,
-0.0923076923076923,-0.0769230769230769,-0.0615384615384615,-0.0461538461538462,
-0.0307692307692308,-0.0153846153846154,0.),(-1.,1.),.UNSPECIFIED.)
GEOMETRIC_REPRESENTATION_ITEM()
RATIONAL_B_SPLINE_SURFACE(((1.,1.),(1.,1.),(1.,1.),(1.,1.),(1.,1.),(1.,
1.),(1.,1.),(1.,1.),(1.,1.),(1.,1.),(1.,1.),(1.,1.),(1.,1.),(1.,1.),(1.,
1.),(1.,1.),(1.,1.),(1.,1.),(1.,1.),(1.,1.),(1.,1.),(1.,1.),(1.,1.),(1.,
1.),(1.,1.),(1.,1.),(1.,1.),(1.,1.),(1.,1.),(1.,1.),(1.,1.),(1.,1.),(1.,
1.),(1.,1.),(1.,1.),(1.,1.),(1.,1.),(1.,1.),(1.,1.),(1.,1.),(1.,1.),(1.,
1.),(1.,1.),(1.,1.),(1.,1.),(1.,1.),(1.,1.),(1.,1.),(1.,1.),(1.,1.),(1.,
1.),(1.,1.),(1.,1.),(1.,1.),(1.,1.),(1.,1.),(1.,1.),(1.,1.),(1.,1.),(1.,
1.),(1.,1.),(1.,1.),(1.,1.),(1.,1.),(1.,1.),(1.,1.),(1.,1.),(1.,1.),(1.,
1.),(1.,1.)))
REPRESENTATION_ITEM('')
SURFACE()
);
#97=(
BOUNDED_SURFACE()
B_SPLINE_SURFACE(5,1,((#46172,#46173),(#46174,#46175),(#46176,#46177),(#46178,
#46179),(#46180,#46181),(#46182,#46183),(#46184,#46185),(#46186,#46187),
(#46188,#46189),(#46190,#46191),(#46192,#46193),(#46194,#46195),(#46196,
#46197),(#46198,#46199),(#46200,#46201),(#46202,#46203),(#46204,#46205),
(#46206,#46207),(#46208,#46209),(#46210,#46211),(#46212,#46213),(#46214,
#46215),(#46216,#46217),(#46218,#46219),(#46220,#46221),(#46222,#46223),
(#46224,#46225),(#46226,#46227),(#46228,#46229),(#46230,#46231),(#46232,
#46233),(#46234,#46235),(#46236,#46237),(#46238,#46239),(#46240,#46241),
(#46242,#46243),(#46244,#46245),(#46246,#46247),(#46248,#46249),(#46250,
#46251),(#46252,#46253),(#46254,#46255),(#46256,#46257),(#46258,#46259),
(#46260,#46261),(#46262,#46263),(#46264,#46265),(#46266,#46267),(#46268,
#46269),(#46270,#46271),(#46272,#46273),(#46274,#46275),(#46276,#46277),
(#46278,#46279),(#46280,#46281),(#46282,#46283),(#46284,#46285),(#46286,
#46287),(#46288,#46289),(#46290,#46291),(#46292,#46293),(#46294,#46295),
(#46296,#46297),(#46298,#46299),(#46300,#46301),(#46302,#46303),(#46304,
#46305),(#46306,#46307),(#46308,#46309),(#46310,#46311)),.UNSPECIFIED.,
 .F.,.F.,.F.)
B_SPLINE_SURFACE_WITH_KNOTS((6,1,1,1,1,1,1,1,1,1,1,1,1,1,1,1,1,1,1,1,1,
1,1,1,1,1,1,1,1,1,1,1,1,1,1,1,1,1,1,1,1,1,1,1,1,1,1,1,1,1,1,1,1,1,1,1,1,
1,1,1,1,1,1,1,1,6),(2,2),(-1.,-0.984615384615383,-0.969230769230768,-0.953846153846152,
-0.938461538461537,-0.923076923076922,-0.907692307692306,-0.892307692307691,
-0.876923076923076,-0.86153846153846,-0.846153846153845,-0.83076923076923,
-0.815384615384614,-0.799999999999999,-0.784615384615384,-0.769230769230768,
-0.753846153846153,-0.738461538461538,-0.723076923076922,-0.707692307692307,
-0.692307692307692,-0.676923076923076,-0.661538461538461,-0.646153846153846,
-0.63076923076923,-0.615384615384615,-0.6,-0.584615384615384,-0.569230769230769,
-0.553846153846154,-0.538461538461538,-0.523076923076923,-0.507692307692308,
-0.492307692307692,-0.476923076923077,-0.461538461538462,-0.446153846153846,
-0.430769230769231,-0.415384615384615,-0.4,-0.384615384615385,-0.369230769230769,
-0.353846153846154,-0.338461538461538,-0.323076923076923,-0.307692307692308,
-0.292307692307692,-0.276923076923077,-0.261538461538462,-0.246153846153846,
-0.230769230769231,-0.215384615384615,-0.2,-0.184615384615385,-0.169230769230769,
-0.153846153846154,-0.138461538461538,-0.123076923076923,-0.107692307692308,
-0.0923076923076923,-0.0769230769230769,-0.0615384615384615,-0.0461538461538462,
-0.0307692307692308,-0.0153846153846154,0.),(-1.,1.),.UNSPECIFIED.)
GEOMETRIC_REPRESENTATION_ITEM()
RATIONAL_B_SPLINE_SURFACE(((1.,1.),(1.,1.),(1.,1.),(1.,1.),(1.,1.),(1.,
1.),(1.,1.),(1.,1.),(1.,1.),(1.,1.),(1.,1.),(1.,1.),(1.,1.),(1.,1.),(1.,
1.),(1.,1.),(1.,1.),(1.,1.),(1.,1.),(1.,1.),(1.,1.),(1.,1.),(1.,1.),(1.,
1.),(1.,1.),(1.,1.),(1.,1.),(1.,1.),(1.,1.),(1.,1.),(1.,1.),(1.,1.),(1.,
1.),(1.,1.),(1.,1.),(1.,1.),(1.,1.),(1.,1.),(1.,1.),(1.,1.),(1.,1.),(1.,
1.),(1.,1.),(1.,1.),(1.,1.),(1.,1.),(1.,1.),(1.,1.),(1.,1.),(1.,1.),(1.,
1.),(1.,1.),(1.,1.),(1.,1.),(1.,1.),(1.,1.),(1.,1.),(1.,1.),(1.,1.),(1.,
1.),(1.,1.),(1.,1.),(1.,1.),(1.,1.),(1.,1.),(1.,1.),(1.,1.),(1.,1.),(1.,
1.),(1.,1.)))
REPRESENTATION_ITEM('')
SURFACE()
);
#98=(
BOUNDED_SURFACE()
B_SPLINE_SURFACE(5,1,((#46384,#46385),(#46386,#46387),(#46388,#46389),(#46390,
#46391),(#46392,#46393),(#46394,#46395),(#46396,#46397),(#46398,#46399),
(#46400,#46401),(#46402,#46403),(#46404,#46405),(#46406,#46407),(#46408,
#46409),(#46410,#46411),(#46412,#46413),(#46414,#46415),(#46416,#46417),
(#46418,#46419),(#46420,#46421),(#46422,#46423),(#46424,#46425),(#46426,
#46427),(#46428,#46429),(#46430,#46431),(#46432,#46433),(#46434,#46435),
(#46436,#46437),(#46438,#46439),(#46440,#46441),(#46442,#46443),(#46444,
#46445),(#46446,#46447),(#46448,#46449),(#46450,#46451),(#46452,#46453),
(#46454,#46455),(#46456,#46457),(#46458,#46459),(#46460,#46461),(#46462,
#46463),(#46464,#46465),(#46466,#46467),(#46468,#46469),(#46470,#46471),
(#46472,#46473),(#46474,#46475),(#46476,#46477),(#46478,#46479),(#46480,
#46481),(#46482,#46483),(#46484,#46485),(#46486,#46487),(#46488,#46489),
(#46490,#46491),(#46492,#46493),(#46494,#46495),(#46496,#46497),(#46498,
#46499),(#46500,#46501),(#46502,#46503),(#46504,#46505),(#46506,#46507),
(#46508,#46509),(#46510,#46511),(#46512,#46513),(#46514,#46515),(#46516,
#46517),(#46518,#46519),(#46520,#46521),(#46522,#46523)),.UNSPECIFIED.,
 .F.,.F.,.F.)
B_SPLINE_SURFACE_WITH_KNOTS((6,1,1,1,1,1,1,1,1,1,1,1,1,1,1,1,1,1,1,1,1,
1,1,1,1,1,1,1,1,1,1,1,1,1,1,1,1,1,1,1,1,1,1,1,1,1,1,1,1,1,1,1,1,1,1,1,1,
1,1,1,1,1,1,1,1,6),(2,2),(-1.,-0.984615384615383,-0.969230769230768,-0.953846153846152,
-0.938461538461537,-0.923076923076922,-0.907692307692306,-0.892307692307691,
-0.876923076923076,-0.86153846153846,-0.846153846153845,-0.83076923076923,
-0.815384615384614,-0.799999999999999,-0.784615384615384,-0.769230769230768,
-0.753846153846153,-0.738461538461538,-0.723076923076922,-0.707692307692307,
-0.692307692307692,-0.676923076923076,-0.661538461538461,-0.646153846153846,
-0.63076923076923,-0.615384615384615,-0.6,-0.584615384615384,-0.569230769230769,
-0.553846153846154,-0.538461538461538,-0.523076923076923,-0.507692307692308,
-0.492307692307692,-0.476923076923077,-0.461538461538462,-0.446153846153846,
-0.430769230769231,-0.415384615384615,-0.4,-0.384615384615385,-0.369230769230769,
-0.353846153846154,-0.338461538461538,-0.323076923076923,-0.307692307692308,
-0.292307692307692,-0.276923076923077,-0.261538461538462,-0.246153846153846,
-0.230769230769231,-0.215384615384615,-0.2,-0.184615384615385,-0.169230769230769,
-0.153846153846154,-0.138461538461538,-0.123076923076923,-0.107692307692308,
-0.0923076923076923,-0.0769230769230769,-0.0615384615384615,-0.0461538461538462,
-0.0307692307692308,-0.0153846153846154,0.),(-1.,1.),.UNSPECIFIED.)
GEOMETRIC_REPRESENTATION_ITEM()
RATIONAL_B_SPLINE_SURFACE(((1.,1.),(1.,1.),(1.,1.),(1.,1.),(1.,1.),(1.,
1.),(1.,1.),(1.,1.),(1.,1.),(1.,1.),(1.,1.),(1.,1.),(1.,1.),(1.,1.),(1.,
1.),(1.,1.),(1.,1.),(1.,1.),(1.,1.),(1.,1.),(1.,1.),(1.,1.),(1.,1.),(1.,
1.),(1.,1.),(1.,1.),(1.,1.),(1.,1.),(1.,1.),(1.,1.),(1.,1.),(1.,1.),(1.,
1.),(1.,1.),(1.,1.),(1.,1.),(1.,1.),(1.,1.),(1.,1.),(1.,1.),(1.,1.),(1.,
1.),(1.,1.),(1.,1.),(1.,1.),(1.,1.),(1.,1.),(1.,1.),(1.,1.),(1.,1.),(1.,
1.),(1.,1.),(1.,1.),(1.,1.),(1.,1.),(1.,1.),(1.,1.),(1.,1.),(1.,1.),(1.,
1.),(1.,1.),(1.,1.),(1.,1.),(1.,1.),(1.,1.),(1.,1.),(1.,1.),(1.,1.),(1.,
1.),(1.,1.)))
REPRESENTATION_ITEM('')
SURFACE()
);
#99=(
BOUNDED_SURFACE()
B_SPLINE_SURFACE(5,1,((#46614,#46615),(#46616,#46617),(#46618,#46619),(#46620,
#46621),(#46622,#46623),(#46624,#46625),(#46626,#46627),(#46628,#46629),
(#46630,#46631),(#46632,#46633),(#46634,#46635),(#46636,#46637),(#46638,
#46639),(#46640,#46641),(#46642,#46643),(#46644,#46645),(#46646,#46647),
(#46648,#46649),(#46650,#46651),(#46652,#46653),(#46654,#46655),(#46656,
#46657),(#46658,#46659),(#46660,#46661),(#46662,#46663),(#46664,#46665),
(#46666,#46667),(#46668,#46669),(#46670,#46671),(#46672,#46673),(#46674,
#46675),(#46676,#46677),(#46678,#46679),(#46680,#46681),(#46682,#46683),
(#46684,#46685),(#46686,#46687),(#46688,#46689),(#46690,#46691),(#46692,
#46693),(#46694,#46695),(#46696,#46697),(#46698,#46699),(#46700,#46701),
(#46702,#46703),(#46704,#46705),(#46706,#46707),(#46708,#46709),(#46710,
#46711),(#46712,#46713),(#46714,#46715),(#46716,#46717),(#46718,#46719),
(#46720,#46721),(#46722,#46723),(#46724,#46725),(#46726,#46727),(#46728,
#46729),(#46730,#46731),(#46732,#46733),(#46734,#46735),(#46736,#46737),
(#46738,#46739),(#46740,#46741),(#46742,#46743),(#46744,#46745),(#46746,
#46747),(#46748,#46749),(#46750,#46751),(#46752,#46753)),.UNSPECIFIED.,
 .F.,.F.,.F.)
B_SPLINE_SURFACE_WITH_KNOTS((6,1,1,1,1,1,1,1,1,1,1,1,1,1,1,1,1,1,1,1,1,
1,1,1,1,1,1,1,1,1,1,1,1,1,1,1,1,1,1,1,1,1,1,1,1,1,1,1,1,1,1,1,1,1,1,1,1,
1,1,1,1,1,1,1,1,6),(2,2),(-1.,-0.984615384615383,-0.969230769230768,-0.953846153846152,
-0.938461538461537,-0.923076923076922,-0.907692307692306,-0.892307692307691,
-0.876923076923076,-0.86153846153846,-0.846153846153845,-0.83076923076923,
-0.815384615384614,-0.799999999999999,-0.784615384615384,-0.769230769230768,
-0.753846153846153,-0.738461538461538,-0.723076923076922,-0.707692307692307,
-0.692307692307692,-0.676923076923076,-0.661538461538461,-0.646153846153846,
-0.63076923076923,-0.615384615384615,-0.6,-0.584615384615384,-0.569230769230769,
-0.553846153846154,-0.538461538461538,-0.523076923076923,-0.507692307692308,
-0.492307692307692,-0.476923076923077,-0.461538461538462,-0.446153846153846,
-0.430769230769231,-0.415384615384615,-0.4,-0.384615384615385,-0.369230769230769,
-0.353846153846154,-0.338461538461538,-0.323076923076923,-0.307692307692308,
-0.292307692307692,-0.276923076923077,-0.261538461538462,-0.246153846153846,
-0.230769230769231,-0.215384615384615,-0.2,-0.184615384615385,-0.169230769230769,
-0.153846153846154,-0.138461538461538,-0.123076923076923,-0.107692307692308,
-0.0923076923076923,-0.0769230769230769,-0.0615384615384615,-0.0461538461538462,
-0.0307692307692308,-0.0153846153846154,0.),(-1.,1.),.UNSPECIFIED.)
GEOMETRIC_REPRESENTATION_ITEM()
RATIONAL_B_SPLINE_SURFACE(((1.,1.),(1.,1.),(1.,1.),(1.,1.),(1.,1.),(1.,
1.),(1.,1.),(1.,1.),(1.,1.),(1.,1.),(1.,1.),(1.,1.),(1.,1.),(1.,1.),(1.,
1.),(1.,1.),(1.,1.),(1.,1.),(1.,1.),(1.,1.),(1.,1.),(1.,1.),(1.,1.),(1.,
1.),(1.,1.),(1.,1.),(1.,1.),(1.,1.),(1.,1.),(1.,1.),(1.,1.),(1.,1.),(1.,
1.),(1.,1.),(1.,1.),(1.,1.),(1.,1.),(1.,1.),(1.,1.),(1.,1.),(1.,1.),(1.,
1.),(1.,1.),(1.,1.),(1.,1.),(1.,1.),(1.,1.),(1.,1.),(1.,1.),(1.,1.),(1.,
1.),(1.,1.),(1.,1.),(1.,1.),(1.,1.),(1.,1.),(1.,1.),(1.,1.),(1.,1.),(1.,
1.),(1.,1.),(1.,1.),(1.,1.),(1.,1.),(1.,1.),(1.,1.),(1.,1.),(1.,1.),(1.,
1.),(1.,1.)))
REPRESENTATION_ITEM('')
SURFACE()
);
#100=(
BOUNDED_SURFACE()
B_SPLINE_SURFACE(5,1,((#46826,#46827),(#46828,#46829),(#46830,#46831),(#46832,
#46833),(#46834,#46835),(#46836,#46837),(#46838,#46839),(#46840,#46841),
(#46842,#46843),(#46844,#46845),(#46846,#46847),(#46848,#46849),(#46850,
#46851),(#46852,#46853),(#46854,#46855),(#46856,#46857),(#46858,#46859),
(#46860,#46861),(#46862,#46863),(#46864,#46865),(#46866,#46867),(#46868,
#46869),(#46870,#46871),(#46872,#46873),(#46874,#46875),(#46876,#46877),
(#46878,#46879),(#46880,#46881),(#46882,#46883),(#46884,#46885),(#46886,
#46887),(#46888,#46889),(#46890,#46891),(#46892,#46893),(#46894,#46895),
(#46896,#46897),(#46898,#46899),(#46900,#46901),(#46902,#46903),(#46904,
#46905),(#46906,#46907),(#46908,#46909),(#46910,#46911),(#46912,#46913),
(#46914,#46915),(#46916,#46917),(#46918,#46919),(#46920,#46921),(#46922,
#46923),(#46924,#46925),(#46926,#46927),(#46928,#46929),(#46930,#46931),
(#46932,#46933),(#46934,#46935),(#46936,#46937),(#46938,#46939),(#46940,
#46941),(#46942,#46943),(#46944,#46945),(#46946,#46947),(#46948,#46949),
(#46950,#46951),(#46952,#46953),(#46954,#46955),(#46956,#46957),(#46958,
#46959),(#46960,#46961),(#46962,#46963),(#46964,#46965)),.UNSPECIFIED.,
 .F.,.F.,.F.)
B_SPLINE_SURFACE_WITH_KNOTS((6,1,1,1,1,1,1,1,1,1,1,1,1,1,1,1,1,1,1,1,1,
1,1,1,1,1,1,1,1,1,1,1,1,1,1,1,1,1,1,1,1,1,1,1,1,1,1,1,1,1,1,1,1,1,1,1,1,
1,1,1,1,1,1,1,1,6),(2,2),(-1.,-0.984615384615383,-0.969230769230768,-0.953846153846152,
-0.938461538461537,-0.923076923076922,-0.907692307692306,-0.892307692307691,
-0.876923076923076,-0.86153846153846,-0.846153846153845,-0.83076923076923,
-0.815384615384614,-0.799999999999999,-0.784615384615384,-0.769230769230768,
-0.753846153846153,-0.738461538461538,-0.723076923076922,-0.707692307692307,
-0.692307692307692,-0.676923076923076,-0.661538461538461,-0.646153846153846,
-0.63076923076923,-0.615384615384615,-0.6,-0.584615384615384,-0.569230769230769,
-0.553846153846154,-0.538461538461538,-0.523076923076923,-0.507692307692308,
-0.492307692307692,-0.476923076923077,-0.461538461538462,-0.446153846153846,
-0.430769230769231,-0.415384615384615,-0.4,-0.384615384615385,-0.369230769230769,
-0.353846153846154,-0.338461538461538,-0.323076923076923,-0.307692307692308,
-0.292307692307692,-0.276923076923077,-0.261538461538462,-0.246153846153846,
-0.230769230769231,-0.215384615384615,-0.2,-0.184615384615385,-0.169230769230769,
-0.153846153846154,-0.138461538461538,-0.123076923076923,-0.107692307692308,
-0.0923076923076923,-0.0769230769230769,-0.0615384615384615,-0.0461538461538462,
-0.0307692307692308,-0.0153846153846154,0.),(-1.,1.),.UNSPECIFIED.)
GEOMETRIC_REPRESENTATION_ITEM()
RATIONAL_B_SPLINE_SURFACE(((1.,1.),(1.,1.),(1.,1.),(1.,1.),(1.,1.),(1.,
1.),(1.,1.),(1.,1.),(1.,1.),(1.,1.),(1.,1.),(1.,1.),(1.,1.),(1.,1.),(1.,
1.),(1.,1.),(1.,1.),(1.,1.),(1.,1.),(1.,1.),(1.,1.),(1.,1.),(1.,1.),(1.,
1.),(1.,1.),(1.,1.),(1.,1.),(1.,1.),(1.,1.),(1.,1.),(1.,1.),(1.,1.),(1.,
1.),(1.,1.),(1.,1.),(1.,1.),(1.,1.),(1.,1.),(1.,1.),(1.,1.),(1.,1.),(1.,
1.),(1.,1.),(1.,1.),(1.,1.),(1.,1.),(1.,1.),(1.,1.),(1.,1.),(1.,1.),(1.,
1.),(1.,1.),(1.,1.),(1.,1.),(1.,1.),(1.,1.),(1.,1.),(1.,1.),(1.,1.),(1.,
1.),(1.,1.),(1.,1.),(1.,1.),(1.,1.),(1.,1.),(1.,1.),(1.,1.),(1.,1.),(1.,
1.),(1.,1.)))
REPRESENTATION_ITEM('')
SURFACE()
);
#101=(
BOUNDED_SURFACE()
B_SPLINE_SURFACE(5,1,((#47056,#47057),(#47058,#47059),(#47060,#47061),(#47062,
#47063),(#47064,#47065),(#47066,#47067),(#47068,#47069),(#47070,#47071),
(#47072,#47073),(#47074,#47075),(#47076,#47077),(#47078,#47079),(#47080,
#47081),(#47082,#47083),(#47084,#47085),(#47086,#47087),(#47088,#47089),
(#47090,#47091),(#47092,#47093),(#47094,#47095),(#47096,#47097),(#47098,
#47099),(#47100,#47101),(#47102,#47103),(#47104,#47105),(#47106,#47107),
(#47108,#47109),(#47110,#47111),(#47112,#47113),(#47114,#47115),(#47116,
#47117),(#47118,#47119),(#47120,#47121),(#47122,#47123),(#47124,#47125),
(#47126,#47127),(#47128,#47129),(#47130,#47131),(#47132,#47133),(#47134,
#47135),(#47136,#47137),(#47138,#47139),(#47140,#47141),(#47142,#47143),
(#47144,#47145),(#47146,#47147),(#47148,#47149),(#47150,#47151),(#47152,
#47153),(#47154,#47155),(#47156,#47157),(#47158,#47159),(#47160,#47161),
(#47162,#47163),(#47164,#47165),(#47166,#47167),(#47168,#47169),(#47170,
#47171),(#47172,#47173),(#47174,#47175),(#47176,#47177),(#47178,#47179),
(#47180,#47181),(#47182,#47183),(#47184,#47185),(#47186,#47187),(#47188,
#47189),(#47190,#47191),(#47192,#47193),(#47194,#47195)),.UNSPECIFIED.,
 .F.,.F.,.F.)
B_SPLINE_SURFACE_WITH_KNOTS((6,1,1,1,1,1,1,1,1,1,1,1,1,1,1,1,1,1,1,1,1,
1,1,1,1,1,1,1,1,1,1,1,1,1,1,1,1,1,1,1,1,1,1,1,1,1,1,1,1,1,1,1,1,1,1,1,1,
1,1,1,1,1,1,1,1,6),(2,2),(-1.,-0.984615384615383,-0.969230769230768,-0.953846153846152,
-0.938461538461537,-0.923076923076922,-0.907692307692306,-0.892307692307691,
-0.876923076923076,-0.86153846153846,-0.846153846153845,-0.83076923076923,
-0.815384615384614,-0.799999999999999,-0.784615384615384,-0.769230769230768,
-0.753846153846153,-0.738461538461538,-0.723076923076922,-0.707692307692307,
-0.692307692307692,-0.676923076923076,-0.661538461538461,-0.646153846153846,
-0.63076923076923,-0.615384615384615,-0.6,-0.584615384615384,-0.569230769230769,
-0.553846153846154,-0.538461538461538,-0.523076923076923,-0.507692307692308,
-0.492307692307692,-0.476923076923077,-0.461538461538462,-0.446153846153846,
-0.430769230769231,-0.415384615384615,-0.4,-0.384615384615385,-0.369230769230769,
-0.353846153846154,-0.338461538461538,-0.323076923076923,-0.307692307692308,
-0.292307692307692,-0.276923076923077,-0.261538461538462,-0.246153846153846,
-0.230769230769231,-0.215384615384615,-0.2,-0.184615384615385,-0.169230769230769,
-0.153846153846154,-0.138461538461538,-0.123076923076923,-0.107692307692308,
-0.0923076923076923,-0.0769230769230769,-0.0615384615384615,-0.0461538461538462,
-0.0307692307692308,-0.0153846153846154,0.),(-1.,1.),.UNSPECIFIED.)
GEOMETRIC_REPRESENTATION_ITEM()
RATIONAL_B_SPLINE_SURFACE(((1.,1.),(1.,1.),(1.,1.),(1.,1.),(1.,1.),(1.,
1.),(1.,1.),(1.,1.),(1.,1.),(1.,1.),(1.,1.),(1.,1.),(1.,1.),(1.,1.),(1.,
1.),(1.,1.),(1.,1.),(1.,1.),(1.,1.),(1.,1.),(1.,1.),(1.,1.),(1.,1.),(1.,
1.),(1.,1.),(1.,1.),(1.,1.),(1.,1.),(1.,1.),(1.,1.),(1.,1.),(1.,1.),(1.,
1.),(1.,1.),(1.,1.),(1.,1.),(1.,1.),(1.,1.),(1.,1.),(1.,1.),(1.,1.),(1.,
1.),(1.,1.),(1.,1.),(1.,1.),(1.,1.),(1.,1.),(1.,1.),(1.,1.),(1.,1.),(1.,
1.),(1.,1.),(1.,1.),(1.,1.),(1.,1.),(1.,1.),(1.,1.),(1.,1.),(1.,1.),(1.,
1.),(1.,1.),(1.,1.),(1.,1.),(1.,1.),(1.,1.),(1.,1.),(1.,1.),(1.,1.),(1.,
1.),(1.,1.)))
REPRESENTATION_ITEM('')
SURFACE()
);
#102=(
BOUNDED_SURFACE()
B_SPLINE_SURFACE(5,1,((#47268,#47269),(#47270,#47271),(#47272,#47273),(#47274,
#47275),(#47276,#47277),(#47278,#47279),(#47280,#47281),(#47282,#47283),
(#47284,#47285),(#47286,#47287),(#47288,#47289),(#47290,#47291),(#47292,
#47293),(#47294,#47295),(#47296,#47297),(#47298,#47299),(#47300,#47301),
(#47302,#47303),(#47304,#47305),(#47306,#47307),(#47308,#47309),(#47310,
#47311),(#47312,#47313),(#47314,#47315),(#47316,#47317),(#47318,#47319),
(#47320,#47321),(#47322,#47323),(#47324,#47325),(#47326,#47327),(#47328,
#47329),(#47330,#47331),(#47332,#47333),(#47334,#47335),(#47336,#47337),
(#47338,#47339),(#47340,#47341),(#47342,#47343),(#47344,#47345),(#47346,
#47347),(#47348,#47349),(#47350,#47351),(#47352,#47353),(#47354,#47355),
(#47356,#47357),(#47358,#47359),(#47360,#47361),(#47362,#47363),(#47364,
#47365),(#47366,#47367),(#47368,#47369),(#47370,#47371),(#47372,#47373),
(#47374,#47375),(#47376,#47377),(#47378,#47379),(#47380,#47381),(#47382,
#47383),(#47384,#47385),(#47386,#47387),(#47388,#47389),(#47390,#47391),
(#47392,#47393),(#47394,#47395),(#47396,#47397),(#47398,#47399),(#47400,
#47401),(#47402,#47403),(#47404,#47405),(#47406,#47407)),.UNSPECIFIED.,
 .F.,.F.,.F.)
B_SPLINE_SURFACE_WITH_KNOTS((6,1,1,1,1,1,1,1,1,1,1,1,1,1,1,1,1,1,1,1,1,
1,1,1,1,1,1,1,1,1,1,1,1,1,1,1,1,1,1,1,1,1,1,1,1,1,1,1,1,1,1,1,1,1,1,1,1,
1,1,1,1,1,1,1,1,6),(2,2),(-1.,-0.984615384615383,-0.969230769230768,-0.953846153846152,
-0.938461538461537,-0.923076923076922,-0.907692307692306,-0.892307692307691,
-0.876923076923076,-0.86153846153846,-0.846153846153845,-0.83076923076923,
-0.815384615384614,-0.799999999999999,-0.784615384615384,-0.769230769230768,
-0.753846153846153,-0.738461538461538,-0.723076923076922,-0.707692307692307,
-0.692307692307692,-0.676923076923076,-0.661538461538461,-0.646153846153846,
-0.63076923076923,-0.615384615384615,-0.6,-0.584615384615384,-0.569230769230769,
-0.553846153846154,-0.538461538461538,-0.523076923076923,-0.507692307692308,
-0.492307692307692,-0.476923076923077,-0.461538461538462,-0.446153846153846,
-0.430769230769231,-0.415384615384615,-0.4,-0.384615384615385,-0.369230769230769,
-0.353846153846154,-0.338461538461538,-0.323076923076923,-0.307692307692308,
-0.292307692307692,-0.276923076923077,-0.261538461538462,-0.246153846153846,
-0.230769230769231,-0.215384615384615,-0.2,-0.184615384615385,-0.169230769230769,
-0.153846153846154,-0.138461538461538,-0.123076923076923,-0.107692307692308,
-0.0923076923076923,-0.0769230769230769,-0.0615384615384615,-0.0461538461538462,
-0.0307692307692308,-0.0153846153846154,0.),(-1.,1.),.UNSPECIFIED.)
GEOMETRIC_REPRESENTATION_ITEM()
RATIONAL_B_SPLINE_SURFACE(((1.,1.),(1.,1.),(1.,1.),(1.,1.),(1.,1.),(1.,
1.),(1.,1.),(1.,1.),(1.,1.),(1.,1.),(1.,1.),(1.,1.),(1.,1.),(1.,1.),(1.,
1.),(1.,1.),(1.,1.),(1.,1.),(1.,1.),(1.,1.),(1.,1.),(1.,1.),(1.,1.),(1.,
1.),(1.,1.),(1.,1.),(1.,1.),(1.,1.),(1.,1.),(1.,1.),(1.,1.),(1.,1.),(1.,
1.),(1.,1.),(1.,1.),(1.,1.),(1.,1.),(1.,1.),(1.,1.),(1.,1.),(1.,1.),(1.,
1.),(1.,1.),(1.,1.),(1.,1.),(1.,1.),(1.,1.),(1.,1.),(1.,1.),(1.,1.),(1.,
1.),(1.,1.),(1.,1.),(1.,1.),(1.,1.),(1.,1.),(1.,1.),(1.,1.),(1.,1.),(1.,
1.),(1.,1.),(1.,1.),(1.,1.),(1.,1.),(1.,1.),(1.,1.),(1.,1.),(1.,1.),(1.,
1.),(1.,1.)))
REPRESENTATION_ITEM('')
SURFACE()
);
#103=(
BOUNDED_SURFACE()
B_SPLINE_SURFACE(5,1,((#47498,#47499),(#47500,#47501),(#47502,#47503),(#47504,
#47505),(#47506,#47507),(#47508,#47509),(#47510,#47511),(#47512,#47513),
(#47514,#47515),(#47516,#47517),(#47518,#47519),(#47520,#47521),(#47522,
#47523),(#47524,#47525),(#47526,#47527),(#47528,#47529),(#47530,#47531),
(#47532,#47533),(#47534,#47535),(#47536,#47537),(#47538,#47539),(#47540,
#47541),(#47542,#47543),(#47544,#47545),(#47546,#47547),(#47548,#47549),
(#47550,#47551),(#47552,#47553),(#47554,#47555),(#47556,#47557),(#47558,
#47559),(#47560,#47561),(#47562,#47563),(#47564,#47565),(#47566,#47567),
(#47568,#47569),(#47570,#47571),(#47572,#47573),(#47574,#47575),(#47576,
#47577),(#47578,#47579),(#47580,#47581),(#47582,#47583),(#47584,#47585),
(#47586,#47587),(#47588,#47589),(#47590,#47591),(#47592,#47593),(#47594,
#47595),(#47596,#47597),(#47598,#47599),(#47600,#47601),(#47602,#47603),
(#47604,#47605),(#47606,#47607),(#47608,#47609),(#47610,#47611),(#47612,
#47613),(#47614,#47615),(#47616,#47617),(#47618,#47619),(#47620,#47621),
(#47622,#47623),(#47624,#47625),(#47626,#47627),(#47628,#47629),(#47630,
#47631),(#47632,#47633),(#47634,#47635),(#47636,#47637)),.UNSPECIFIED.,
 .F.,.F.,.F.)
B_SPLINE_SURFACE_WITH_KNOTS((6,1,1,1,1,1,1,1,1,1,1,1,1,1,1,1,1,1,1,1,1,
1,1,1,1,1,1,1,1,1,1,1,1,1,1,1,1,1,1,1,1,1,1,1,1,1,1,1,1,1,1,1,1,1,1,1,1,
1,1,1,1,1,1,1,1,6),(2,2),(-1.,-0.984615384615383,-0.969230769230768,-0.953846153846152,
-0.938461538461537,-0.923076923076922,-0.907692307692306,-0.892307692307691,
-0.876923076923076,-0.86153846153846,-0.846153846153845,-0.83076923076923,
-0.815384615384614,-0.799999999999999,-0.784615384615384,-0.769230769230768,
-0.753846153846153,-0.738461538461538,-0.723076923076922,-0.707692307692307,
-0.692307692307692,-0.676923076923076,-0.661538461538461,-0.646153846153846,
-0.63076923076923,-0.615384615384615,-0.6,-0.584615384615384,-0.569230769230769,
-0.553846153846154,-0.538461538461538,-0.523076923076923,-0.507692307692308,
-0.492307692307692,-0.476923076923077,-0.461538461538462,-0.446153846153846,
-0.430769230769231,-0.415384615384615,-0.4,-0.384615384615385,-0.369230769230769,
-0.353846153846154,-0.338461538461538,-0.323076923076923,-0.307692307692308,
-0.292307692307692,-0.276923076923077,-0.261538461538462,-0.246153846153846,
-0.230769230769231,-0.215384615384615,-0.2,-0.184615384615385,-0.169230769230769,
-0.153846153846154,-0.138461538461538,-0.123076923076923,-0.107692307692308,
-0.0923076923076923,-0.0769230769230769,-0.0615384615384615,-0.0461538461538462,
-0.0307692307692308,-0.0153846153846154,0.),(-1.,1.),.UNSPECIFIED.)
GEOMETRIC_REPRESENTATION_ITEM()
RATIONAL_B_SPLINE_SURFACE(((1.,1.),(1.,1.),(1.,1.),(1.,1.),(1.,1.),(1.,
1.),(1.,1.),(1.,1.),(1.,1.),(1.,1.),(1.,1.),(1.,1.),(1.,1.),(1.,1.),(1.,
1.),(1.,1.),(1.,1.),(1.,1.),(1.,1.),(1.,1.),(1.,1.),(1.,1.),(1.,1.),(1.,
1.),(1.,1.),(1.,1.),(1.,1.),(1.,1.),(1.,1.),(1.,1.),(1.,1.),(1.,1.),(1.,
1.),(1.,1.),(1.,1.),(1.,1.),(1.,1.),(1.,1.),(1.,1.),(1.,1.),(1.,1.),(1.,
1.),(1.,1.),(1.,1.),(1.,1.),(1.,1.),(1.,1.),(1.,1.),(1.,1.),(1.,1.),(1.,
1.),(1.,1.),(1.,1.),(1.,1.),(1.,1.),(1.,1.),(1.,1.),(1.,1.),(1.,1.),(1.,
1.),(1.,1.),(1.,1.),(1.,1.),(1.,1.),(1.,1.),(1.,1.),(1.,1.),(1.,1.),(1.,
1.),(1.,1.)))
REPRESENTATION_ITEM('')
SURFACE()
);
#104=(
BOUNDED_SURFACE()
B_SPLINE_SURFACE(5,1,((#47710,#47711),(#47712,#47713),(#47714,#47715),(#47716,
#47717),(#47718,#47719),(#47720,#47721),(#47722,#47723),(#47724,#47725),
(#47726,#47727),(#47728,#47729),(#47730,#47731),(#47732,#47733),(#47734,
#47735),(#47736,#47737),(#47738,#47739),(#47740,#47741),(#47742,#47743),
(#47744,#47745),(#47746,#47747),(#47748,#47749),(#47750,#47751),(#47752,
#47753),(#47754,#47755),(#47756,#47757),(#47758,#47759),(#47760,#47761),
(#47762,#47763),(#47764,#47765),(#47766,#47767),(#47768,#47769),(#47770,
#47771),(#47772,#47773),(#47774,#47775),(#47776,#47777),(#47778,#47779),
(#47780,#47781),(#47782,#47783),(#47784,#47785),(#47786,#47787),(#47788,
#47789),(#47790,#47791),(#47792,#47793),(#47794,#47795),(#47796,#47797),
(#47798,#47799),(#47800,#47801),(#47802,#47803),(#47804,#47805),(#47806,
#47807),(#47808,#47809),(#47810,#47811),(#47812,#47813),(#47814,#47815),
(#47816,#47817),(#47818,#47819),(#47820,#47821),(#47822,#47823),(#47824,
#47825),(#47826,#47827),(#47828,#47829),(#47830,#47831),(#47832,#47833),
(#47834,#47835),(#47836,#47837),(#47838,#47839),(#47840,#47841),(#47842,
#47843),(#47844,#47845),(#47846,#47847),(#47848,#47849)),.UNSPECIFIED.,
 .F.,.F.,.F.)
B_SPLINE_SURFACE_WITH_KNOTS((6,1,1,1,1,1,1,1,1,1,1,1,1,1,1,1,1,1,1,1,1,
1,1,1,1,1,1,1,1,1,1,1,1,1,1,1,1,1,1,1,1,1,1,1,1,1,1,1,1,1,1,1,1,1,1,1,1,
1,1,1,1,1,1,1,1,6),(2,2),(-1.,-0.984615384615383,-0.969230769230768,-0.953846153846152,
-0.938461538461537,-0.923076923076922,-0.907692307692306,-0.892307692307691,
-0.876923076923076,-0.86153846153846,-0.846153846153845,-0.83076923076923,
-0.815384615384614,-0.799999999999999,-0.784615384615384,-0.769230769230768,
-0.753846153846153,-0.738461538461538,-0.723076923076922,-0.707692307692307,
-0.692307692307692,-0.676923076923076,-0.661538461538461,-0.646153846153846,
-0.63076923076923,-0.615384615384615,-0.6,-0.584615384615384,-0.569230769230769,
-0.553846153846154,-0.538461538461538,-0.523076923076923,-0.507692307692308,
-0.492307692307692,-0.476923076923077,-0.461538461538462,-0.446153846153846,
-0.430769230769231,-0.415384615384615,-0.4,-0.384615384615385,-0.369230769230769,
-0.353846153846154,-0.338461538461538,-0.323076923076923,-0.307692307692308,
-0.292307692307692,-0.276923076923077,-0.261538461538462,-0.246153846153846,
-0.230769230769231,-0.215384615384615,-0.2,-0.184615384615385,-0.169230769230769,
-0.153846153846154,-0.138461538461538,-0.123076923076923,-0.107692307692308,
-0.0923076923076923,-0.0769230769230769,-0.0615384615384615,-0.0461538461538462,
-0.0307692307692308,-0.0153846153846154,0.),(-1.,1.),.UNSPECIFIED.)
GEOMETRIC_REPRESENTATION_ITEM()
RATIONAL_B_SPLINE_SURFACE(((1.,1.),(1.,1.),(1.,1.),(1.,1.),(1.,1.),(1.,
1.),(1.,1.),(1.,1.),(1.,1.),(1.,1.),(1.,1.),(1.,1.),(1.,1.),(1.,1.),(1.,
1.),(1.,1.),(1.,1.),(1.,1.),(1.,1.),(1.,1.),(1.,1.),(1.,1.),(1.,1.),(1.,
1.),(1.,1.),(1.,1.),(1.,1.),(1.,1.),(1.,1.),(1.,1.),(1.,1.),(1.,1.),(1.,
1.),(1.,1.),(1.,1.),(1.,1.),(1.,1.),(1.,1.),(1.,1.),(1.,1.),(1.,1.),(1.,
1.),(1.,1.),(1.,1.),(1.,1.),(1.,1.),(1.,1.),(1.,1.),(1.,1.),(1.,1.),(1.,
1.),(1.,1.),(1.,1.),(1.,1.),(1.,1.),(1.,1.),(1.,1.),(1.,1.),(1.,1.),(1.,
1.),(1.,1.),(1.,1.),(1.,1.),(1.,1.),(1.,1.),(1.,1.),(1.,1.),(1.,1.),(1.,
1.),(1.,1.)))
REPRESENTATION_ITEM('')
SURFACE()
);
#105=(
BOUNDED_SURFACE()
B_SPLINE_SURFACE(5,1,((#47940,#47941),(#47942,#47943),(#47944,#47945),(#47946,
#47947),(#47948,#47949),(#47950,#47951),(#47952,#47953),(#47954,#47955),
(#47956,#47957),(#47958,#47959),(#47960,#47961),(#47962,#47963),(#47964,
#47965),(#47966,#47967),(#47968,#47969),(#47970,#47971),(#47972,#47973),
(#47974,#47975),(#47976,#47977),(#47978,#47979),(#47980,#47981),(#47982,
#47983),(#47984,#47985),(#47986,#47987),(#47988,#47989),(#47990,#47991),
(#47992,#47993),(#47994,#47995),(#47996,#47997),(#47998,#47999),(#48000,
#48001),(#48002,#48003),(#48004,#48005),(#48006,#48007),(#48008,#48009),
(#48010,#48011),(#48012,#48013),(#48014,#48015),(#48016,#48017),(#48018,
#48019),(#48020,#48021),(#48022,#48023),(#48024,#48025),(#48026,#48027),
(#48028,#48029),(#48030,#48031),(#48032,#48033),(#48034,#48035),(#48036,
#48037),(#48038,#48039),(#48040,#48041),(#48042,#48043),(#48044,#48045),
(#48046,#48047),(#48048,#48049),(#48050,#48051),(#48052,#48053),(#48054,
#48055),(#48056,#48057),(#48058,#48059),(#48060,#48061),(#48062,#48063),
(#48064,#48065),(#48066,#48067),(#48068,#48069),(#48070,#48071),(#48072,
#48073),(#48074,#48075),(#48076,#48077),(#48078,#48079)),.UNSPECIFIED.,
 .F.,.F.,.F.)
B_SPLINE_SURFACE_WITH_KNOTS((6,1,1,1,1,1,1,1,1,1,1,1,1,1,1,1,1,1,1,1,1,
1,1,1,1,1,1,1,1,1,1,1,1,1,1,1,1,1,1,1,1,1,1,1,1,1,1,1,1,1,1,1,1,1,1,1,1,
1,1,1,1,1,1,1,1,6),(2,2),(-1.,-0.984615384615383,-0.969230769230768,-0.953846153846152,
-0.938461538461537,-0.923076923076922,-0.907692307692306,-0.892307692307691,
-0.876923076923076,-0.86153846153846,-0.846153846153845,-0.83076923076923,
-0.815384615384614,-0.799999999999999,-0.784615384615384,-0.769230769230768,
-0.753846153846153,-0.738461538461538,-0.723076923076922,-0.707692307692307,
-0.692307692307692,-0.676923076923076,-0.661538461538461,-0.646153846153846,
-0.63076923076923,-0.615384615384615,-0.6,-0.584615384615384,-0.569230769230769,
-0.553846153846154,-0.538461538461538,-0.523076923076923,-0.507692307692308,
-0.492307692307692,-0.476923076923077,-0.461538461538462,-0.446153846153846,
-0.430769230769231,-0.415384615384615,-0.4,-0.384615384615385,-0.369230769230769,
-0.353846153846154,-0.338461538461538,-0.323076923076923,-0.307692307692308,
-0.292307692307692,-0.276923076923077,-0.261538461538462,-0.246153846153846,
-0.230769230769231,-0.215384615384615,-0.2,-0.184615384615385,-0.169230769230769,
-0.153846153846154,-0.138461538461538,-0.123076923076923,-0.107692307692308,
-0.0923076923076923,-0.0769230769230769,-0.0615384615384615,-0.0461538461538462,
-0.0307692307692308,-0.0153846153846154,0.),(-1.,1.),.UNSPECIFIED.)
GEOMETRIC_REPRESENTATION_ITEM()
RATIONAL_B_SPLINE_SURFACE(((1.,1.),(1.,1.),(1.,1.),(1.,1.),(1.,1.),(1.,
1.),(1.,1.),(1.,1.),(1.,1.),(1.,1.),(1.,1.),(1.,1.),(1.,1.),(1.,1.),(1.,
1.),(1.,1.),(1.,1.),(1.,1.),(1.,1.),(1.,1.),(1.,1.),(1.,1.),(1.,1.),(1.,
1.),(1.,1.),(1.,1.),(1.,1.),(1.,1.),(1.,1.),(1.,1.),(1.,1.),(1.,1.),(1.,
1.),(1.,1.),(1.,1.),(1.,1.),(1.,1.),(1.,1.),(1.,1.),(1.,1.),(1.,1.),(1.,
1.),(1.,1.),(1.,1.),(1.,1.),(1.,1.),(1.,1.),(1.,1.),(1.,1.),(1.,1.),(1.,
1.),(1.,1.),(1.,1.),(1.,1.),(1.,1.),(1.,1.),(1.,1.),(1.,1.),(1.,1.),(1.,
1.),(1.,1.),(1.,1.),(1.,1.),(1.,1.),(1.,1.),(1.,1.),(1.,1.),(1.,1.),(1.,
1.),(1.,1.)))
REPRESENTATION_ITEM('')
SURFACE()
);
#106=(
BOUNDED_SURFACE()
B_SPLINE_SURFACE(5,1,((#48152,#48153),(#48154,#48155),(#48156,#48157),(#48158,
#48159),(#48160,#48161),(#48162,#48163),(#48164,#48165),(#48166,#48167),
(#48168,#48169),(#48170,#48171),(#48172,#48173),(#48174,#48175),(#48176,
#48177),(#48178,#48179),(#48180,#48181),(#48182,#48183),(#48184,#48185),
(#48186,#48187),(#48188,#48189),(#48190,#48191),(#48192,#48193),(#48194,
#48195),(#48196,#48197),(#48198,#48199),(#48200,#48201),(#48202,#48203),
(#48204,#48205),(#48206,#48207),(#48208,#48209),(#48210,#48211),(#48212,
#48213),(#48214,#48215),(#48216,#48217),(#48218,#48219),(#48220,#48221),
(#48222,#48223),(#48224,#48225),(#48226,#48227),(#48228,#48229),(#48230,
#48231),(#48232,#48233),(#48234,#48235),(#48236,#48237),(#48238,#48239),
(#48240,#48241),(#48242,#48243),(#48244,#48245),(#48246,#48247),(#48248,
#48249),(#48250,#48251),(#48252,#48253),(#48254,#48255),(#48256,#48257),
(#48258,#48259),(#48260,#48261),(#48262,#48263),(#48264,#48265),(#48266,
#48267),(#48268,#48269),(#48270,#48271),(#48272,#48273),(#48274,#48275),
(#48276,#48277),(#48278,#48279),(#48280,#48281),(#48282,#48283),(#48284,
#48285),(#48286,#48287),(#48288,#48289),(#48290,#48291)),.UNSPECIFIED.,
 .F.,.F.,.F.)
B_SPLINE_SURFACE_WITH_KNOTS((6,1,1,1,1,1,1,1,1,1,1,1,1,1,1,1,1,1,1,1,1,
1,1,1,1,1,1,1,1,1,1,1,1,1,1,1,1,1,1,1,1,1,1,1,1,1,1,1,1,1,1,1,1,1,1,1,1,
1,1,1,1,1,1,1,1,6),(2,2),(-1.,-0.984615384615383,-0.969230769230768,-0.953846153846152,
-0.938461538461537,-0.923076923076922,-0.907692307692306,-0.892307692307691,
-0.876923076923076,-0.86153846153846,-0.846153846153845,-0.83076923076923,
-0.815384615384614,-0.799999999999999,-0.784615384615384,-0.769230769230768,
-0.753846153846153,-0.738461538461538,-0.723076923076922,-0.707692307692307,
-0.692307692307692,-0.676923076923076,-0.661538461538461,-0.646153846153846,
-0.63076923076923,-0.615384615384615,-0.6,-0.584615384615384,-0.569230769230769,
-0.553846153846154,-0.538461538461538,-0.523076923076923,-0.507692307692308,
-0.492307692307692,-0.476923076923077,-0.461538461538462,-0.446153846153846,
-0.430769230769231,-0.415384615384615,-0.4,-0.384615384615385,-0.369230769230769,
-0.353846153846154,-0.338461538461538,-0.323076923076923,-0.307692307692308,
-0.292307692307692,-0.276923076923077,-0.261538461538462,-0.246153846153846,
-0.230769230769231,-0.215384615384615,-0.2,-0.184615384615385,-0.169230769230769,
-0.153846153846154,-0.138461538461538,-0.123076923076923,-0.107692307692308,
-0.0923076923076923,-0.0769230769230769,-0.0615384615384615,-0.0461538461538462,
-0.0307692307692308,-0.0153846153846154,0.),(-1.,1.),.UNSPECIFIED.)
GEOMETRIC_REPRESENTATION_ITEM()
RATIONAL_B_SPLINE_SURFACE(((1.,1.),(1.,1.),(1.,1.),(1.,1.),(1.,1.),(1.,
1.),(1.,1.),(1.,1.),(1.,1.),(1.,1.),(1.,1.),(1.,1.),(1.,1.),(1.,1.),(1.,
1.),(1.,1.),(1.,1.),(1.,1.),(1.,1.),(1.,1.),(1.,1.),(1.,1.),(1.,1.),(1.,
1.),(1.,1.),(1.,1.),(1.,1.),(1.,1.),(1.,1.),(1.,1.),(1.,1.),(1.,1.),(1.,
1.),(1.,1.),(1.,1.),(1.,1.),(1.,1.),(1.,1.),(1.,1.),(1.,1.),(1.,1.),(1.,
1.),(1.,1.),(1.,1.),(1.,1.),(1.,1.),(1.,1.),(1.,1.),(1.,1.),(1.,1.),(1.,
1.),(1.,1.),(1.,1.),(1.,1.),(1.,1.),(1.,1.),(1.,1.),(1.,1.),(1.,1.),(1.,
1.),(1.,1.),(1.,1.),(1.,1.),(1.,1.),(1.,1.),(1.,1.),(1.,1.),(1.,1.),(1.,
1.),(1.,1.)))
REPRESENTATION_ITEM('')
SURFACE()
);
#107=(
BOUNDED_SURFACE()
B_SPLINE_SURFACE(5,1,((#48382,#48383),(#48384,#48385),(#48386,#48387),(#48388,
#48389),(#48390,#48391),(#48392,#48393),(#48394,#48395),(#48396,#48397),
(#48398,#48399),(#48400,#48401),(#48402,#48403),(#48404,#48405),(#48406,
#48407),(#48408,#48409),(#48410,#48411),(#48412,#48413),(#48414,#48415),
(#48416,#48417),(#48418,#48419),(#48420,#48421),(#48422,#48423),(#48424,
#48425),(#48426,#48427),(#48428,#48429),(#48430,#48431),(#48432,#48433),
(#48434,#48435),(#48436,#48437),(#48438,#48439),(#48440,#48441),(#48442,
#48443),(#48444,#48445),(#48446,#48447),(#48448,#48449),(#48450,#48451),
(#48452,#48453),(#48454,#48455),(#48456,#48457),(#48458,#48459),(#48460,
#48461),(#48462,#48463),(#48464,#48465),(#48466,#48467),(#48468,#48469),
(#48470,#48471),(#48472,#48473),(#48474,#48475),(#48476,#48477),(#48478,
#48479),(#48480,#48481),(#48482,#48483),(#48484,#48485),(#48486,#48487),
(#48488,#48489),(#48490,#48491),(#48492,#48493),(#48494,#48495),(#48496,
#48497),(#48498,#48499),(#48500,#48501),(#48502,#48503),(#48504,#48505),
(#48506,#48507),(#48508,#48509),(#48510,#48511),(#48512,#48513),(#48514,
#48515),(#48516,#48517),(#48518,#48519),(#48520,#48521)),.UNSPECIFIED.,
 .F.,.F.,.F.)
B_SPLINE_SURFACE_WITH_KNOTS((6,1,1,1,1,1,1,1,1,1,1,1,1,1,1,1,1,1,1,1,1,
1,1,1,1,1,1,1,1,1,1,1,1,1,1,1,1,1,1,1,1,1,1,1,1,1,1,1,1,1,1,1,1,1,1,1,1,
1,1,1,1,1,1,1,1,6),(2,2),(-1.,-0.984615384615383,-0.969230769230768,-0.953846153846152,
-0.938461538461537,-0.923076923076922,-0.907692307692306,-0.892307692307691,
-0.876923076923076,-0.86153846153846,-0.846153846153845,-0.83076923076923,
-0.815384615384614,-0.799999999999999,-0.784615384615384,-0.769230769230768,
-0.753846153846153,-0.738461538461538,-0.723076923076922,-0.707692307692307,
-0.692307692307692,-0.676923076923076,-0.661538461538461,-0.646153846153846,
-0.63076923076923,-0.615384615384615,-0.6,-0.584615384615384,-0.569230769230769,
-0.553846153846154,-0.538461538461538,-0.523076923076923,-0.507692307692308,
-0.492307692307692,-0.476923076923077,-0.461538461538462,-0.446153846153846,
-0.430769230769231,-0.415384615384615,-0.4,-0.384615384615385,-0.369230769230769,
-0.353846153846154,-0.338461538461538,-0.323076923076923,-0.307692307692308,
-0.292307692307692,-0.276923076923077,-0.261538461538462,-0.246153846153846,
-0.230769230769231,-0.215384615384615,-0.2,-0.184615384615385,-0.169230769230769,
-0.153846153846154,-0.138461538461538,-0.123076923076923,-0.107692307692308,
-0.0923076923076923,-0.0769230769230769,-0.0615384615384615,-0.0461538461538462,
-0.0307692307692308,-0.0153846153846154,0.),(-1.,1.),.UNSPECIFIED.)
GEOMETRIC_REPRESENTATION_ITEM()
RATIONAL_B_SPLINE_SURFACE(((1.,1.),(1.,1.),(1.,1.),(1.,1.),(1.,1.),(1.,
1.),(1.,1.),(1.,1.),(1.,1.),(1.,1.),(1.,1.),(1.,1.),(1.,1.),(1.,1.),(1.,
1.),(1.,1.),(1.,1.),(1.,1.),(1.,1.),(1.,1.),(1.,1.),(1.,1.),(1.,1.),(1.,
1.),(1.,1.),(1.,1.),(1.,1.),(1.,1.),(1.,1.),(1.,1.),(1.,1.),(1.,1.),(1.,
1.),(1.,1.),(1.,1.),(1.,1.),(1.,1.),(1.,1.),(1.,1.),(1.,1.),(1.,1.),(1.,
1.),(1.,1.),(1.,1.),(1.,1.),(1.,1.),(1.,1.),(1.,1.),(1.,1.),(1.,1.),(1.,
1.),(1.,1.),(1.,1.),(1.,1.),(1.,1.),(1.,1.),(1.,1.),(1.,1.),(1.,1.),(1.,
1.),(1.,1.),(1.,1.),(1.,1.),(1.,1.),(1.,1.),(1.,1.),(1.,1.),(1.,1.),(1.,
1.),(1.,1.)))
REPRESENTATION_ITEM('')
SURFACE()
);
#108=(
BOUNDED_SURFACE()
B_SPLINE_SURFACE(5,1,((#48594,#48595),(#48596,#48597),(#48598,#48599),(#48600,
#48601),(#48602,#48603),(#48604,#48605),(#48606,#48607),(#48608,#48609),
(#48610,#48611),(#48612,#48613),(#48614,#48615),(#48616,#48617),(#48618,
#48619),(#48620,#48621),(#48622,#48623),(#48624,#48625),(#48626,#48627),
(#48628,#48629),(#48630,#48631),(#48632,#48633),(#48634,#48635),(#48636,
#48637),(#48638,#48639),(#48640,#48641),(#48642,#48643),(#48644,#48645),
(#48646,#48647),(#48648,#48649),(#48650,#48651),(#48652,#48653),(#48654,
#48655),(#48656,#48657),(#48658,#48659),(#48660,#48661),(#48662,#48663),
(#48664,#48665),(#48666,#48667),(#48668,#48669),(#48670,#48671),(#48672,
#48673),(#48674,#48675),(#48676,#48677),(#48678,#48679),(#48680,#48681),
(#48682,#48683),(#48684,#48685),(#48686,#48687),(#48688,#48689),(#48690,
#48691),(#48692,#48693),(#48694,#48695),(#48696,#48697),(#48698,#48699),
(#48700,#48701),(#48702,#48703),(#48704,#48705),(#48706,#48707),(#48708,
#48709),(#48710,#48711),(#48712,#48713),(#48714,#48715),(#48716,#48717),
(#48718,#48719),(#48720,#48721),(#48722,#48723),(#48724,#48725),(#48726,
#48727),(#48728,#48729),(#48730,#48731),(#48732,#48733)),.UNSPECIFIED.,
 .F.,.F.,.F.)
B_SPLINE_SURFACE_WITH_KNOTS((6,1,1,1,1,1,1,1,1,1,1,1,1,1,1,1,1,1,1,1,1,
1,1,1,1,1,1,1,1,1,1,1,1,1,1,1,1,1,1,1,1,1,1,1,1,1,1,1,1,1,1,1,1,1,1,1,1,
1,1,1,1,1,1,1,1,6),(2,2),(-1.,-0.984615384615383,-0.969230769230768,-0.953846153846152,
-0.938461538461537,-0.923076923076922,-0.907692307692306,-0.892307692307691,
-0.876923076923076,-0.86153846153846,-0.846153846153845,-0.83076923076923,
-0.815384615384614,-0.799999999999999,-0.784615384615384,-0.769230769230768,
-0.753846153846153,-0.738461538461538,-0.723076923076922,-0.707692307692307,
-0.692307692307692,-0.676923076923076,-0.661538461538461,-0.646153846153846,
-0.63076923076923,-0.615384615384615,-0.6,-0.584615384615384,-0.569230769230769,
-0.553846153846154,-0.538461538461538,-0.523076923076923,-0.507692307692308,
-0.492307692307692,-0.476923076923077,-0.461538461538462,-0.446153846153846,
-0.430769230769231,-0.415384615384615,-0.4,-0.384615384615385,-0.369230769230769,
-0.353846153846154,-0.338461538461538,-0.323076923076923,-0.307692307692308,
-0.292307692307692,-0.276923076923077,-0.261538461538462,-0.246153846153846,
-0.230769230769231,-0.215384615384615,-0.2,-0.184615384615385,-0.169230769230769,
-0.153846153846154,-0.138461538461538,-0.123076923076923,-0.107692307692308,
-0.0923076923076923,-0.0769230769230769,-0.0615384615384615,-0.0461538461538462,
-0.0307692307692308,-0.0153846153846154,0.),(-1.,1.),.UNSPECIFIED.)
GEOMETRIC_REPRESENTATION_ITEM()
RATIONAL_B_SPLINE_SURFACE(((1.,1.),(1.,1.),(1.,1.),(1.,1.),(1.,1.),(1.,
1.),(1.,1.),(1.,1.),(1.,1.),(1.,1.),(1.,1.),(1.,1.),(1.,1.),(1.,1.),(1.,
1.),(1.,1.),(1.,1.),(1.,1.),(1.,1.),(1.,1.),(1.,1.),(1.,1.),(1.,1.),(1.,
1.),(1.,1.),(1.,1.),(1.,1.),(1.,1.),(1.,1.),(1.,1.),(1.,1.),(1.,1.),(1.,
1.),(1.,1.),(1.,1.),(1.,1.),(1.,1.),(1.,1.),(1.,1.),(1.,1.),(1.,1.),(1.,
1.),(1.,1.),(1.,1.),(1.,1.),(1.,1.),(1.,1.),(1.,1.),(1.,1.),(1.,1.),(1.,
1.),(1.,1.),(1.,1.),(1.,1.),(1.,1.),(1.,1.),(1.,1.),(1.,1.),(1.,1.),(1.,
1.),(1.,1.),(1.,1.),(1.,1.),(1.,1.),(1.,1.),(1.,1.),(1.,1.),(1.,1.),(1.,
1.),(1.,1.)))
REPRESENTATION_ITEM('')
SURFACE()
);
#109=(
BOUNDED_SURFACE()
B_SPLINE_SURFACE(5,1,((#48824,#48825),(#48826,#48827),(#48828,#48829),(#48830,
#48831),(#48832,#48833),(#48834,#48835),(#48836,#48837),(#48838,#48839),
(#48840,#48841),(#48842,#48843),(#48844,#48845),(#48846,#48847),(#48848,
#48849),(#48850,#48851),(#48852,#48853),(#48854,#48855),(#48856,#48857),
(#48858,#48859),(#48860,#48861),(#48862,#48863),(#48864,#48865),(#48866,
#48867),(#48868,#48869),(#48870,#48871),(#48872,#48873),(#48874,#48875),
(#48876,#48877),(#48878,#48879),(#48880,#48881),(#48882,#48883),(#48884,
#48885),(#48886,#48887),(#48888,#48889),(#48890,#48891),(#48892,#48893),
(#48894,#48895),(#48896,#48897),(#48898,#48899),(#48900,#48901),(#48902,
#48903),(#48904,#48905),(#48906,#48907),(#48908,#48909),(#48910,#48911),
(#48912,#48913),(#48914,#48915),(#48916,#48917),(#48918,#48919),(#48920,
#48921),(#48922,#48923),(#48924,#48925),(#48926,#48927),(#48928,#48929),
(#48930,#48931),(#48932,#48933),(#48934,#48935),(#48936,#48937),(#48938,
#48939),(#48940,#48941),(#48942,#48943),(#48944,#48945),(#48946,#48947),
(#48948,#48949),(#48950,#48951),(#48952,#48953),(#48954,#48955),(#48956,
#48957),(#48958,#48959),(#48960,#48961),(#48962,#48963)),.UNSPECIFIED.,
 .F.,.F.,.F.)
B_SPLINE_SURFACE_WITH_KNOTS((6,1,1,1,1,1,1,1,1,1,1,1,1,1,1,1,1,1,1,1,1,
1,1,1,1,1,1,1,1,1,1,1,1,1,1,1,1,1,1,1,1,1,1,1,1,1,1,1,1,1,1,1,1,1,1,1,1,
1,1,1,1,1,1,1,1,6),(2,2),(-1.,-0.984615384615383,-0.969230769230768,-0.953846153846152,
-0.938461538461537,-0.923076923076922,-0.907692307692306,-0.892307692307691,
-0.876923076923076,-0.86153846153846,-0.846153846153845,-0.83076923076923,
-0.815384615384614,-0.799999999999999,-0.784615384615384,-0.769230769230768,
-0.753846153846153,-0.738461538461538,-0.723076923076922,-0.707692307692307,
-0.692307692307692,-0.676923076923076,-0.661538461538461,-0.646153846153846,
-0.63076923076923,-0.615384615384615,-0.6,-0.584615384615384,-0.569230769230769,
-0.553846153846154,-0.538461538461538,-0.523076923076923,-0.507692307692308,
-0.492307692307692,-0.476923076923077,-0.461538461538462,-0.446153846153846,
-0.430769230769231,-0.415384615384615,-0.4,-0.384615384615385,-0.369230769230769,
-0.353846153846154,-0.338461538461538,-0.323076923076923,-0.307692307692308,
-0.292307692307692,-0.276923076923077,-0.261538461538462,-0.246153846153846,
-0.230769230769231,-0.215384615384615,-0.2,-0.184615384615385,-0.169230769230769,
-0.153846153846154,-0.138461538461538,-0.123076923076923,-0.107692307692308,
-0.0923076923076923,-0.0769230769230769,-0.0615384615384615,-0.0461538461538462,
-0.0307692307692308,-0.0153846153846154,0.),(-1.,1.),.UNSPECIFIED.)
GEOMETRIC_REPRESENTATION_ITEM()
RATIONAL_B_SPLINE_SURFACE(((1.,1.),(1.,1.),(1.,1.),(1.,1.),(1.,1.),(1.,
1.),(1.,1.),(1.,1.),(1.,1.),(1.,1.),(1.,1.),(1.,1.),(1.,1.),(1.,1.),(1.,
1.),(1.,1.),(1.,1.),(1.,1.),(1.,1.),(1.,1.),(1.,1.),(1.,1.),(1.,1.),(1.,
1.),(1.,1.),(1.,1.),(1.,1.),(1.,1.),(1.,1.),(1.,1.),(1.,1.),(1.,1.),(1.,
1.),(1.,1.),(1.,1.),(1.,1.),(1.,1.),(1.,1.),(1.,1.),(1.,1.),(1.,1.),(1.,
1.),(1.,1.),(1.,1.),(1.,1.),(1.,1.),(1.,1.),(1.,1.),(1.,1.),(1.,1.),(1.,
1.),(1.,1.),(1.,1.),(1.,1.),(1.,1.),(1.,1.),(1.,1.),(1.,1.),(1.,1.),(1.,
1.),(1.,1.),(1.,1.),(1.,1.),(1.,1.),(1.,1.),(1.,1.),(1.,1.),(1.,1.),(1.,
1.),(1.,1.)))
REPRESENTATION_ITEM('')
SURFACE()
);
#110=(
BOUNDED_SURFACE()
B_SPLINE_SURFACE(5,1,((#49036,#49037),(#49038,#49039),(#49040,#49041),(#49042,
#49043),(#49044,#49045),(#49046,#49047),(#49048,#49049),(#49050,#49051),
(#49052,#49053),(#49054,#49055),(#49056,#49057),(#49058,#49059),(#49060,
#49061),(#49062,#49063),(#49064,#49065),(#49066,#49067),(#49068,#49069),
(#49070,#49071),(#49072,#49073),(#49074,#49075),(#49076,#49077),(#49078,
#49079),(#49080,#49081),(#49082,#49083),(#49084,#49085),(#49086,#49087),
(#49088,#49089),(#49090,#49091),(#49092,#49093),(#49094,#49095),(#49096,
#49097),(#49098,#49099),(#49100,#49101),(#49102,#49103),(#49104,#49105),
(#49106,#49107),(#49108,#49109),(#49110,#49111),(#49112,#49113),(#49114,
#49115),(#49116,#49117),(#49118,#49119),(#49120,#49121),(#49122,#49123),
(#49124,#49125),(#49126,#49127),(#49128,#49129),(#49130,#49131),(#49132,
#49133),(#49134,#49135),(#49136,#49137),(#49138,#49139),(#49140,#49141),
(#49142,#49143),(#49144,#49145),(#49146,#49147),(#49148,#49149),(#49150,
#49151),(#49152,#49153),(#49154,#49155),(#49156,#49157),(#49158,#49159),
(#49160,#49161),(#49162,#49163),(#49164,#49165),(#49166,#49167),(#49168,
#49169),(#49170,#49171),(#49172,#49173),(#49174,#49175)),.UNSPECIFIED.,
 .F.,.F.,.F.)
B_SPLINE_SURFACE_WITH_KNOTS((6,1,1,1,1,1,1,1,1,1,1,1,1,1,1,1,1,1,1,1,1,
1,1,1,1,1,1,1,1,1,1,1,1,1,1,1,1,1,1,1,1,1,1,1,1,1,1,1,1,1,1,1,1,1,1,1,1,
1,1,1,1,1,1,1,1,6),(2,2),(-1.,-0.984615384615383,-0.969230769230768,-0.953846153846152,
-0.938461538461537,-0.923076923076922,-0.907692307692306,-0.892307692307691,
-0.876923076923076,-0.86153846153846,-0.846153846153845,-0.83076923076923,
-0.815384615384614,-0.799999999999999,-0.784615384615384,-0.769230769230768,
-0.753846153846153,-0.738461538461538,-0.723076923076922,-0.707692307692307,
-0.692307692307692,-0.676923076923076,-0.661538461538461,-0.646153846153846,
-0.63076923076923,-0.615384615384615,-0.6,-0.584615384615384,-0.569230769230769,
-0.553846153846154,-0.538461538461538,-0.523076923076923,-0.507692307692308,
-0.492307692307692,-0.476923076923077,-0.461538461538462,-0.446153846153846,
-0.430769230769231,-0.415384615384615,-0.4,-0.384615384615385,-0.369230769230769,
-0.353846153846154,-0.338461538461538,-0.323076923076923,-0.307692307692308,
-0.292307692307692,-0.276923076923077,-0.261538461538462,-0.246153846153846,
-0.230769230769231,-0.215384615384615,-0.2,-0.184615384615385,-0.169230769230769,
-0.153846153846154,-0.138461538461538,-0.123076923076923,-0.107692307692308,
-0.0923076923076923,-0.0769230769230769,-0.0615384615384615,-0.0461538461538462,
-0.0307692307692308,-0.0153846153846154,0.),(-1.,1.),.UNSPECIFIED.)
GEOMETRIC_REPRESENTATION_ITEM()
RATIONAL_B_SPLINE_SURFACE(((1.,1.),(1.,1.),(1.,1.),(1.,1.),(1.,1.),(1.,
1.),(1.,1.),(1.,1.),(1.,1.),(1.,1.),(1.,1.),(1.,1.),(1.,1.),(1.,1.),(1.,
1.),(1.,1.),(1.,1.),(1.,1.),(1.,1.),(1.,1.),(1.,1.),(1.,1.),(1.,1.),(1.,
1.),(1.,1.),(1.,1.),(1.,1.),(1.,1.),(1.,1.),(1.,1.),(1.,1.),(1.,1.),(1.,
1.),(1.,1.),(1.,1.),(1.,1.),(1.,1.),(1.,1.),(1.,1.),(1.,1.),(1.,1.),(1.,
1.),(1.,1.),(1.,1.),(1.,1.),(1.,1.),(1.,1.),(1.,1.),(1.,1.),(1.,1.),(1.,
1.),(1.,1.),(1.,1.),(1.,1.),(1.,1.),(1.,1.),(1.,1.),(1.,1.),(1.,1.),(1.,
1.),(1.,1.),(1.,1.),(1.,1.),(1.,1.),(1.,1.),(1.,1.),(1.,1.),(1.,1.),(1.,
1.),(1.,1.)))
REPRESENTATION_ITEM('')
SURFACE()
);
#111=(
BOUNDED_SURFACE()
B_SPLINE_SURFACE(5,1,((#49266,#49267),(#49268,#49269),(#49270,#49271),(#49272,
#49273),(#49274,#49275),(#49276,#49277),(#49278,#49279),(#49280,#49281),
(#49282,#49283),(#49284,#49285),(#49286,#49287),(#49288,#49289),(#49290,
#49291),(#49292,#49293),(#49294,#49295),(#49296,#49297),(#49298,#49299),
(#49300,#49301),(#49302,#49303),(#49304,#49305),(#49306,#49307),(#49308,
#49309),(#49310,#49311),(#49312,#49313),(#49314,#49315),(#49316,#49317),
(#49318,#49319),(#49320,#49321),(#49322,#49323),(#49324,#49325),(#49326,
#49327),(#49328,#49329),(#49330,#49331),(#49332,#49333),(#49334,#49335),
(#49336,#49337),(#49338,#49339),(#49340,#49341),(#49342,#49343),(#49344,
#49345),(#49346,#49347),(#49348,#49349),(#49350,#49351),(#49352,#49353),
(#49354,#49355),(#49356,#49357),(#49358,#49359),(#49360,#49361),(#49362,
#49363),(#49364,#49365),(#49366,#49367),(#49368,#49369),(#49370,#49371),
(#49372,#49373),(#49374,#49375),(#49376,#49377),(#49378,#49379),(#49380,
#49381),(#49382,#49383),(#49384,#49385),(#49386,#49387),(#49388,#49389),
(#49390,#49391),(#49392,#49393),(#49394,#49395),(#49396,#49397),(#49398,
#49399),(#49400,#49401),(#49402,#49403),(#49404,#49405)),.UNSPECIFIED.,
 .F.,.F.,.F.)
B_SPLINE_SURFACE_WITH_KNOTS((6,1,1,1,1,1,1,1,1,1,1,1,1,1,1,1,1,1,1,1,1,
1,1,1,1,1,1,1,1,1,1,1,1,1,1,1,1,1,1,1,1,1,1,1,1,1,1,1,1,1,1,1,1,1,1,1,1,
1,1,1,1,1,1,1,1,6),(2,2),(-1.,-0.984615384615383,-0.969230769230768,-0.953846153846152,
-0.938461538461537,-0.923076923076922,-0.907692307692306,-0.892307692307691,
-0.876923076923076,-0.86153846153846,-0.846153846153845,-0.83076923076923,
-0.815384615384614,-0.799999999999999,-0.784615384615384,-0.769230769230768,
-0.753846153846153,-0.738461538461538,-0.723076923076922,-0.707692307692307,
-0.692307692307692,-0.676923076923076,-0.661538461538461,-0.646153846153846,
-0.63076923076923,-0.615384615384615,-0.6,-0.584615384615384,-0.569230769230769,
-0.553846153846154,-0.538461538461538,-0.523076923076923,-0.507692307692308,
-0.492307692307692,-0.476923076923077,-0.461538461538462,-0.446153846153846,
-0.430769230769231,-0.415384615384615,-0.4,-0.384615384615385,-0.369230769230769,
-0.353846153846154,-0.338461538461538,-0.323076923076923,-0.307692307692308,
-0.292307692307692,-0.276923076923077,-0.261538461538462,-0.246153846153846,
-0.230769230769231,-0.215384615384615,-0.2,-0.184615384615385,-0.169230769230769,
-0.153846153846154,-0.138461538461538,-0.123076923076923,-0.107692307692308,
-0.0923076923076923,-0.0769230769230769,-0.0615384615384615,-0.0461538461538462,
-0.0307692307692308,-0.0153846153846154,0.),(-1.,1.),.UNSPECIFIED.)
GEOMETRIC_REPRESENTATION_ITEM()
RATIONAL_B_SPLINE_SURFACE(((1.,1.),(1.,1.),(1.,1.),(1.,1.),(1.,1.),(1.,
1.),(1.,1.),(1.,1.),(1.,1.),(1.,1.),(1.,1.),(1.,1.),(1.,1.),(1.,1.),(1.,
1.),(1.,1.),(1.,1.),(1.,1.),(1.,1.),(1.,1.),(1.,1.),(1.,1.),(1.,1.),(1.,
1.),(1.,1.),(1.,1.),(1.,1.),(1.,1.),(1.,1.),(1.,1.),(1.,1.),(1.,1.),(1.,
1.),(1.,1.),(1.,1.),(1.,1.),(1.,1.),(1.,1.),(1.,1.),(1.,1.),(1.,1.),(1.,
1.),(1.,1.),(1.,1.),(1.,1.),(1.,1.),(1.,1.),(1.,1.),(1.,1.),(1.,1.),(1.,
1.),(1.,1.),(1.,1.),(1.,1.),(1.,1.),(1.,1.),(1.,1.),(1.,1.),(1.,1.),(1.,
1.),(1.,1.),(1.,1.),(1.,1.),(1.,1.),(1.,1.),(1.,1.),(1.,1.),(1.,1.),(1.,
1.),(1.,1.)))
REPRESENTATION_ITEM('')
SURFACE()
);
#112=(
BOUNDED_SURFACE()
B_SPLINE_SURFACE(5,1,((#49478,#49479),(#49480,#49481),(#49482,#49483),(#49484,
#49485),(#49486,#49487),(#49488,#49489),(#49490,#49491),(#49492,#49493),
(#49494,#49495),(#49496,#49497),(#49498,#49499),(#49500,#49501),(#49502,
#49503),(#49504,#49505),(#49506,#49507),(#49508,#49509),(#49510,#49511),
(#49512,#49513),(#49514,#49515),(#49516,#49517),(#49518,#49519),(#49520,
#49521),(#49522,#49523),(#49524,#49525),(#49526,#49527),(#49528,#49529),
(#49530,#49531),(#49532,#49533),(#49534,#49535),(#49536,#49537),(#49538,
#49539),(#49540,#49541),(#49542,#49543),(#49544,#49545),(#49546,#49547),
(#49548,#49549),(#49550,#49551),(#49552,#49553),(#49554,#49555),(#49556,
#49557),(#49558,#49559),(#49560,#49561),(#49562,#49563),(#49564,#49565),
(#49566,#49567),(#49568,#49569),(#49570,#49571),(#49572,#49573),(#49574,
#49575),(#49576,#49577),(#49578,#49579),(#49580,#49581),(#49582,#49583),
(#49584,#49585),(#49586,#49587),(#49588,#49589),(#49590,#49591),(#49592,
#49593),(#49594,#49595),(#49596,#49597),(#49598,#49599),(#49600,#49601),
(#49602,#49603),(#49604,#49605),(#49606,#49607),(#49608,#49609),(#49610,
#49611),(#49612,#49613),(#49614,#49615),(#49616,#49617)),.UNSPECIFIED.,
 .F.,.F.,.F.)
B_SPLINE_SURFACE_WITH_KNOTS((6,1,1,1,1,1,1,1,1,1,1,1,1,1,1,1,1,1,1,1,1,
1,1,1,1,1,1,1,1,1,1,1,1,1,1,1,1,1,1,1,1,1,1,1,1,1,1,1,1,1,1,1,1,1,1,1,1,
1,1,1,1,1,1,1,1,6),(2,2),(-1.,-0.984615384615383,-0.969230769230768,-0.953846153846152,
-0.938461538461537,-0.923076923076922,-0.907692307692306,-0.892307692307691,
-0.876923076923076,-0.86153846153846,-0.846153846153845,-0.83076923076923,
-0.815384615384614,-0.799999999999999,-0.784615384615384,-0.769230769230768,
-0.753846153846153,-0.738461538461538,-0.723076923076922,-0.707692307692307,
-0.692307692307692,-0.676923076923076,-0.661538461538461,-0.646153846153846,
-0.63076923076923,-0.615384615384615,-0.6,-0.584615384615384,-0.569230769230769,
-0.553846153846154,-0.538461538461538,-0.523076923076923,-0.507692307692308,
-0.492307692307692,-0.476923076923077,-0.461538461538462,-0.446153846153846,
-0.430769230769231,-0.415384615384615,-0.4,-0.384615384615385,-0.369230769230769,
-0.353846153846154,-0.338461538461538,-0.323076923076923,-0.307692307692308,
-0.292307692307692,-0.276923076923077,-0.261538461538462,-0.246153846153846,
-0.230769230769231,-0.215384615384615,-0.2,-0.184615384615385,-0.169230769230769,
-0.153846153846154,-0.138461538461538,-0.123076923076923,-0.107692307692308,
-0.0923076923076923,-0.0769230769230769,-0.0615384615384615,-0.0461538461538462,
-0.0307692307692308,-0.0153846153846154,0.),(-1.,1.),.UNSPECIFIED.)
GEOMETRIC_REPRESENTATION_ITEM()
RATIONAL_B_SPLINE_SURFACE(((1.,1.),(1.,1.),(1.,1.),(1.,1.),(1.,1.),(1.,
1.),(1.,1.),(1.,1.),(1.,1.),(1.,1.),(1.,1.),(1.,1.),(1.,1.),(1.,1.),(1.,
1.),(1.,1.),(1.,1.),(1.,1.),(1.,1.),(1.,1.),(1.,1.),(1.,1.),(1.,1.),(1.,
1.),(1.,1.),(1.,1.),(1.,1.),(1.,1.),(1.,1.),(1.,1.),(1.,1.),(1.,1.),(1.,
1.),(1.,1.),(1.,1.),(1.,1.),(1.,1.),(1.,1.),(1.,1.),(1.,1.),(1.,1.),(1.,
1.),(1.,1.),(1.,1.),(1.,1.),(1.,1.),(1.,1.),(1.,1.),(1.,1.),(1.,1.),(1.,
1.),(1.,1.),(1.,1.),(1.,1.),(1.,1.),(1.,1.),(1.,1.),(1.,1.),(1.,1.),(1.,
1.),(1.,1.),(1.,1.),(1.,1.),(1.,1.),(1.,1.),(1.,1.),(1.,1.),(1.,1.),(1.,
1.),(1.,1.)))
REPRESENTATION_ITEM('')
SURFACE()
);
#113=(
BOUNDED_SURFACE()
B_SPLINE_SURFACE(5,1,((#49708,#49709),(#49710,#49711),(#49712,#49713),(#49714,
#49715),(#49716,#49717),(#49718,#49719),(#49720,#49721),(#49722,#49723),
(#49724,#49725),(#49726,#49727),(#49728,#49729),(#49730,#49731),(#49732,
#49733),(#49734,#49735),(#49736,#49737),(#49738,#49739),(#49740,#49741),
(#49742,#49743),(#49744,#49745),(#49746,#49747),(#49748,#49749),(#49750,
#49751),(#49752,#49753),(#49754,#49755),(#49756,#49757),(#49758,#49759),
(#49760,#49761),(#49762,#49763),(#49764,#49765),(#49766,#49767),(#49768,
#49769),(#49770,#49771),(#49772,#49773),(#49774,#49775),(#49776,#49777),
(#49778,#49779),(#49780,#49781),(#49782,#49783),(#49784,#49785),(#49786,
#49787),(#49788,#49789),(#49790,#49791),(#49792,#49793),(#49794,#49795),
(#49796,#49797),(#49798,#49799),(#49800,#49801),(#49802,#49803),(#49804,
#49805),(#49806,#49807),(#49808,#49809),(#49810,#49811),(#49812,#49813),
(#49814,#49815),(#49816,#49817),(#49818,#49819),(#49820,#49821),(#49822,
#49823),(#49824,#49825),(#49826,#49827),(#49828,#49829),(#49830,#49831),
(#49832,#49833),(#49834,#49835),(#49836,#49837),(#49838,#49839),(#49840,
#49841),(#49842,#49843),(#49844,#49845),(#49846,#49847)),.UNSPECIFIED.,
 .F.,.F.,.F.)
B_SPLINE_SURFACE_WITH_KNOTS((6,1,1,1,1,1,1,1,1,1,1,1,1,1,1,1,1,1,1,1,1,
1,1,1,1,1,1,1,1,1,1,1,1,1,1,1,1,1,1,1,1,1,1,1,1,1,1,1,1,1,1,1,1,1,1,1,1,
1,1,1,1,1,1,1,1,6),(2,2),(-1.,-0.984615384615383,-0.969230769230768,-0.953846153846152,
-0.938461538461537,-0.923076923076922,-0.907692307692306,-0.892307692307691,
-0.876923076923076,-0.86153846153846,-0.846153846153845,-0.83076923076923,
-0.815384615384614,-0.799999999999999,-0.784615384615384,-0.769230769230768,
-0.753846153846153,-0.738461538461538,-0.723076923076922,-0.707692307692307,
-0.692307692307692,-0.676923076923076,-0.661538461538461,-0.646153846153846,
-0.63076923076923,-0.615384615384615,-0.6,-0.584615384615384,-0.569230769230769,
-0.553846153846154,-0.538461538461538,-0.523076923076923,-0.507692307692308,
-0.492307692307692,-0.476923076923077,-0.461538461538462,-0.446153846153846,
-0.430769230769231,-0.415384615384615,-0.4,-0.384615384615385,-0.369230769230769,
-0.353846153846154,-0.338461538461538,-0.323076923076923,-0.307692307692308,
-0.292307692307692,-0.276923076923077,-0.261538461538462,-0.246153846153846,
-0.230769230769231,-0.215384615384615,-0.2,-0.184615384615385,-0.169230769230769,
-0.153846153846154,-0.138461538461538,-0.123076923076923,-0.107692307692308,
-0.0923076923076923,-0.0769230769230769,-0.0615384615384615,-0.0461538461538462,
-0.0307692307692308,-0.0153846153846154,0.),(-1.,1.),.UNSPECIFIED.)
GEOMETRIC_REPRESENTATION_ITEM()
RATIONAL_B_SPLINE_SURFACE(((1.,1.),(1.,1.),(1.,1.),(1.,1.),(1.,1.),(1.,
1.),(1.,1.),(1.,1.),(1.,1.),(1.,1.),(1.,1.),(1.,1.),(1.,1.),(1.,1.),(1.,
1.),(1.,1.),(1.,1.),(1.,1.),(1.,1.),(1.,1.),(1.,1.),(1.,1.),(1.,1.),(1.,
1.),(1.,1.),(1.,1.),(1.,1.),(1.,1.),(1.,1.),(1.,1.),(1.,1.),(1.,1.),(1.,
1.),(1.,1.),(1.,1.),(1.,1.),(1.,1.),(1.,1.),(1.,1.),(1.,1.),(1.,1.),(1.,
1.),(1.,1.),(1.,1.),(1.,1.),(1.,1.),(1.,1.),(1.,1.),(1.,1.),(1.,1.),(1.,
1.),(1.,1.),(1.,1.),(1.,1.),(1.,1.),(1.,1.),(1.,1.),(1.,1.),(1.,1.),(1.,
1.),(1.,1.),(1.,1.),(1.,1.),(1.,1.),(1.,1.),(1.,1.),(1.,1.),(1.,1.),(1.,
1.),(1.,1.)))
REPRESENTATION_ITEM('')
SURFACE()
);
#114=(
BOUNDED_SURFACE()
B_SPLINE_SURFACE(5,1,((#49920,#49921),(#49922,#49923),(#49924,#49925),(#49926,
#49927),(#49928,#49929),(#49930,#49931),(#49932,#49933),(#49934,#49935),
(#49936,#49937),(#49938,#49939),(#49940,#49941),(#49942,#49943),(#49944,
#49945),(#49946,#49947),(#49948,#49949),(#49950,#49951),(#49952,#49953),
(#49954,#49955),(#49956,#49957),(#49958,#49959),(#49960,#49961),(#49962,
#49963),(#49964,#49965),(#49966,#49967),(#49968,#49969),(#49970,#49971),
(#49972,#49973),(#49974,#49975),(#49976,#49977),(#49978,#49979),(#49980,
#49981),(#49982,#49983),(#49984,#49985),(#49986,#49987),(#49988,#49989),
(#49990,#49991),(#49992,#49993),(#49994,#49995),(#49996,#49997),(#49998,
#49999),(#50000,#50001),(#50002,#50003),(#50004,#50005),(#50006,#50007),
(#50008,#50009),(#50010,#50011),(#50012,#50013),(#50014,#50015),(#50016,
#50017),(#50018,#50019),(#50020,#50021),(#50022,#50023),(#50024,#50025),
(#50026,#50027),(#50028,#50029),(#50030,#50031),(#50032,#50033),(#50034,
#50035),(#50036,#50037),(#50038,#50039),(#50040,#50041),(#50042,#50043),
(#50044,#50045),(#50046,#50047),(#50048,#50049),(#50050,#50051),(#50052,
#50053),(#50054,#50055),(#50056,#50057),(#50058,#50059)),.UNSPECIFIED.,
 .F.,.F.,.F.)
B_SPLINE_SURFACE_WITH_KNOTS((6,1,1,1,1,1,1,1,1,1,1,1,1,1,1,1,1,1,1,1,1,
1,1,1,1,1,1,1,1,1,1,1,1,1,1,1,1,1,1,1,1,1,1,1,1,1,1,1,1,1,1,1,1,1,1,1,1,
1,1,1,1,1,1,1,1,6),(2,2),(-1.,-0.984615384615383,-0.969230769230768,-0.953846153846152,
-0.938461538461537,-0.923076923076922,-0.907692307692306,-0.892307692307691,
-0.876923076923076,-0.86153846153846,-0.846153846153845,-0.83076923076923,
-0.815384615384614,-0.799999999999999,-0.784615384615384,-0.769230769230768,
-0.753846153846153,-0.738461538461538,-0.723076923076922,-0.707692307692307,
-0.692307692307692,-0.676923076923076,-0.661538461538461,-0.646153846153846,
-0.63076923076923,-0.615384615384615,-0.6,-0.584615384615384,-0.569230769230769,
-0.553846153846154,-0.538461538461538,-0.523076923076923,-0.507692307692308,
-0.492307692307692,-0.476923076923077,-0.461538461538462,-0.446153846153846,
-0.430769230769231,-0.415384615384615,-0.4,-0.384615384615385,-0.369230769230769,
-0.353846153846154,-0.338461538461538,-0.323076923076923,-0.307692307692308,
-0.292307692307692,-0.276923076923077,-0.261538461538462,-0.246153846153846,
-0.230769230769231,-0.215384615384615,-0.2,-0.184615384615385,-0.169230769230769,
-0.153846153846154,-0.138461538461538,-0.123076923076923,-0.107692307692308,
-0.0923076923076923,-0.0769230769230769,-0.0615384615384615,-0.0461538461538462,
-0.0307692307692308,-0.0153846153846154,0.),(-1.,1.),.UNSPECIFIED.)
GEOMETRIC_REPRESENTATION_ITEM()
RATIONAL_B_SPLINE_SURFACE(((1.,1.),(1.,1.),(1.,1.),(1.,1.),(1.,1.),(1.,
1.),(1.,1.),(1.,1.),(1.,1.),(1.,1.),(1.,1.),(1.,1.),(1.,1.),(1.,1.),(1.,
1.),(1.,1.),(1.,1.),(1.,1.),(1.,1.),(1.,1.),(1.,1.),(1.,1.),(1.,1.),(1.,
1.),(1.,1.),(1.,1.),(1.,1.),(1.,1.),(1.,1.),(1.,1.),(1.,1.),(1.,1.),(1.,
1.),(1.,1.),(1.,1.),(1.,1.),(1.,1.),(1.,1.),(1.,1.),(1.,1.),(1.,1.),(1.,
1.),(1.,1.),(1.,1.),(1.,1.),(1.,1.),(1.,1.),(1.,1.),(1.,1.),(1.,1.),(1.,
1.),(1.,1.),(1.,1.),(1.,1.),(1.,1.),(1.,1.),(1.,1.),(1.,1.),(1.,1.),(1.,
1.),(1.,1.),(1.,1.),(1.,1.),(1.,1.),(1.,1.),(1.,1.),(1.,1.),(1.,1.),(1.,
1.),(1.,1.)))
REPRESENTATION_ITEM('')
SURFACE()
);
#115=(
BOUNDED_SURFACE()
B_SPLINE_SURFACE(5,1,((#50150,#50151),(#50152,#50153),(#50154,#50155),(#50156,
#50157),(#50158,#50159),(#50160,#50161),(#50162,#50163),(#50164,#50165),
(#50166,#50167),(#50168,#50169),(#50170,#50171),(#50172,#50173),(#50174,
#50175),(#50176,#50177),(#50178,#50179),(#50180,#50181),(#50182,#50183),
(#50184,#50185),(#50186,#50187),(#50188,#50189),(#50190,#50191),(#50192,
#50193),(#50194,#50195),(#50196,#50197),(#50198,#50199),(#50200,#50201),
(#50202,#50203),(#50204,#50205),(#50206,#50207),(#50208,#50209),(#50210,
#50211),(#50212,#50213),(#50214,#50215),(#50216,#50217),(#50218,#50219),
(#50220,#50221),(#50222,#50223),(#50224,#50225),(#50226,#50227),(#50228,
#50229),(#50230,#50231),(#50232,#50233),(#50234,#50235),(#50236,#50237),
(#50238,#50239),(#50240,#50241),(#50242,#50243),(#50244,#50245),(#50246,
#50247),(#50248,#50249),(#50250,#50251),(#50252,#50253),(#50254,#50255),
(#50256,#50257),(#50258,#50259),(#50260,#50261),(#50262,#50263),(#50264,
#50265),(#50266,#50267),(#50268,#50269),(#50270,#50271),(#50272,#50273),
(#50274,#50275),(#50276,#50277),(#50278,#50279),(#50280,#50281),(#50282,
#50283),(#50284,#50285),(#50286,#50287),(#50288,#50289)),.UNSPECIFIED.,
 .F.,.F.,.F.)
B_SPLINE_SURFACE_WITH_KNOTS((6,1,1,1,1,1,1,1,1,1,1,1,1,1,1,1,1,1,1,1,1,
1,1,1,1,1,1,1,1,1,1,1,1,1,1,1,1,1,1,1,1,1,1,1,1,1,1,1,1,1,1,1,1,1,1,1,1,
1,1,1,1,1,1,1,1,6),(2,2),(-1.,-0.984615384615383,-0.969230769230768,-0.953846153846152,
-0.938461538461537,-0.923076923076922,-0.907692307692306,-0.892307692307691,
-0.876923076923076,-0.86153846153846,-0.846153846153845,-0.83076923076923,
-0.815384615384614,-0.799999999999999,-0.784615384615384,-0.769230769230768,
-0.753846153846153,-0.738461538461538,-0.723076923076922,-0.707692307692307,
-0.692307692307692,-0.676923076923076,-0.661538461538461,-0.646153846153846,
-0.63076923076923,-0.615384615384615,-0.6,-0.584615384615384,-0.569230769230769,
-0.553846153846154,-0.538461538461538,-0.523076923076923,-0.507692307692308,
-0.492307692307692,-0.476923076923077,-0.461538461538462,-0.446153846153846,
-0.430769230769231,-0.415384615384615,-0.4,-0.384615384615385,-0.369230769230769,
-0.353846153846154,-0.338461538461538,-0.323076923076923,-0.307692307692308,
-0.292307692307692,-0.276923076923077,-0.261538461538462,-0.246153846153846,
-0.230769230769231,-0.215384615384615,-0.2,-0.184615384615385,-0.169230769230769,
-0.153846153846154,-0.138461538461538,-0.123076923076923,-0.107692307692308,
-0.0923076923076923,-0.0769230769230769,-0.0615384615384615,-0.0461538461538462,
-0.0307692307692308,-0.0153846153846154,0.),(-1.,1.),.UNSPECIFIED.)
GEOMETRIC_REPRESENTATION_ITEM()
RATIONAL_B_SPLINE_SURFACE(((1.,1.),(1.,1.),(1.,1.),(1.,1.),(1.,1.),(1.,
1.),(1.,1.),(1.,1.),(1.,1.),(1.,1.),(1.,1.),(1.,1.),(1.,1.),(1.,1.),(1.,
1.),(1.,1.),(1.,1.),(1.,1.),(1.,1.),(1.,1.),(1.,1.),(1.,1.),(1.,1.),(1.,
1.),(1.,1.),(1.,1.),(1.,1.),(1.,1.),(1.,1.),(1.,1.),(1.,1.),(1.,1.),(1.,
1.),(1.,1.),(1.,1.),(1.,1.),(1.,1.),(1.,1.),(1.,1.),(1.,1.),(1.,1.),(1.,
1.),(1.,1.),(1.,1.),(1.,1.),(1.,1.),(1.,1.),(1.,1.),(1.,1.),(1.,1.),(1.,
1.),(1.,1.),(1.,1.),(1.,1.),(1.,1.),(1.,1.),(1.,1.),(1.,1.),(1.,1.),(1.,
1.),(1.,1.),(1.,1.),(1.,1.),(1.,1.),(1.,1.),(1.,1.),(1.,1.),(1.,1.),(1.,
1.),(1.,1.)))
REPRESENTATION_ITEM('')
SURFACE()
);
#116=(
BOUNDED_SURFACE()
B_SPLINE_SURFACE(5,1,((#50362,#50363),(#50364,#50365),(#50366,#50367),(#50368,
#50369),(#50370,#50371),(#50372,#50373),(#50374,#50375),(#50376,#50377),
(#50378,#50379),(#50380,#50381),(#50382,#50383),(#50384,#50385),(#50386,
#50387),(#50388,#50389),(#50390,#50391),(#50392,#50393),(#50394,#50395),
(#50396,#50397),(#50398,#50399),(#50400,#50401),(#50402,#50403),(#50404,
#50405),(#50406,#50407),(#50408,#50409),(#50410,#50411),(#50412,#50413),
(#50414,#50415),(#50416,#50417),(#50418,#50419),(#50420,#50421),(#50422,
#50423),(#50424,#50425),(#50426,#50427),(#50428,#50429),(#50430,#50431),
(#50432,#50433),(#50434,#50435),(#50436,#50437),(#50438,#50439),(#50440,
#50441),(#50442,#50443),(#50444,#50445),(#50446,#50447),(#50448,#50449),
(#50450,#50451),(#50452,#50453),(#50454,#50455),(#50456,#50457),(#50458,
#50459),(#50460,#50461),(#50462,#50463),(#50464,#50465),(#50466,#50467),
(#50468,#50469),(#50470,#50471),(#50472,#50473),(#50474,#50475),(#50476,
#50477),(#50478,#50479),(#50480,#50481),(#50482,#50483),(#50484,#50485),
(#50486,#50487),(#50488,#50489),(#50490,#50491),(#50492,#50493),(#50494,
#50495),(#50496,#50497),(#50498,#50499),(#50500,#50501)),.UNSPECIFIED.,
 .F.,.F.,.F.)
B_SPLINE_SURFACE_WITH_KNOTS((6,1,1,1,1,1,1,1,1,1,1,1,1,1,1,1,1,1,1,1,1,
1,1,1,1,1,1,1,1,1,1,1,1,1,1,1,1,1,1,1,1,1,1,1,1,1,1,1,1,1,1,1,1,1,1,1,1,
1,1,1,1,1,1,1,1,6),(2,2),(-1.,-0.984615384615383,-0.969230769230768,-0.953846153846152,
-0.938461538461537,-0.923076923076922,-0.907692307692306,-0.892307692307691,
-0.876923076923076,-0.86153846153846,-0.846153846153845,-0.83076923076923,
-0.815384615384614,-0.799999999999999,-0.784615384615384,-0.769230769230768,
-0.753846153846153,-0.738461538461538,-0.723076923076922,-0.707692307692307,
-0.692307692307692,-0.676923076923076,-0.661538461538461,-0.646153846153846,
-0.63076923076923,-0.615384615384615,-0.6,-0.584615384615384,-0.569230769230769,
-0.553846153846154,-0.538461538461538,-0.523076923076923,-0.507692307692308,
-0.492307692307692,-0.476923076923077,-0.461538461538462,-0.446153846153846,
-0.430769230769231,-0.415384615384615,-0.4,-0.384615384615385,-0.369230769230769,
-0.353846153846154,-0.338461538461538,-0.323076923076923,-0.307692307692308,
-0.292307692307692,-0.276923076923077,-0.261538461538462,-0.246153846153846,
-0.230769230769231,-0.215384615384615,-0.2,-0.184615384615385,-0.169230769230769,
-0.153846153846154,-0.138461538461538,-0.123076923076923,-0.107692307692308,
-0.0923076923076923,-0.0769230769230769,-0.0615384615384615,-0.0461538461538462,
-0.0307692307692308,-0.0153846153846154,0.),(-1.,1.),.UNSPECIFIED.)
GEOMETRIC_REPRESENTATION_ITEM()
RATIONAL_B_SPLINE_SURFACE(((1.,1.),(1.,1.),(1.,1.),(1.,1.),(1.,1.),(1.,
1.),(1.,1.),(1.,1.),(1.,1.),(1.,1.),(1.,1.),(1.,1.),(1.,1.),(1.,1.),(1.,
1.),(1.,1.),(1.,1.),(1.,1.),(1.,1.),(1.,1.),(1.,1.),(1.,1.),(1.,1.),(1.,
1.),(1.,1.),(1.,1.),(1.,1.),(1.,1.),(1.,1.),(1.,1.),(1.,1.),(1.,1.),(1.,
1.),(1.,1.),(1.,1.),(1.,1.),(1.,1.),(1.,1.),(1.,1.),(1.,1.),(1.,1.),(1.,
1.),(1.,1.),(1.,1.),(1.,1.),(1.,1.),(1.,1.),(1.,1.),(1.,1.),(1.,1.),(1.,
1.),(1.,1.),(1.,1.),(1.,1.),(1.,1.),(1.,1.),(1.,1.),(1.,1.),(1.,1.),(1.,
1.),(1.,1.),(1.,1.),(1.,1.),(1.,1.),(1.,1.),(1.,1.),(1.,1.),(1.,1.),(1.,
1.),(1.,1.)))
REPRESENTATION_ITEM('')
SURFACE()
);
#117=(
BOUNDED_SURFACE()
B_SPLINE_SURFACE(5,1,((#50592,#50593),(#50594,#50595),(#50596,#50597),(#50598,
#50599),(#50600,#50601),(#50602,#50603),(#50604,#50605),(#50606,#50607),
(#50608,#50609),(#50610,#50611),(#50612,#50613),(#50614,#50615),(#50616,
#50617),(#50618,#50619),(#50620,#50621),(#50622,#50623),(#50624,#50625),
(#50626,#50627),(#50628,#50629),(#50630,#50631),(#50632,#50633),(#50634,
#50635),(#50636,#50637),(#50638,#50639),(#50640,#50641),(#50642,#50643),
(#50644,#50645),(#50646,#50647),(#50648,#50649),(#50650,#50651),(#50652,
#50653),(#50654,#50655),(#50656,#50657),(#50658,#50659),(#50660,#50661),
(#50662,#50663),(#50664,#50665),(#50666,#50667),(#50668,#50669),(#50670,
#50671),(#50672,#50673),(#50674,#50675),(#50676,#50677),(#50678,#50679),
(#50680,#50681),(#50682,#50683),(#50684,#50685),(#50686,#50687),(#50688,
#50689),(#50690,#50691),(#50692,#50693),(#50694,#50695),(#50696,#50697),
(#50698,#50699),(#50700,#50701),(#50702,#50703),(#50704,#50705),(#50706,
#50707),(#50708,#50709),(#50710,#50711),(#50712,#50713),(#50714,#50715),
(#50716,#50717),(#50718,#50719),(#50720,#50721),(#50722,#50723),(#50724,
#50725),(#50726,#50727),(#50728,#50729),(#50730,#50731)),.UNSPECIFIED.,
 .F.,.F.,.F.)
B_SPLINE_SURFACE_WITH_KNOTS((6,1,1,1,1,1,1,1,1,1,1,1,1,1,1,1,1,1,1,1,1,
1,1,1,1,1,1,1,1,1,1,1,1,1,1,1,1,1,1,1,1,1,1,1,1,1,1,1,1,1,1,1,1,1,1,1,1,
1,1,1,1,1,1,1,1,6),(2,2),(-1.,-0.984615384615383,-0.969230769230768,-0.953846153846152,
-0.938461538461537,-0.923076923076922,-0.907692307692306,-0.892307692307691,
-0.876923076923076,-0.86153846153846,-0.846153846153845,-0.83076923076923,
-0.815384615384614,-0.799999999999999,-0.784615384615384,-0.769230769230768,
-0.753846153846153,-0.738461538461538,-0.723076923076922,-0.707692307692307,
-0.692307692307692,-0.676923076923076,-0.661538461538461,-0.646153846153846,
-0.63076923076923,-0.615384615384615,-0.6,-0.584615384615384,-0.569230769230769,
-0.553846153846154,-0.538461538461538,-0.523076923076923,-0.507692307692308,
-0.492307692307692,-0.476923076923077,-0.461538461538462,-0.446153846153846,
-0.430769230769231,-0.415384615384615,-0.4,-0.384615384615385,-0.369230769230769,
-0.353846153846154,-0.338461538461538,-0.323076923076923,-0.307692307692308,
-0.292307692307692,-0.276923076923077,-0.261538461538462,-0.246153846153846,
-0.230769230769231,-0.215384615384615,-0.2,-0.184615384615385,-0.169230769230769,
-0.153846153846154,-0.138461538461538,-0.123076923076923,-0.107692307692308,
-0.0923076923076923,-0.0769230769230769,-0.0615384615384615,-0.0461538461538462,
-0.0307692307692308,-0.0153846153846154,0.),(-1.,1.),.UNSPECIFIED.)
GEOMETRIC_REPRESENTATION_ITEM()
RATIONAL_B_SPLINE_SURFACE(((1.,1.),(1.,1.),(1.,1.),(1.,1.),(1.,1.),(1.,
1.),(1.,1.),(1.,1.),(1.,1.),(1.,1.),(1.,1.),(1.,1.),(1.,1.),(1.,1.),(1.,
1.),(1.,1.),(1.,1.),(1.,1.),(1.,1.),(1.,1.),(1.,1.),(1.,1.),(1.,1.),(1.,
1.),(1.,1.),(1.,1.),(1.,1.),(1.,1.),(1.,1.),(1.,1.),(1.,1.),(1.,1.),(1.,
1.),(1.,1.),(1.,1.),(1.,1.),(1.,1.),(1.,1.),(1.,1.),(1.,1.),(1.,1.),(1.,
1.),(1.,1.),(1.,1.),(1.,1.),(1.,1.),(1.,1.),(1.,1.),(1.,1.),(1.,1.),(1.,
1.),(1.,1.),(1.,1.),(1.,1.),(1.,1.),(1.,1.),(1.,1.),(1.,1.),(1.,1.),(1.,
1.),(1.,1.),(1.,1.),(1.,1.),(1.,1.),(1.,1.),(1.,1.),(1.,1.),(1.,1.),(1.,
1.),(1.,1.)))
REPRESENTATION_ITEM('')
SURFACE()
);
#118=(
BOUNDED_SURFACE()
B_SPLINE_SURFACE(5,1,((#50804,#50805),(#50806,#50807),(#50808,#50809),(#50810,
#50811),(#50812,#50813),(#50814,#50815),(#50816,#50817),(#50818,#50819),
(#50820,#50821),(#50822,#50823),(#50824,#50825),(#50826,#50827),(#50828,
#50829),(#50830,#50831),(#50832,#50833),(#50834,#50835),(#50836,#50837),
(#50838,#50839),(#50840,#50841),(#50842,#50843),(#50844,#50845),(#50846,
#50847),(#50848,#50849),(#50850,#50851),(#50852,#50853),(#50854,#50855),
(#50856,#50857),(#50858,#50859),(#50860,#50861),(#50862,#50863),(#50864,
#50865),(#50866,#50867),(#50868,#50869),(#50870,#50871),(#50872,#50873),
(#50874,#50875),(#50876,#50877),(#50878,#50879),(#50880,#50881),(#50882,
#50883),(#50884,#50885),(#50886,#50887),(#50888,#50889),(#50890,#50891),
(#50892,#50893),(#50894,#50895),(#50896,#50897),(#50898,#50899),(#50900,
#50901),(#50902,#50903),(#50904,#50905),(#50906,#50907),(#50908,#50909),
(#50910,#50911),(#50912,#50913),(#50914,#50915),(#50916,#50917),(#50918,
#50919),(#50920,#50921),(#50922,#50923),(#50924,#50925),(#50926,#50927),
(#50928,#50929),(#50930,#50931),(#50932,#50933),(#50934,#50935),(#50936,
#50937),(#50938,#50939),(#50940,#50941),(#50942,#50943)),.UNSPECIFIED.,
 .F.,.F.,.F.)
B_SPLINE_SURFACE_WITH_KNOTS((6,1,1,1,1,1,1,1,1,1,1,1,1,1,1,1,1,1,1,1,1,
1,1,1,1,1,1,1,1,1,1,1,1,1,1,1,1,1,1,1,1,1,1,1,1,1,1,1,1,1,1,1,1,1,1,1,1,
1,1,1,1,1,1,1,1,6),(2,2),(-1.,-0.984615384615383,-0.969230769230768,-0.953846153846152,
-0.938461538461537,-0.923076923076922,-0.907692307692306,-0.892307692307691,
-0.876923076923076,-0.86153846153846,-0.846153846153845,-0.83076923076923,
-0.815384615384614,-0.799999999999999,-0.784615384615384,-0.769230769230768,
-0.753846153846153,-0.738461538461538,-0.723076923076922,-0.707692307692307,
-0.692307692307692,-0.676923076923076,-0.661538461538461,-0.646153846153846,
-0.63076923076923,-0.615384615384615,-0.6,-0.584615384615384,-0.569230769230769,
-0.553846153846154,-0.538461538461538,-0.523076923076923,-0.507692307692308,
-0.492307692307692,-0.476923076923077,-0.461538461538462,-0.446153846153846,
-0.430769230769231,-0.415384615384615,-0.4,-0.384615384615385,-0.369230769230769,
-0.353846153846154,-0.338461538461538,-0.323076923076923,-0.307692307692308,
-0.292307692307692,-0.276923076923077,-0.261538461538462,-0.246153846153846,
-0.230769230769231,-0.215384615384615,-0.2,-0.184615384615385,-0.169230769230769,
-0.153846153846154,-0.138461538461538,-0.123076923076923,-0.107692307692308,
-0.0923076923076923,-0.0769230769230769,-0.0615384615384615,-0.0461538461538462,
-0.0307692307692308,-0.0153846153846154,0.),(-1.,1.),.UNSPECIFIED.)
GEOMETRIC_REPRESENTATION_ITEM()
RATIONAL_B_SPLINE_SURFACE(((1.,1.),(1.,1.),(1.,1.),(1.,1.),(1.,1.),(1.,
1.),(1.,1.),(1.,1.),(1.,1.),(1.,1.),(1.,1.),(1.,1.),(1.,1.),(1.,1.),(1.,
1.),(1.,1.),(1.,1.),(1.,1.),(1.,1.),(1.,1.),(1.,1.),(1.,1.),(1.,1.),(1.,
1.),(1.,1.),(1.,1.),(1.,1.),(1.,1.),(1.,1.),(1.,1.),(1.,1.),(1.,1.),(1.,
1.),(1.,1.),(1.,1.),(1.,1.),(1.,1.),(1.,1.),(1.,1.),(1.,1.),(1.,1.),(1.,
1.),(1.,1.),(1.,1.),(1.,1.),(1.,1.),(1.,1.),(1.,1.),(1.,1.),(1.,1.),(1.,
1.),(1.,1.),(1.,1.),(1.,1.),(1.,1.),(1.,1.),(1.,1.),(1.,1.),(1.,1.),(1.,
1.),(1.,1.),(1.,1.),(1.,1.),(1.,1.),(1.,1.),(1.,1.),(1.,1.),(1.,1.),(1.,
1.),(1.,1.)))
REPRESENTATION_ITEM('')
SURFACE()
);
#119=(
BOUNDED_SURFACE()
B_SPLINE_SURFACE(5,1,((#51034,#51035),(#51036,#51037),(#51038,#51039),(#51040,
#51041),(#51042,#51043),(#51044,#51045),(#51046,#51047),(#51048,#51049),
(#51050,#51051),(#51052,#51053),(#51054,#51055),(#51056,#51057),(#51058,
#51059),(#51060,#51061),(#51062,#51063),(#51064,#51065),(#51066,#51067),
(#51068,#51069),(#51070,#51071),(#51072,#51073),(#51074,#51075),(#51076,
#51077),(#51078,#51079),(#51080,#51081),(#51082,#51083),(#51084,#51085),
(#51086,#51087),(#51088,#51089),(#51090,#51091),(#51092,#51093),(#51094,
#51095),(#51096,#51097),(#51098,#51099),(#51100,#51101),(#51102,#51103),
(#51104,#51105),(#51106,#51107),(#51108,#51109),(#51110,#51111),(#51112,
#51113),(#51114,#51115),(#51116,#51117),(#51118,#51119),(#51120,#51121),
(#51122,#51123),(#51124,#51125),(#51126,#51127),(#51128,#51129),(#51130,
#51131),(#51132,#51133),(#51134,#51135),(#51136,#51137),(#51138,#51139),
(#51140,#51141),(#51142,#51143),(#51144,#51145),(#51146,#51147),(#51148,
#51149),(#51150,#51151),(#51152,#51153),(#51154,#51155),(#51156,#51157),
(#51158,#51159),(#51160,#51161),(#51162,#51163),(#51164,#51165),(#51166,
#51167),(#51168,#51169),(#51170,#51171),(#51172,#51173)),.UNSPECIFIED.,
 .F.,.F.,.F.)
B_SPLINE_SURFACE_WITH_KNOTS((6,1,1,1,1,1,1,1,1,1,1,1,1,1,1,1,1,1,1,1,1,
1,1,1,1,1,1,1,1,1,1,1,1,1,1,1,1,1,1,1,1,1,1,1,1,1,1,1,1,1,1,1,1,1,1,1,1,
1,1,1,1,1,1,1,1,6),(2,2),(-1.,-0.984615384615383,-0.969230769230768,-0.953846153846152,
-0.938461538461537,-0.923076923076922,-0.907692307692306,-0.892307692307691,
-0.876923076923076,-0.86153846153846,-0.846153846153845,-0.83076923076923,
-0.815384615384614,-0.799999999999999,-0.784615384615384,-0.769230769230768,
-0.753846153846153,-0.738461538461538,-0.723076923076922,-0.707692307692307,
-0.692307692307692,-0.676923076923076,-0.661538461538461,-0.646153846153846,
-0.63076923076923,-0.615384615384615,-0.6,-0.584615384615384,-0.569230769230769,
-0.553846153846154,-0.538461538461538,-0.523076923076923,-0.507692307692308,
-0.492307692307692,-0.476923076923077,-0.461538461538462,-0.446153846153846,
-0.430769230769231,-0.415384615384615,-0.4,-0.384615384615385,-0.369230769230769,
-0.353846153846154,-0.338461538461538,-0.323076923076923,-0.307692307692308,
-0.292307692307692,-0.276923076923077,-0.261538461538462,-0.246153846153846,
-0.230769230769231,-0.215384615384615,-0.2,-0.184615384615385,-0.169230769230769,
-0.153846153846154,-0.138461538461538,-0.123076923076923,-0.107692307692308,
-0.0923076923076923,-0.0769230769230769,-0.0615384615384615,-0.0461538461538462,
-0.0307692307692308,-0.0153846153846154,0.),(-1.,1.),.UNSPECIFIED.)
GEOMETRIC_REPRESENTATION_ITEM()
RATIONAL_B_SPLINE_SURFACE(((1.,1.),(1.,1.),(1.,1.),(1.,1.),(1.,1.),(1.,
1.),(1.,1.),(1.,1.),(1.,1.),(1.,1.),(1.,1.),(1.,1.),(1.,1.),(1.,1.),(1.,
1.),(1.,1.),(1.,1.),(1.,1.),(1.,1.),(1.,1.),(1.,1.),(1.,1.),(1.,1.),(1.,
1.),(1.,1.),(1.,1.),(1.,1.),(1.,1.),(1.,1.),(1.,1.),(1.,1.),(1.,1.),(1.,
1.),(1.,1.),(1.,1.),(1.,1.),(1.,1.),(1.,1.),(1.,1.),(1.,1.),(1.,1.),(1.,
1.),(1.,1.),(1.,1.),(1.,1.),(1.,1.),(1.,1.),(1.,1.),(1.,1.),(1.,1.),(1.,
1.),(1.,1.),(1.,1.),(1.,1.),(1.,1.),(1.,1.),(1.,1.),(1.,1.),(1.,1.),(1.,
1.),(1.,1.),(1.,1.),(1.,1.),(1.,1.),(1.,1.),(1.,1.),(1.,1.),(1.,1.),(1.,
1.),(1.,1.)))
REPRESENTATION_ITEM('')
SURFACE()
);
#120=(
BOUNDED_SURFACE()
B_SPLINE_SURFACE(5,1,((#51246,#51247),(#51248,#51249),(#51250,#51251),(#51252,
#51253),(#51254,#51255),(#51256,#51257),(#51258,#51259),(#51260,#51261),
(#51262,#51263),(#51264,#51265),(#51266,#51267),(#51268,#51269),(#51270,
#51271),(#51272,#51273),(#51274,#51275),(#51276,#51277),(#51278,#51279),
(#51280,#51281),(#51282,#51283),(#51284,#51285),(#51286,#51287),(#51288,
#51289),(#51290,#51291),(#51292,#51293),(#51294,#51295),(#51296,#51297),
(#51298,#51299),(#51300,#51301),(#51302,#51303),(#51304,#51305),(#51306,
#51307),(#51308,#51309),(#51310,#51311),(#51312,#51313),(#51314,#51315),
(#51316,#51317),(#51318,#51319),(#51320,#51321),(#51322,#51323),(#51324,
#51325),(#51326,#51327),(#51328,#51329),(#51330,#51331),(#51332,#51333),
(#51334,#51335),(#51336,#51337),(#51338,#51339),(#51340,#51341),(#51342,
#51343),(#51344,#51345),(#51346,#51347),(#51348,#51349),(#51350,#51351),
(#51352,#51353),(#51354,#51355),(#51356,#51357),(#51358,#51359),(#51360,
#51361),(#51362,#51363),(#51364,#51365),(#51366,#51367),(#51368,#51369),
(#51370,#51371),(#51372,#51373),(#51374,#51375),(#51376,#51377),(#51378,
#51379),(#51380,#51381),(#51382,#51383),(#51384,#51385)),.UNSPECIFIED.,
 .F.,.F.,.F.)
B_SPLINE_SURFACE_WITH_KNOTS((6,1,1,1,1,1,1,1,1,1,1,1,1,1,1,1,1,1,1,1,1,
1,1,1,1,1,1,1,1,1,1,1,1,1,1,1,1,1,1,1,1,1,1,1,1,1,1,1,1,1,1,1,1,1,1,1,1,
1,1,1,1,1,1,1,1,6),(2,2),(-1.,-0.984615384615383,-0.969230769230768,-0.953846153846152,
-0.938461538461537,-0.923076923076922,-0.907692307692306,-0.892307692307691,
-0.876923076923076,-0.86153846153846,-0.846153846153845,-0.83076923076923,
-0.815384615384614,-0.799999999999999,-0.784615384615384,-0.769230769230768,
-0.753846153846153,-0.738461538461538,-0.723076923076922,-0.707692307692307,
-0.692307692307692,-0.676923076923076,-0.661538461538461,-0.646153846153846,
-0.63076923076923,-0.615384615384615,-0.6,-0.584615384615384,-0.569230769230769,
-0.553846153846154,-0.538461538461538,-0.523076923076923,-0.507692307692308,
-0.492307692307692,-0.476923076923077,-0.461538461538462,-0.446153846153846,
-0.430769230769231,-0.415384615384615,-0.4,-0.384615384615385,-0.369230769230769,
-0.353846153846154,-0.338461538461538,-0.323076923076923,-0.307692307692308,
-0.292307692307692,-0.276923076923077,-0.261538461538462,-0.246153846153846,
-0.230769230769231,-0.215384615384615,-0.2,-0.184615384615385,-0.169230769230769,
-0.153846153846154,-0.138461538461538,-0.123076923076923,-0.107692307692308,
-0.0923076923076923,-0.0769230769230769,-0.0615384615384615,-0.0461538461538462,
-0.0307692307692308,-0.0153846153846154,0.),(-1.,1.),.UNSPECIFIED.)
GEOMETRIC_REPRESENTATION_ITEM()
RATIONAL_B_SPLINE_SURFACE(((1.,1.),(1.,1.),(1.,1.),(1.,1.),(1.,1.),(1.,
1.),(1.,1.),(1.,1.),(1.,1.),(1.,1.),(1.,1.),(1.,1.),(1.,1.),(1.,1.),(1.,
1.),(1.,1.),(1.,1.),(1.,1.),(1.,1.),(1.,1.),(1.,1.),(1.,1.),(1.,1.),(1.,
1.),(1.,1.),(1.,1.),(1.,1.),(1.,1.),(1.,1.),(1.,1.),(1.,1.),(1.,1.),(1.,
1.),(1.,1.),(1.,1.),(1.,1.),(1.,1.),(1.,1.),(1.,1.),(1.,1.),(1.,1.),(1.,
1.),(1.,1.),(1.,1.),(1.,1.),(1.,1.),(1.,1.),(1.,1.),(1.,1.),(1.,1.),(1.,
1.),(1.,1.),(1.,1.),(1.,1.),(1.,1.),(1.,1.),(1.,1.),(1.,1.),(1.,1.),(1.,
1.),(1.,1.),(1.,1.),(1.,1.),(1.,1.),(1.,1.),(1.,1.),(1.,1.),(1.,1.),(1.,
1.),(1.,1.)))
REPRESENTATION_ITEM('')
SURFACE()
);
#121=(
BOUNDED_SURFACE()
B_SPLINE_SURFACE(5,1,((#51476,#51477),(#51478,#51479),(#51480,#51481),(#51482,
#51483),(#51484,#51485),(#51486,#51487),(#51488,#51489),(#51490,#51491),
(#51492,#51493),(#51494,#51495),(#51496,#51497),(#51498,#51499),(#51500,
#51501),(#51502,#51503),(#51504,#51505),(#51506,#51507),(#51508,#51509),
(#51510,#51511),(#51512,#51513),(#51514,#51515),(#51516,#51517),(#51518,
#51519),(#51520,#51521),(#51522,#51523),(#51524,#51525),(#51526,#51527),
(#51528,#51529),(#51530,#51531),(#51532,#51533),(#51534,#51535),(#51536,
#51537),(#51538,#51539),(#51540,#51541),(#51542,#51543),(#51544,#51545),
(#51546,#51547),(#51548,#51549),(#51550,#51551),(#51552,#51553),(#51554,
#51555),(#51556,#51557),(#51558,#51559),(#51560,#51561),(#51562,#51563),
(#51564,#51565),(#51566,#51567),(#51568,#51569),(#51570,#51571),(#51572,
#51573),(#51574,#51575),(#51576,#51577),(#51578,#51579),(#51580,#51581),
(#51582,#51583),(#51584,#51585),(#51586,#51587),(#51588,#51589),(#51590,
#51591),(#51592,#51593),(#51594,#51595),(#51596,#51597),(#51598,#51599),
(#51600,#51601),(#51602,#51603),(#51604,#51605),(#51606,#51607),(#51608,
#51609),(#51610,#51611),(#51612,#51613),(#51614,#51615)),.UNSPECIFIED.,
 .F.,.F.,.F.)
B_SPLINE_SURFACE_WITH_KNOTS((6,1,1,1,1,1,1,1,1,1,1,1,1,1,1,1,1,1,1,1,1,
1,1,1,1,1,1,1,1,1,1,1,1,1,1,1,1,1,1,1,1,1,1,1,1,1,1,1,1,1,1,1,1,1,1,1,1,
1,1,1,1,1,1,1,1,6),(2,2),(-1.,-0.984615384615383,-0.969230769230768,-0.953846153846152,
-0.938461538461537,-0.923076923076922,-0.907692307692306,-0.892307692307691,
-0.876923076923076,-0.86153846153846,-0.846153846153845,-0.83076923076923,
-0.815384615384614,-0.799999999999999,-0.784615384615384,-0.769230769230768,
-0.753846153846153,-0.738461538461538,-0.723076923076922,-0.707692307692307,
-0.692307692307692,-0.676923076923076,-0.661538461538461,-0.646153846153846,
-0.63076923076923,-0.615384615384615,-0.6,-0.584615384615384,-0.569230769230769,
-0.553846153846154,-0.538461538461538,-0.523076923076923,-0.507692307692308,
-0.492307692307692,-0.476923076923077,-0.461538461538462,-0.446153846153846,
-0.430769230769231,-0.415384615384615,-0.4,-0.384615384615385,-0.369230769230769,
-0.353846153846154,-0.338461538461538,-0.323076923076923,-0.307692307692308,
-0.292307692307692,-0.276923076923077,-0.261538461538462,-0.246153846153846,
-0.230769230769231,-0.215384615384615,-0.2,-0.184615384615385,-0.169230769230769,
-0.153846153846154,-0.138461538461538,-0.123076923076923,-0.107692307692308,
-0.0923076923076923,-0.0769230769230769,-0.0615384615384615,-0.0461538461538462,
-0.0307692307692308,-0.0153846153846154,0.),(-1.,1.),.UNSPECIFIED.)
GEOMETRIC_REPRESENTATION_ITEM()
RATIONAL_B_SPLINE_SURFACE(((1.,1.),(1.,1.),(1.,1.),(1.,1.),(1.,1.),(1.,
1.),(1.,1.),(1.,1.),(1.,1.),(1.,1.),(1.,1.),(1.,1.),(1.,1.),(1.,1.),(1.,
1.),(1.,1.),(1.,1.),(1.,1.),(1.,1.),(1.,1.),(1.,1.),(1.,1.),(1.,1.),(1.,
1.),(1.,1.),(1.,1.),(1.,1.),(1.,1.),(1.,1.),(1.,1.),(1.,1.),(1.,1.),(1.,
1.),(1.,1.),(1.,1.),(1.,1.),(1.,1.),(1.,1.),(1.,1.),(1.,1.),(1.,1.),(1.,
1.),(1.,1.),(1.,1.),(1.,1.),(1.,1.),(1.,1.),(1.,1.),(1.,1.),(1.,1.),(1.,
1.),(1.,1.),(1.,1.),(1.,1.),(1.,1.),(1.,1.),(1.,1.),(1.,1.),(1.,1.),(1.,
1.),(1.,1.),(1.,1.),(1.,1.),(1.,1.),(1.,1.),(1.,1.),(1.,1.),(1.,1.),(1.,
1.),(1.,1.)))
REPRESENTATION_ITEM('')
SURFACE()
);
#122=(
BOUNDED_SURFACE()
B_SPLINE_SURFACE(5,1,((#51688,#51689),(#51690,#51691),(#51692,#51693),(#51694,
#51695),(#51696,#51697),(#51698,#51699),(#51700,#51701),(#51702,#51703),
(#51704,#51705),(#51706,#51707),(#51708,#51709),(#51710,#51711),(#51712,
#51713),(#51714,#51715),(#51716,#51717),(#51718,#51719),(#51720,#51721),
(#51722,#51723),(#51724,#51725),(#51726,#51727),(#51728,#51729),(#51730,
#51731),(#51732,#51733),(#51734,#51735),(#51736,#51737),(#51738,#51739),
(#51740,#51741),(#51742,#51743),(#51744,#51745),(#51746,#51747),(#51748,
#51749),(#51750,#51751),(#51752,#51753),(#51754,#51755),(#51756,#51757),
(#51758,#51759),(#51760,#51761),(#51762,#51763),(#51764,#51765),(#51766,
#51767),(#51768,#51769),(#51770,#51771),(#51772,#51773),(#51774,#51775),
(#51776,#51777),(#51778,#51779),(#51780,#51781),(#51782,#51783),(#51784,
#51785),(#51786,#51787),(#51788,#51789),(#51790,#51791),(#51792,#51793),
(#51794,#51795),(#51796,#51797),(#51798,#51799),(#51800,#51801),(#51802,
#51803),(#51804,#51805),(#51806,#51807),(#51808,#51809),(#51810,#51811),
(#51812,#51813),(#51814,#51815),(#51816,#51817),(#51818,#51819),(#51820,
#51821),(#51822,#51823),(#51824,#51825),(#51826,#51827)),.UNSPECIFIED.,
 .F.,.F.,.F.)
B_SPLINE_SURFACE_WITH_KNOTS((6,1,1,1,1,1,1,1,1,1,1,1,1,1,1,1,1,1,1,1,1,
1,1,1,1,1,1,1,1,1,1,1,1,1,1,1,1,1,1,1,1,1,1,1,1,1,1,1,1,1,1,1,1,1,1,1,1,
1,1,1,1,1,1,1,1,6),(2,2),(-1.,-0.984615384615383,-0.969230769230768,-0.953846153846152,
-0.938461538461537,-0.923076923076922,-0.907692307692306,-0.892307692307691,
-0.876923076923076,-0.86153846153846,-0.846153846153845,-0.83076923076923,
-0.815384615384614,-0.799999999999999,-0.784615384615384,-0.769230769230768,
-0.753846153846153,-0.738461538461538,-0.723076923076922,-0.707692307692307,
-0.692307692307692,-0.676923076923076,-0.661538461538461,-0.646153846153846,
-0.63076923076923,-0.615384615384615,-0.6,-0.584615384615384,-0.569230769230769,
-0.553846153846154,-0.538461538461538,-0.523076923076923,-0.507692307692308,
-0.492307692307692,-0.476923076923077,-0.461538461538462,-0.446153846153846,
-0.430769230769231,-0.415384615384615,-0.4,-0.384615384615385,-0.369230769230769,
-0.353846153846154,-0.338461538461538,-0.323076923076923,-0.307692307692308,
-0.292307692307692,-0.276923076923077,-0.261538461538462,-0.246153846153846,
-0.230769230769231,-0.215384615384615,-0.2,-0.184615384615385,-0.169230769230769,
-0.153846153846154,-0.138461538461538,-0.123076923076923,-0.107692307692308,
-0.0923076923076923,-0.0769230769230769,-0.0615384615384615,-0.0461538461538462,
-0.0307692307692308,-0.0153846153846154,0.),(-1.,1.),.UNSPECIFIED.)
GEOMETRIC_REPRESENTATION_ITEM()
RATIONAL_B_SPLINE_SURFACE(((1.,1.),(1.,1.),(1.,1.),(1.,1.),(1.,1.),(1.,
1.),(1.,1.),(1.,1.),(1.,1.),(1.,1.),(1.,1.),(1.,1.),(1.,1.),(1.,1.),(1.,
1.),(1.,1.),(1.,1.),(1.,1.),(1.,1.),(1.,1.),(1.,1.),(1.,1.),(1.,1.),(1.,
1.),(1.,1.),(1.,1.),(1.,1.),(1.,1.),(1.,1.),(1.,1.),(1.,1.),(1.,1.),(1.,
1.),(1.,1.),(1.,1.),(1.,1.),(1.,1.),(1.,1.),(1.,1.),(1.,1.),(1.,1.),(1.,
1.),(1.,1.),(1.,1.),(1.,1.),(1.,1.),(1.,1.),(1.,1.),(1.,1.),(1.,1.),(1.,
1.),(1.,1.),(1.,1.),(1.,1.),(1.,1.),(1.,1.),(1.,1.),(1.,1.),(1.,1.),(1.,
1.),(1.,1.),(1.,1.),(1.,1.),(1.,1.),(1.,1.),(1.,1.),(1.,1.),(1.,1.),(1.,
1.),(1.,1.)))
REPRESENTATION_ITEM('')
SURFACE()
);
#123=(
BOUNDED_SURFACE()
B_SPLINE_SURFACE(5,1,((#51918,#51919),(#51920,#51921),(#51922,#51923),(#51924,
#51925),(#51926,#51927),(#51928,#51929),(#51930,#51931),(#51932,#51933),
(#51934,#51935),(#51936,#51937),(#51938,#51939),(#51940,#51941),(#51942,
#51943),(#51944,#51945),(#51946,#51947),(#51948,#51949),(#51950,#51951),
(#51952,#51953),(#51954,#51955),(#51956,#51957),(#51958,#51959),(#51960,
#51961),(#51962,#51963),(#51964,#51965),(#51966,#51967),(#51968,#51969),
(#51970,#51971),(#51972,#51973),(#51974,#51975),(#51976,#51977),(#51978,
#51979),(#51980,#51981),(#51982,#51983),(#51984,#51985),(#51986,#51987),
(#51988,#51989),(#51990,#51991),(#51992,#51993),(#51994,#51995),(#51996,
#51997),(#51998,#51999),(#52000,#52001),(#52002,#52003),(#52004,#52005),
(#52006,#52007),(#52008,#52009),(#52010,#52011),(#52012,#52013),(#52014,
#52015),(#52016,#52017),(#52018,#52019),(#52020,#52021),(#52022,#52023),
(#52024,#52025),(#52026,#52027),(#52028,#52029),(#52030,#52031),(#52032,
#52033),(#52034,#52035),(#52036,#52037),(#52038,#52039),(#52040,#52041),
(#52042,#52043),(#52044,#52045),(#52046,#52047),(#52048,#52049),(#52050,
#52051),(#52052,#52053),(#52054,#52055),(#52056,#52057)),.UNSPECIFIED.,
 .F.,.F.,.F.)
B_SPLINE_SURFACE_WITH_KNOTS((6,1,1,1,1,1,1,1,1,1,1,1,1,1,1,1,1,1,1,1,1,
1,1,1,1,1,1,1,1,1,1,1,1,1,1,1,1,1,1,1,1,1,1,1,1,1,1,1,1,1,1,1,1,1,1,1,1,
1,1,1,1,1,1,1,1,6),(2,2),(-1.,-0.984615384615383,-0.969230769230768,-0.953846153846152,
-0.938461538461537,-0.923076923076922,-0.907692307692306,-0.892307692307691,
-0.876923076923076,-0.86153846153846,-0.846153846153845,-0.83076923076923,
-0.815384615384614,-0.799999999999999,-0.784615384615384,-0.769230769230768,
-0.753846153846153,-0.738461538461538,-0.723076923076922,-0.707692307692307,
-0.692307692307692,-0.676923076923076,-0.661538461538461,-0.646153846153846,
-0.63076923076923,-0.615384615384615,-0.6,-0.584615384615384,-0.569230769230769,
-0.553846153846154,-0.538461538461538,-0.523076923076923,-0.507692307692308,
-0.492307692307692,-0.476923076923077,-0.461538461538462,-0.446153846153846,
-0.430769230769231,-0.415384615384615,-0.4,-0.384615384615385,-0.369230769230769,
-0.353846153846154,-0.338461538461538,-0.323076923076923,-0.307692307692308,
-0.292307692307692,-0.276923076923077,-0.261538461538462,-0.246153846153846,
-0.230769230769231,-0.215384615384615,-0.2,-0.184615384615385,-0.169230769230769,
-0.153846153846154,-0.138461538461538,-0.123076923076923,-0.107692307692308,
-0.0923076923076923,-0.0769230769230769,-0.0615384615384615,-0.0461538461538462,
-0.0307692307692308,-0.0153846153846154,0.),(-1.,1.),.UNSPECIFIED.)
GEOMETRIC_REPRESENTATION_ITEM()
RATIONAL_B_SPLINE_SURFACE(((1.,1.),(1.,1.),(1.,1.),(1.,1.),(1.,1.),(1.,
1.),(1.,1.),(1.,1.),(1.,1.),(1.,1.),(1.,1.),(1.,1.),(1.,1.),(1.,1.),(1.,
1.),(1.,1.),(1.,1.),(1.,1.),(1.,1.),(1.,1.),(1.,1.),(1.,1.),(1.,1.),(1.,
1.),(1.,1.),(1.,1.),(1.,1.),(1.,1.),(1.,1.),(1.,1.),(1.,1.),(1.,1.),(1.,
1.),(1.,1.),(1.,1.),(1.,1.),(1.,1.),(1.,1.),(1.,1.),(1.,1.),(1.,1.),(1.,
1.),(1.,1.),(1.,1.),(1.,1.),(1.,1.),(1.,1.),(1.,1.),(1.,1.),(1.,1.),(1.,
1.),(1.,1.),(1.,1.),(1.,1.),(1.,1.),(1.,1.),(1.,1.),(1.,1.),(1.,1.),(1.,
1.),(1.,1.),(1.,1.),(1.,1.),(1.,1.),(1.,1.),(1.,1.),(1.,1.),(1.,1.),(1.,
1.),(1.,1.)))
REPRESENTATION_ITEM('')
SURFACE()
);
#124=(
BOUNDED_SURFACE()
B_SPLINE_SURFACE(5,1,((#52130,#52131),(#52132,#52133),(#52134,#52135),(#52136,
#52137),(#52138,#52139),(#52140,#52141),(#52142,#52143),(#52144,#52145),
(#52146,#52147),(#52148,#52149),(#52150,#52151),(#52152,#52153),(#52154,
#52155),(#52156,#52157),(#52158,#52159),(#52160,#52161),(#52162,#52163),
(#52164,#52165),(#52166,#52167),(#52168,#52169),(#52170,#52171),(#52172,
#52173),(#52174,#52175),(#52176,#52177),(#52178,#52179),(#52180,#52181),
(#52182,#52183),(#52184,#52185),(#52186,#52187),(#52188,#52189),(#52190,
#52191),(#52192,#52193),(#52194,#52195),(#52196,#52197),(#52198,#52199),
(#52200,#52201),(#52202,#52203),(#52204,#52205),(#52206,#52207),(#52208,
#52209),(#52210,#52211),(#52212,#52213),(#52214,#52215),(#52216,#52217),
(#52218,#52219),(#52220,#52221),(#52222,#52223),(#52224,#52225),(#52226,
#52227),(#52228,#52229),(#52230,#52231),(#52232,#52233),(#52234,#52235),
(#52236,#52237),(#52238,#52239),(#52240,#52241),(#52242,#52243),(#52244,
#52245),(#52246,#52247),(#52248,#52249),(#52250,#52251),(#52252,#52253),
(#52254,#52255),(#52256,#52257),(#52258,#52259),(#52260,#52261),(#52262,
#52263),(#52264,#52265),(#52266,#52267),(#52268,#52269)),.UNSPECIFIED.,
 .F.,.F.,.F.)
B_SPLINE_SURFACE_WITH_KNOTS((6,1,1,1,1,1,1,1,1,1,1,1,1,1,1,1,1,1,1,1,1,
1,1,1,1,1,1,1,1,1,1,1,1,1,1,1,1,1,1,1,1,1,1,1,1,1,1,1,1,1,1,1,1,1,1,1,1,
1,1,1,1,1,1,1,1,6),(2,2),(-1.,-0.984615384615383,-0.969230769230768,-0.953846153846152,
-0.938461538461537,-0.923076923076922,-0.907692307692306,-0.892307692307691,
-0.876923076923076,-0.86153846153846,-0.846153846153845,-0.83076923076923,
-0.815384615384614,-0.799999999999999,-0.784615384615384,-0.769230769230768,
-0.753846153846153,-0.738461538461538,-0.723076923076922,-0.707692307692307,
-0.692307692307692,-0.676923076923076,-0.661538461538461,-0.646153846153846,
-0.63076923076923,-0.615384615384615,-0.6,-0.584615384615384,-0.569230769230769,
-0.553846153846154,-0.538461538461538,-0.523076923076923,-0.507692307692308,
-0.492307692307692,-0.476923076923077,-0.461538461538462,-0.446153846153846,
-0.430769230769231,-0.415384615384615,-0.4,-0.384615384615385,-0.369230769230769,
-0.353846153846154,-0.338461538461538,-0.323076923076923,-0.307692307692308,
-0.292307692307692,-0.276923076923077,-0.261538461538462,-0.246153846153846,
-0.230769230769231,-0.215384615384615,-0.2,-0.184615384615385,-0.169230769230769,
-0.153846153846154,-0.138461538461538,-0.123076923076923,-0.107692307692308,
-0.0923076923076923,-0.0769230769230769,-0.0615384615384615,-0.0461538461538462,
-0.0307692307692308,-0.0153846153846154,0.),(-1.,1.),.UNSPECIFIED.)
GEOMETRIC_REPRESENTATION_ITEM()
RATIONAL_B_SPLINE_SURFACE(((1.,1.),(1.,1.),(1.,1.),(1.,1.),(1.,1.),(1.,
1.),(1.,1.),(1.,1.),(1.,1.),(1.,1.),(1.,1.),(1.,1.),(1.,1.),(1.,1.),(1.,
1.),(1.,1.),(1.,1.),(1.,1.),(1.,1.),(1.,1.),(1.,1.),(1.,1.),(1.,1.),(1.,
1.),(1.,1.),(1.,1.),(1.,1.),(1.,1.),(1.,1.),(1.,1.),(1.,1.),(1.,1.),(1.,
1.),(1.,1.),(1.,1.),(1.,1.),(1.,1.),(1.,1.),(1.,1.),(1.,1.),(1.,1.),(1.,
1.),(1.,1.),(1.,1.),(1.,1.),(1.,1.),(1.,1.),(1.,1.),(1.,1.),(1.,1.),(1.,
1.),(1.,1.),(1.,1.),(1.,1.),(1.,1.),(1.,1.),(1.,1.),(1.,1.),(1.,1.),(1.,
1.),(1.,1.),(1.,1.),(1.,1.),(1.,1.),(1.,1.),(1.,1.),(1.,1.),(1.,1.),(1.,
1.),(1.,1.)))
REPRESENTATION_ITEM('')
SURFACE()
);
#125=(
BOUNDED_SURFACE()
B_SPLINE_SURFACE(5,1,((#52360,#52361),(#52362,#52363),(#52364,#52365),(#52366,
#52367),(#52368,#52369),(#52370,#52371),(#52372,#52373),(#52374,#52375),
(#52376,#52377),(#52378,#52379),(#52380,#52381),(#52382,#52383),(#52384,
#52385),(#52386,#52387),(#52388,#52389),(#52390,#52391),(#52392,#52393),
(#52394,#52395),(#52396,#52397),(#52398,#52399),(#52400,#52401),(#52402,
#52403),(#52404,#52405),(#52406,#52407),(#52408,#52409),(#52410,#52411),
(#52412,#52413),(#52414,#52415),(#52416,#52417),(#52418,#52419),(#52420,
#52421),(#52422,#52423),(#52424,#52425),(#52426,#52427),(#52428,#52429),
(#52430,#52431),(#52432,#52433),(#52434,#52435),(#52436,#52437),(#52438,
#52439),(#52440,#52441),(#52442,#52443),(#52444,#52445),(#52446,#52447),
(#52448,#52449),(#52450,#52451),(#52452,#52453),(#52454,#52455),(#52456,
#52457),(#52458,#52459),(#52460,#52461),(#52462,#52463),(#52464,#52465),
(#52466,#52467),(#52468,#52469),(#52470,#52471),(#52472,#52473),(#52474,
#52475),(#52476,#52477),(#52478,#52479),(#52480,#52481),(#52482,#52483),
(#52484,#52485),(#52486,#52487),(#52488,#52489),(#52490,#52491),(#52492,
#52493),(#52494,#52495),(#52496,#52497),(#52498,#52499)),.UNSPECIFIED.,
 .F.,.F.,.F.)
B_SPLINE_SURFACE_WITH_KNOTS((6,1,1,1,1,1,1,1,1,1,1,1,1,1,1,1,1,1,1,1,1,
1,1,1,1,1,1,1,1,1,1,1,1,1,1,1,1,1,1,1,1,1,1,1,1,1,1,1,1,1,1,1,1,1,1,1,1,
1,1,1,1,1,1,1,1,6),(2,2),(-1.,-0.984615384615383,-0.969230769230768,-0.953846153846152,
-0.938461538461537,-0.923076923076922,-0.907692307692306,-0.892307692307691,
-0.876923076923076,-0.86153846153846,-0.846153846153845,-0.83076923076923,
-0.815384615384614,-0.799999999999999,-0.784615384615384,-0.769230769230768,
-0.753846153846153,-0.738461538461538,-0.723076923076922,-0.707692307692307,
-0.692307692307692,-0.676923076923076,-0.661538461538461,-0.646153846153846,
-0.63076923076923,-0.615384615384615,-0.6,-0.584615384615384,-0.569230769230769,
-0.553846153846154,-0.538461538461538,-0.523076923076923,-0.507692307692308,
-0.492307692307692,-0.476923076923077,-0.461538461538462,-0.446153846153846,
-0.430769230769231,-0.415384615384615,-0.4,-0.384615384615385,-0.369230769230769,
-0.353846153846154,-0.338461538461538,-0.323076923076923,-0.307692307692308,
-0.292307692307692,-0.276923076923077,-0.261538461538462,-0.246153846153846,
-0.230769230769231,-0.215384615384615,-0.2,-0.184615384615385,-0.169230769230769,
-0.153846153846154,-0.138461538461538,-0.123076923076923,-0.107692307692308,
-0.0923076923076923,-0.0769230769230769,-0.0615384615384615,-0.0461538461538462,
-0.0307692307692308,-0.0153846153846154,0.),(-1.,1.),.UNSPECIFIED.)
GEOMETRIC_REPRESENTATION_ITEM()
RATIONAL_B_SPLINE_SURFACE(((1.,1.),(1.,1.),(1.,1.),(1.,1.),(1.,1.),(1.,
1.),(1.,1.),(1.,1.),(1.,1.),(1.,1.),(1.,1.),(1.,1.),(1.,1.),(1.,1.),(1.,
1.),(1.,1.),(1.,1.),(1.,1.),(1.,1.),(1.,1.),(1.,1.),(1.,1.),(1.,1.),(1.,
1.),(1.,1.),(1.,1.),(1.,1.),(1.,1.),(1.,1.),(1.,1.),(1.,1.),(1.,1.),(1.,
1.),(1.,1.),(1.,1.),(1.,1.),(1.,1.),(1.,1.),(1.,1.),(1.,1.),(1.,1.),(1.,
1.),(1.,1.),(1.,1.),(1.,1.),(1.,1.),(1.,1.),(1.,1.),(1.,1.),(1.,1.),(1.,
1.),(1.,1.),(1.,1.),(1.,1.),(1.,1.),(1.,1.),(1.,1.),(1.,1.),(1.,1.),(1.,
1.),(1.,1.),(1.,1.),(1.,1.),(1.,1.),(1.,1.),(1.,1.),(1.,1.),(1.,1.),(1.,
1.),(1.,1.)))
REPRESENTATION_ITEM('')
SURFACE()
);
#126=(
BOUNDED_SURFACE()
B_SPLINE_SURFACE(5,1,((#52572,#52573),(#52574,#52575),(#52576,#52577),(#52578,
#52579),(#52580,#52581),(#52582,#52583),(#52584,#52585),(#52586,#52587),
(#52588,#52589),(#52590,#52591),(#52592,#52593),(#52594,#52595),(#52596,
#52597),(#52598,#52599),(#52600,#52601),(#52602,#52603),(#52604,#52605),
(#52606,#52607),(#52608,#52609),(#52610,#52611),(#52612,#52613),(#52614,
#52615),(#52616,#52617),(#52618,#52619),(#52620,#52621),(#52622,#52623),
(#52624,#52625),(#52626,#52627),(#52628,#52629),(#52630,#52631),(#52632,
#52633),(#52634,#52635),(#52636,#52637),(#52638,#52639),(#52640,#52641),
(#52642,#52643),(#52644,#52645),(#52646,#52647),(#52648,#52649),(#52650,
#52651),(#52652,#52653),(#52654,#52655),(#52656,#52657),(#52658,#52659),
(#52660,#52661),(#52662,#52663),(#52664,#52665),(#52666,#52667),(#52668,
#52669),(#52670,#52671),(#52672,#52673),(#52674,#52675),(#52676,#52677),
(#52678,#52679),(#52680,#52681),(#52682,#52683),(#52684,#52685),(#52686,
#52687),(#52688,#52689),(#52690,#52691),(#52692,#52693),(#52694,#52695),
(#52696,#52697),(#52698,#52699),(#52700,#52701),(#52702,#52703),(#52704,
#52705),(#52706,#52707),(#52708,#52709),(#52710,#52711)),.UNSPECIFIED.,
 .F.,.F.,.F.)
B_SPLINE_SURFACE_WITH_KNOTS((6,1,1,1,1,1,1,1,1,1,1,1,1,1,1,1,1,1,1,1,1,
1,1,1,1,1,1,1,1,1,1,1,1,1,1,1,1,1,1,1,1,1,1,1,1,1,1,1,1,1,1,1,1,1,1,1,1,
1,1,1,1,1,1,1,1,6),(2,2),(-1.,-0.984615384615383,-0.969230769230768,-0.953846153846152,
-0.938461538461537,-0.923076923076922,-0.907692307692306,-0.892307692307691,
-0.876923076923076,-0.86153846153846,-0.846153846153845,-0.83076923076923,
-0.815384615384614,-0.799999999999999,-0.784615384615384,-0.769230769230768,
-0.753846153846153,-0.738461538461538,-0.723076923076922,-0.707692307692307,
-0.692307692307692,-0.676923076923076,-0.661538461538461,-0.646153846153846,
-0.63076923076923,-0.615384615384615,-0.6,-0.584615384615384,-0.569230769230769,
-0.553846153846154,-0.538461538461538,-0.523076923076923,-0.507692307692308,
-0.492307692307692,-0.476923076923077,-0.461538461538462,-0.446153846153846,
-0.430769230769231,-0.415384615384615,-0.4,-0.384615384615385,-0.369230769230769,
-0.353846153846154,-0.338461538461538,-0.323076923076923,-0.307692307692308,
-0.292307692307692,-0.276923076923077,-0.261538461538462,-0.246153846153846,
-0.230769230769231,-0.215384615384615,-0.2,-0.184615384615385,-0.169230769230769,
-0.153846153846154,-0.138461538461538,-0.123076923076923,-0.107692307692308,
-0.0923076923076923,-0.0769230769230769,-0.0615384615384615,-0.0461538461538462,
-0.0307692307692308,-0.0153846153846154,0.),(-1.,1.),.UNSPECIFIED.)
GEOMETRIC_REPRESENTATION_ITEM()
RATIONAL_B_SPLINE_SURFACE(((1.,1.),(1.,1.),(1.,1.),(1.,1.),(1.,1.),(1.,
1.),(1.,1.),(1.,1.),(1.,1.),(1.,1.),(1.,1.),(1.,1.),(1.,1.),(1.,1.),(1.,
1.),(1.,1.),(1.,1.),(1.,1.),(1.,1.),(1.,1.),(1.,1.),(1.,1.),(1.,1.),(1.,
1.),(1.,1.),(1.,1.),(1.,1.),(1.,1.),(1.,1.),(1.,1.),(1.,1.),(1.,1.),(1.,
1.),(1.,1.),(1.,1.),(1.,1.),(1.,1.),(1.,1.),(1.,1.),(1.,1.),(1.,1.),(1.,
1.),(1.,1.),(1.,1.),(1.,1.),(1.,1.),(1.,1.),(1.,1.),(1.,1.),(1.,1.),(1.,
1.),(1.,1.),(1.,1.),(1.,1.),(1.,1.),(1.,1.),(1.,1.),(1.,1.),(1.,1.),(1.,
1.),(1.,1.),(1.,1.),(1.,1.),(1.,1.),(1.,1.),(1.,1.),(1.,1.),(1.,1.),(1.,
1.),(1.,1.)))
REPRESENTATION_ITEM('')
SURFACE()
);
#127=(
BOUNDED_SURFACE()
B_SPLINE_SURFACE(5,1,((#52802,#52803),(#52804,#52805),(#52806,#52807),(#52808,
#52809),(#52810,#52811),(#52812,#52813),(#52814,#52815),(#52816,#52817),
(#52818,#52819),(#52820,#52821),(#52822,#52823),(#52824,#52825),(#52826,
#52827),(#52828,#52829),(#52830,#52831),(#52832,#52833),(#52834,#52835),
(#52836,#52837),(#52838,#52839),(#52840,#52841),(#52842,#52843),(#52844,
#52845),(#52846,#52847),(#52848,#52849),(#52850,#52851),(#52852,#52853),
(#52854,#52855),(#52856,#52857),(#52858,#52859),(#52860,#52861),(#52862,
#52863),(#52864,#52865),(#52866,#52867),(#52868,#52869),(#52870,#52871),
(#52872,#52873),(#52874,#52875),(#52876,#52877),(#52878,#52879),(#52880,
#52881),(#52882,#52883),(#52884,#52885),(#52886,#52887),(#52888,#52889),
(#52890,#52891),(#52892,#52893),(#52894,#52895),(#52896,#52897),(#52898,
#52899),(#52900,#52901),(#52902,#52903),(#52904,#52905),(#52906,#52907),
(#52908,#52909),(#52910,#52911),(#52912,#52913),(#52914,#52915),(#52916,
#52917),(#52918,#52919),(#52920,#52921),(#52922,#52923),(#52924,#52925),
(#52926,#52927),(#52928,#52929),(#52930,#52931),(#52932,#52933),(#52934,
#52935),(#52936,#52937),(#52938,#52939),(#52940,#52941)),.UNSPECIFIED.,
 .F.,.F.,.F.)
B_SPLINE_SURFACE_WITH_KNOTS((6,1,1,1,1,1,1,1,1,1,1,1,1,1,1,1,1,1,1,1,1,
1,1,1,1,1,1,1,1,1,1,1,1,1,1,1,1,1,1,1,1,1,1,1,1,1,1,1,1,1,1,1,1,1,1,1,1,
1,1,1,1,1,1,1,1,6),(2,2),(-1.,-0.984615384615383,-0.969230769230768,-0.953846153846152,
-0.938461538461537,-0.923076923076922,-0.907692307692306,-0.892307692307691,
-0.876923076923076,-0.86153846153846,-0.846153846153845,-0.83076923076923,
-0.815384615384614,-0.799999999999999,-0.784615384615384,-0.769230769230768,
-0.753846153846153,-0.738461538461538,-0.723076923076922,-0.707692307692307,
-0.692307692307692,-0.676923076923076,-0.661538461538461,-0.646153846153846,
-0.63076923076923,-0.615384615384615,-0.6,-0.584615384615384,-0.569230769230769,
-0.553846153846154,-0.538461538461538,-0.523076923076923,-0.507692307692308,
-0.492307692307692,-0.476923076923077,-0.461538461538462,-0.446153846153846,
-0.430769230769231,-0.415384615384615,-0.4,-0.384615384615385,-0.369230769230769,
-0.353846153846154,-0.338461538461538,-0.323076923076923,-0.307692307692308,
-0.292307692307692,-0.276923076923077,-0.261538461538462,-0.246153846153846,
-0.230769230769231,-0.215384615384615,-0.2,-0.184615384615385,-0.169230769230769,
-0.153846153846154,-0.138461538461538,-0.123076923076923,-0.107692307692308,
-0.0923076923076923,-0.0769230769230769,-0.0615384615384615,-0.0461538461538462,
-0.0307692307692308,-0.0153846153846154,0.),(-1.,1.),.UNSPECIFIED.)
GEOMETRIC_REPRESENTATION_ITEM()
RATIONAL_B_SPLINE_SURFACE(((1.,1.),(1.,1.),(1.,1.),(1.,1.),(1.,1.),(1.,
1.),(1.,1.),(1.,1.),(1.,1.),(1.,1.),(1.,1.),(1.,1.),(1.,1.),(1.,1.),(1.,
1.),(1.,1.),(1.,1.),(1.,1.),(1.,1.),(1.,1.),(1.,1.),(1.,1.),(1.,1.),(1.,
1.),(1.,1.),(1.,1.),(1.,1.),(1.,1.),(1.,1.),(1.,1.),(1.,1.),(1.,1.),(1.,
1.),(1.,1.),(1.,1.),(1.,1.),(1.,1.),(1.,1.),(1.,1.),(1.,1.),(1.,1.),(1.,
1.),(1.,1.),(1.,1.),(1.,1.),(1.,1.),(1.,1.),(1.,1.),(1.,1.),(1.,1.),(1.,
1.),(1.,1.),(1.,1.),(1.,1.),(1.,1.),(1.,1.),(1.,1.),(1.,1.),(1.,1.),(1.,
1.),(1.,1.),(1.,1.),(1.,1.),(1.,1.),(1.,1.),(1.,1.),(1.,1.),(1.,1.),(1.,
1.),(1.,1.)))
REPRESENTATION_ITEM('')
SURFACE()
);
#128=(
BOUNDED_SURFACE()
B_SPLINE_SURFACE(5,1,((#53018,#53019),(#53020,#53021),(#53022,#53023),(#53024,
#53025),(#53026,#53027),(#53028,#53029),(#53030,#53031),(#53032,#53033),
(#53034,#53035),(#53036,#53037),(#53038,#53039),(#53040,#53041),(#53042,
#53043),(#53044,#53045),(#53046,#53047),(#53048,#53049),(#53050,#53051),
(#53052,#53053),(#53054,#53055),(#53056,#53057),(#53058,#53059),(#53060,
#53061),(#53062,#53063),(#53064,#53065),(#53066,#53067),(#53068,#53069),
(#53070,#53071),(#53072,#53073),(#53074,#53075),(#53076,#53077),(#53078,
#53079),(#53080,#53081),(#53082,#53083),(#53084,#53085),(#53086,#53087),
(#53088,#53089),(#53090,#53091),(#53092,#53093),(#53094,#53095),(#53096,
#53097),(#53098,#53099),(#53100,#53101),(#53102,#53103),(#53104,#53105),
(#53106,#53107),(#53108,#53109),(#53110,#53111),(#53112,#53113),(#53114,
#53115),(#53116,#53117),(#53118,#53119),(#53120,#53121),(#53122,#53123),
(#53124,#53125),(#53126,#53127),(#53128,#53129),(#53130,#53131),(#53132,
#53133),(#53134,#53135),(#53136,#53137),(#53138,#53139),(#53140,#53141),
(#53142,#53143),(#53144,#53145),(#53146,#53147),(#53148,#53149),(#53150,
#53151),(#53152,#53153),(#53154,#53155),(#53156,#53157)),.UNSPECIFIED.,
 .F.,.F.,.F.)
B_SPLINE_SURFACE_WITH_KNOTS((6,1,1,1,1,1,1,1,1,1,1,1,1,1,1,1,1,1,1,1,1,
1,1,1,1,1,1,1,1,1,1,1,1,1,1,1,1,1,1,1,1,1,1,1,1,1,1,1,1,1,1,1,1,1,1,1,1,
1,1,1,1,1,1,1,1,6),(2,2),(-1.,-0.984615384615383,-0.969230769230768,-0.953846153846152,
-0.938461538461537,-0.923076923076922,-0.907692307692306,-0.892307692307691,
-0.876923076923076,-0.86153846153846,-0.846153846153845,-0.83076923076923,
-0.815384615384614,-0.799999999999999,-0.784615384615384,-0.769230769230768,
-0.753846153846153,-0.738461538461538,-0.723076923076922,-0.707692307692307,
-0.692307692307692,-0.676923076923076,-0.661538461538461,-0.646153846153846,
-0.63076923076923,-0.615384615384615,-0.6,-0.584615384615384,-0.569230769230769,
-0.553846153846154,-0.538461538461538,-0.523076923076923,-0.507692307692308,
-0.492307692307692,-0.476923076923077,-0.461538461538462,-0.446153846153846,
-0.430769230769231,-0.415384615384615,-0.4,-0.384615384615385,-0.369230769230769,
-0.353846153846154,-0.338461538461538,-0.323076923076923,-0.307692307692308,
-0.292307692307692,-0.276923076923077,-0.261538461538462,-0.246153846153846,
-0.230769230769231,-0.215384615384615,-0.2,-0.184615384615385,-0.169230769230769,
-0.153846153846154,-0.138461538461538,-0.123076923076923,-0.107692307692308,
-0.0923076923076923,-0.0769230769230769,-0.0615384615384615,-0.0461538461538462,
-0.0307692307692308,-0.0153846153846154,0.),(-1.,1.),.UNSPECIFIED.)
GEOMETRIC_REPRESENTATION_ITEM()
RATIONAL_B_SPLINE_SURFACE(((1.,1.),(1.,1.),(1.,1.),(1.,1.),(1.,1.),(1.,
1.),(1.,1.),(1.,1.),(1.,1.),(1.,1.),(1.,1.),(1.,1.),(1.,1.),(1.,1.),(1.,
1.),(1.,1.),(1.,1.),(1.,1.),(1.,1.),(1.,1.),(1.,1.),(1.,1.),(1.,1.),(1.,
1.),(1.,1.),(1.,1.),(1.,1.),(1.,1.),(1.,1.),(1.,1.),(1.,1.),(1.,1.),(1.,
1.),(1.,1.),(1.,1.),(1.,1.),(1.,1.),(1.,1.),(1.,1.),(1.,1.),(1.,1.),(1.,
1.),(1.,1.),(1.,1.),(1.,1.),(1.,1.),(1.,1.),(1.,1.),(1.,1.),(1.,1.),(1.,
1.),(1.,1.),(1.,1.),(1.,1.),(1.,1.),(1.,1.),(1.,1.),(1.,1.),(1.,1.),(1.,
1.),(1.,1.),(1.,1.),(1.,1.),(1.,1.),(1.,1.),(1.,1.),(1.,1.),(1.,1.),(1.,
1.),(1.,1.)))
REPRESENTATION_ITEM('')
SURFACE()
);
#129=(
BOUNDED_SURFACE()
B_SPLINE_SURFACE(5,1,((#53244,#53245),(#53246,#53247),(#53248,#53249),(#53250,
#53251),(#53252,#53253),(#53254,#53255),(#53256,#53257),(#53258,#53259),
(#53260,#53261),(#53262,#53263),(#53264,#53265),(#53266,#53267),(#53268,
#53269),(#53270,#53271),(#53272,#53273),(#53274,#53275),(#53276,#53277),
(#53278,#53279),(#53280,#53281),(#53282,#53283),(#53284,#53285),(#53286,
#53287),(#53288,#53289),(#53290,#53291),(#53292,#53293),(#53294,#53295),
(#53296,#53297),(#53298,#53299),(#53300,#53301),(#53302,#53303),(#53304,
#53305),(#53306,#53307),(#53308,#53309),(#53310,#53311),(#53312,#53313),
(#53314,#53315),(#53316,#53317),(#53318,#53319),(#53320,#53321),(#53322,
#53323),(#53324,#53325),(#53326,#53327),(#53328,#53329),(#53330,#53331),
(#53332,#53333),(#53334,#53335),(#53336,#53337),(#53338,#53339),(#53340,
#53341),(#53342,#53343),(#53344,#53345),(#53346,#53347),(#53348,#53349),
(#53350,#53351),(#53352,#53353),(#53354,#53355),(#53356,#53357),(#53358,
#53359),(#53360,#53361),(#53362,#53363),(#53364,#53365),(#53366,#53367),
(#53368,#53369),(#53370,#53371),(#53372,#53373),(#53374,#53375),(#53376,
#53377),(#53378,#53379),(#53380,#53381),(#53382,#53383)),.UNSPECIFIED.,
 .F.,.F.,.F.)
B_SPLINE_SURFACE_WITH_KNOTS((6,1,1,1,1,1,1,1,1,1,1,1,1,1,1,1,1,1,1,1,1,
1,1,1,1,1,1,1,1,1,1,1,1,1,1,1,1,1,1,1,1,1,1,1,1,1,1,1,1,1,1,1,1,1,1,1,1,
1,1,1,1,1,1,1,1,6),(2,2),(-1.,-0.984615384615383,-0.969230769230768,-0.953846153846152,
-0.938461538461537,-0.923076923076922,-0.907692307692306,-0.892307692307691,
-0.876923076923076,-0.86153846153846,-0.846153846153845,-0.83076923076923,
-0.815384615384614,-0.799999999999999,-0.784615384615384,-0.769230769230768,
-0.753846153846153,-0.738461538461538,-0.723076923076922,-0.707692307692307,
-0.692307692307692,-0.676923076923076,-0.661538461538461,-0.646153846153846,
-0.63076923076923,-0.615384615384615,-0.6,-0.584615384615384,-0.569230769230769,
-0.553846153846154,-0.538461538461538,-0.523076923076923,-0.507692307692308,
-0.492307692307692,-0.476923076923077,-0.461538461538462,-0.446153846153846,
-0.430769230769231,-0.415384615384615,-0.4,-0.384615384615385,-0.369230769230769,
-0.353846153846154,-0.338461538461538,-0.323076923076923,-0.307692307692308,
-0.292307692307692,-0.276923076923077,-0.261538461538462,-0.246153846153846,
-0.230769230769231,-0.215384615384615,-0.2,-0.184615384615385,-0.169230769230769,
-0.153846153846154,-0.138461538461538,-0.123076923076923,-0.107692307692308,
-0.0923076923076923,-0.0769230769230769,-0.0615384615384615,-0.0461538461538462,
-0.0307692307692308,-0.0153846153846154,0.),(-1.,1.),.UNSPECIFIED.)
GEOMETRIC_REPRESENTATION_ITEM()
RATIONAL_B_SPLINE_SURFACE(((1.,1.),(1.,1.),(1.,1.),(1.,1.),(1.,1.),(1.,
1.),(1.,1.),(1.,1.),(1.,1.),(1.,1.),(1.,1.),(1.,1.),(1.,1.),(1.,1.),(1.,
1.),(1.,1.),(1.,1.),(1.,1.),(1.,1.),(1.,1.),(1.,1.),(1.,1.),(1.,1.),(1.,
1.),(1.,1.),(1.,1.),(1.,1.),(1.,1.),(1.,1.),(1.,1.),(1.,1.),(1.,1.),(1.,
1.),(1.,1.),(1.,1.),(1.,1.),(1.,1.),(1.,1.),(1.,1.),(1.,1.),(1.,1.),(1.,
1.),(1.,1.),(1.,1.),(1.,1.),(1.,1.),(1.,1.),(1.,1.),(1.,1.),(1.,1.),(1.,
1.),(1.,1.),(1.,1.),(1.,1.),(1.,1.),(1.,1.),(1.,1.),(1.,1.),(1.,1.),(1.,
1.),(1.,1.),(1.,1.),(1.,1.),(1.,1.),(1.,1.),(1.,1.),(1.,1.),(1.,1.),(1.,
1.),(1.,1.)))
REPRESENTATION_ITEM('')
SURFACE()
);
#130=(
BOUNDED_SURFACE()
B_SPLINE_SURFACE(5,1,((#53463,#53464),(#53465,#53466),(#53467,#53468),(#53469,
#53470),(#53471,#53472),(#53473,#53474),(#53475,#53476),(#53477,#53478),
(#53479,#53480),(#53481,#53482),(#53483,#53484),(#53485,#53486),(#53487,
#53488),(#53489,#53490),(#53491,#53492),(#53493,#53494),(#53495,#53496),
(#53497,#53498),(#53499,#53500),(#53501,#53502),(#53503,#53504),(#53505,
#53506),(#53507,#53508),(#53509,#53510),(#53511,#53512),(#53513,#53514),
(#53515,#53516),(#53517,#53518),(#53519,#53520),(#53521,#53522),(#53523,
#53524),(#53525,#53526),(#53527,#53528),(#53529,#53530),(#53531,#53532),
(#53533,#53534),(#53535,#53536),(#53537,#53538),(#53539,#53540),(#53541,
#53542),(#53543,#53544),(#53545,#53546),(#53547,#53548),(#53549,#53550),
(#53551,#53552),(#53553,#53554),(#53555,#53556),(#53557,#53558),(#53559,
#53560),(#53561,#53562),(#53563,#53564),(#53565,#53566),(#53567,#53568),
(#53569,#53570),(#53571,#53572),(#53573,#53574),(#53575,#53576),(#53577,
#53578),(#53579,#53580),(#53581,#53582),(#53583,#53584),(#53585,#53586),
(#53587,#53588),(#53589,#53590),(#53591,#53592),(#53593,#53594),(#53595,
#53596),(#53597,#53598),(#53599,#53600),(#53601,#53602)),.UNSPECIFIED.,
 .F.,.F.,.F.)
B_SPLINE_SURFACE_WITH_KNOTS((6,1,1,1,1,1,1,1,1,1,1,1,1,1,1,1,1,1,1,1,1,
1,1,1,1,1,1,1,1,1,1,1,1,1,1,1,1,1,1,1,1,1,1,1,1,1,1,1,1,1,1,1,1,1,1,1,1,
1,1,1,1,1,1,1,1,6),(2,2),(-1.,-0.984615384615383,-0.969230769230768,-0.953846153846152,
-0.938461538461537,-0.923076923076922,-0.907692307692306,-0.892307692307691,
-0.876923076923076,-0.86153846153846,-0.846153846153845,-0.83076923076923,
-0.815384615384614,-0.799999999999999,-0.784615384615384,-0.769230769230768,
-0.753846153846153,-0.738461538461538,-0.723076923076922,-0.707692307692307,
-0.692307692307692,-0.676923076923076,-0.661538461538461,-0.646153846153846,
-0.63076923076923,-0.615384615384615,-0.6,-0.584615384615384,-0.569230769230769,
-0.553846153846154,-0.538461538461538,-0.523076923076923,-0.507692307692308,
-0.492307692307692,-0.476923076923077,-0.461538461538462,-0.446153846153846,
-0.430769230769231,-0.415384615384615,-0.4,-0.384615384615385,-0.369230769230769,
-0.353846153846154,-0.338461538461538,-0.323076923076923,-0.307692307692308,
-0.292307692307692,-0.276923076923077,-0.261538461538462,-0.246153846153846,
-0.230769230769231,-0.215384615384615,-0.2,-0.184615384615385,-0.169230769230769,
-0.153846153846154,-0.138461538461538,-0.123076923076923,-0.107692307692308,
-0.0923076923076923,-0.0769230769230769,-0.0615384615384615,-0.0461538461538462,
-0.0307692307692308,-0.0153846153846154,0.),(-1.,1.),.UNSPECIFIED.)
GEOMETRIC_REPRESENTATION_ITEM()
RATIONAL_B_SPLINE_SURFACE(((1.,1.),(1.,1.),(1.,1.),(1.,1.),(1.,1.),(1.,
1.),(1.,1.),(1.,1.),(1.,1.),(1.,1.),(1.,1.),(1.,1.),(1.,1.),(1.,1.),(1.,
1.),(1.,1.),(1.,1.),(1.,1.),(1.,1.),(1.,1.),(1.,1.),(1.,1.),(1.,1.),(1.,
1.),(1.,1.),(1.,1.),(1.,1.),(1.,1.),(1.,1.),(1.,1.),(1.,1.),(1.,1.),(1.,
1.),(1.,1.),(1.,1.),(1.,1.),(1.,1.),(1.,1.),(1.,1.),(1.,1.),(1.,1.),(1.,
1.),(1.,1.),(1.,1.),(1.,1.),(1.,1.),(1.,1.),(1.,1.),(1.,1.),(1.,1.),(1.,
1.),(1.,1.),(1.,1.),(1.,1.),(1.,1.),(1.,1.),(1.,1.),(1.,1.),(1.,1.),(1.,
1.),(1.,1.),(1.,1.),(1.,1.),(1.,1.),(1.,1.),(1.,1.),(1.,1.),(1.,1.),(1.,
1.),(1.,1.)))
REPRESENTATION_ITEM('')
SURFACE()
);
#131=(
BOUNDED_CURVE()
B_SPLINE_CURVE(5,(#18215,#18216,#18217,#18218,#18219,#18220,#18221,#18222,
#18223,#18224,#18225,#18226,#18227,#18228,#18229,#18230,#18231,#18232,#18233,
#18234,#18235,#18236,#18237,#18238,#18239,#18240,#18241,#18242,#18243,#18244,
#18245,#18246,#18247,#18248,#18249,#18250,#18251,#18252,#18253,#18254,#18255,
#18256,#18257,#18258,#18259,#18260,#18261,#18262,#18263,#18264,#18265,#18266,
#18267,#18268,#18269,#18270,#18271,#18272,#18273,#18274,#18275,#18276,#18277,
#18278,#18279,#18280,#18281,#18282,#18283,#18284),.UNSPECIFIED.,.F.,.F.)
B_SPLINE_CURVE_WITH_KNOTS((6,1,1,1,1,1,1,1,1,1,1,1,1,1,1,1,1,1,1,1,1,1,
1,1,1,1,1,1,1,1,1,1,1,1,1,1,1,1,1,1,1,1,1,1,1,1,1,1,1,1,1,1,1,1,1,1,1,1,
1,1,1,1,1,1,1,6),(0.,0.0153846153846154,0.0307692307692308,0.0461538461538462,
0.0615384615384615,0.0769230769230769,0.0923076923076923,0.107692307692308,
0.123076923076923,0.138461538461538,0.153846153846154,0.169230769230769,
0.184615384615385,0.2,0.215384615384615,0.230769230769231,0.246153846153846,
0.261538461538462,0.276923076923077,0.292307692307692,0.307692307692308,
0.323076923076923,0.338461538461538,0.353846153846154,0.369230769230769,
0.384615384615385,0.4,0.415384615384615,0.430769230769231,0.446153846153846,
0.461538461538462,0.476923076923077,0.492307692307692,0.507692307692308,
0.523076923076923,0.538461538461538,0.553846153846154,0.569230769230769,
0.584615384615384,0.6,0.615384615384615,0.63076923076923,0.646153846153846,
0.661538461538461,0.676923076923076,0.692307692307692,0.707692307692307,
0.723076923076922,0.738461538461538,0.753846153846153,0.769230769230768,
0.784615384615384,0.799999999999999,0.815384615384614,0.83076923076923,
0.846153846153845,0.86153846153846,0.876923076923076,0.892307692307691,
0.907692307692306,0.923076923076922,0.938461538461537,0.953846153846152,
0.969230769230768,0.984615384615383,1.),.UNSPECIFIED.)
CURVE()
GEOMETRIC_REPRESENTATION_ITEM()
RATIONAL_B_SPLINE_CURVE((1.,1.,1.,1.,1.,1.,1.,1.,1.,1.,1.,1.,1.,1.,1.,1.,
1.,1.,1.,1.,1.,1.,1.,1.,1.,1.,1.,1.,1.,1.,1.,1.,1.,1.,1.,1.,1.,1.,1.,1.,
1.,1.,1.,1.,1.,1.,1.,1.,1.,1.,1.,1.,1.,1.,1.,1.,1.,1.,1.,1.,1.,1.,1.,1.,
1.,1.,1.,1.,1.,1.))
REPRESENTATION_ITEM('')
);
#132=(
BOUNDED_CURVE()
B_SPLINE_CURVE(5,(#18288,#18289,#18290,#18291,#18292,#18293,#18294,#18295,
#18296,#18297,#18298,#18299,#18300,#18301,#18302,#18303,#18304,#18305,#18306,
#18307,#18308,#18309,#18310,#18311,#18312,#18313,#18314,#18315,#18316,#18317,
#18318,#18319,#18320,#18321,#18322,#18323,#18324,#18325,#18326,#18327,#18328,
#18329,#18330,#18331,#18332,#18333,#18334,#18335,#18336,#18337,#18338,#18339,
#18340,#18341,#18342,#18343,#18344,#18345,#18346,#18347,#18348,#18349,#18350,
#18351,#18352,#18353,#18354,#18355,#18356,#18357),.UNSPECIFIED.,.F.,.F.)
B_SPLINE_CURVE_WITH_KNOTS((6,1,1,1,1,1,1,1,1,1,1,1,1,1,1,1,1,1,1,1,1,1,
1,1,1,1,1,1,1,1,1,1,1,1,1,1,1,1,1,1,1,1,1,1,1,1,1,1,1,1,1,1,1,1,1,1,1,1,
1,1,1,1,1,1,1,6),(0.,0.0153846153846154,0.0307692307692308,0.0461538461538462,
0.0615384615384615,0.0769230769230769,0.0923076923076923,0.107692307692308,
0.123076923076923,0.138461538461538,0.153846153846154,0.169230769230769,
0.184615384615385,0.2,0.215384615384615,0.230769230769231,0.246153846153846,
0.261538461538462,0.276923076923077,0.292307692307692,0.307692307692308,
0.323076923076923,0.338461538461538,0.353846153846154,0.369230769230769,
0.384615384615385,0.4,0.415384615384615,0.430769230769231,0.446153846153846,
0.461538461538462,0.476923076923077,0.492307692307692,0.507692307692308,
0.523076923076923,0.538461538461538,0.553846153846154,0.569230769230769,
0.584615384615384,0.6,0.615384615384615,0.63076923076923,0.646153846153846,
0.661538461538461,0.676923076923076,0.692307692307692,0.707692307692307,
0.723076923076922,0.738461538461538,0.753846153846153,0.769230769230768,
0.784615384615384,0.799999999999999,0.815384615384614,0.83076923076923,
0.846153846153845,0.86153846153846,0.876923076923076,0.892307692307691,
0.907692307692306,0.923076923076922,0.938461538461537,0.953846153846152,
0.969230769230768,0.984615384615383,1.),.UNSPECIFIED.)
CURVE()
GEOMETRIC_REPRESENTATION_ITEM()
RATIONAL_B_SPLINE_CURVE((1.,1.,1.,1.,1.,1.,1.,1.,1.,1.,1.,1.,1.,1.,1.,1.,
1.,1.,1.,1.,1.,1.,1.,1.,1.,1.,1.,1.,1.,1.,1.,1.,1.,1.,1.,1.,1.,1.,1.,1.,
1.,1.,1.,1.,1.,1.,1.,1.,1.,1.,1.,1.,1.,1.,1.,1.,1.,1.,1.,1.,1.,1.,1.,1.,
1.,1.,1.,1.,1.,1.))
REPRESENTATION_ITEM('')
);
#133=(
BOUNDED_CURVE()
B_SPLINE_CURVE(5,(#18361,#18362,#18363,#18364,#18365,#18366,#18367,#18368,
#18369,#18370,#18371,#18372,#18373,#18374,#18375,#18376,#18377,#18378,#18379,
#18380,#18381,#18382,#18383,#18384,#18385,#18386,#18387,#18388,#18389,#18390,
#18391,#18392,#18393,#18394,#18395,#18396,#18397,#18398,#18399,#18400,#18401,
#18402,#18403,#18404,#18405,#18406,#18407,#18408,#18409,#18410,#18411,#18412,
#18413,#18414,#18415,#18416,#18417,#18418,#18419,#18420,#18421,#18422,#18423,
#18424,#18425,#18426,#18427,#18428,#18429,#18430),.UNSPECIFIED.,.F.,.F.)
B_SPLINE_CURVE_WITH_KNOTS((6,1,1,1,1,1,1,1,1,1,1,1,1,1,1,1,1,1,1,1,1,1,
1,1,1,1,1,1,1,1,1,1,1,1,1,1,1,1,1,1,1,1,1,1,1,1,1,1,1,1,1,1,1,1,1,1,1,1,
1,1,1,1,1,1,1,6),(0.,0.0153846153846154,0.0307692307692308,0.0461538461538462,
0.0615384615384615,0.0769230769230769,0.0923076923076923,0.107692307692308,
0.123076923076923,0.138461538461538,0.153846153846154,0.169230769230769,
0.184615384615385,0.2,0.215384615384615,0.230769230769231,0.246153846153846,
0.261538461538462,0.276923076923077,0.292307692307692,0.307692307692308,
0.323076923076923,0.338461538461538,0.353846153846154,0.369230769230769,
0.384615384615385,0.4,0.415384615384615,0.430769230769231,0.446153846153846,
0.461538461538462,0.476923076923077,0.492307692307692,0.507692307692308,
0.523076923076923,0.538461538461538,0.553846153846154,0.569230769230769,
0.584615384615384,0.6,0.615384615384615,0.63076923076923,0.646153846153846,
0.661538461538461,0.676923076923076,0.692307692307692,0.707692307692307,
0.723076923076922,0.738461538461538,0.753846153846153,0.769230769230768,
0.784615384615384,0.799999999999999,0.815384615384614,0.83076923076923,
0.846153846153845,0.86153846153846,0.876923076923076,0.892307692307691,
0.907692307692306,0.923076923076922,0.938461538461537,0.953846153846152,
0.969230769230768,0.984615384615383,1.),.UNSPECIFIED.)
CURVE()
GEOMETRIC_REPRESENTATION_ITEM()
RATIONAL_B_SPLINE_CURVE((1.,1.,1.,1.,1.,1.,1.,1.,1.,1.,1.,1.,1.,1.,1.,1.,
1.,1.,1.,1.,1.,1.,1.,1.,1.,1.,1.,1.,1.,1.,1.,1.,1.,1.,1.,1.,1.,1.,1.,1.,
1.,1.,1.,1.,1.,1.,1.,1.,1.,1.,1.,1.,1.,1.,1.,1.,1.,1.,1.,1.,1.,1.,1.,1.,
1.,1.,1.,1.,1.,1.))
REPRESENTATION_ITEM('')
);
#134=(
BOUNDED_CURVE()
B_SPLINE_CURVE(5,(#18434,#18435,#18436,#18437,#18438,#18439,#18440,#18441,
#18442,#18443,#18444,#18445,#18446,#18447,#18448,#18449,#18450,#18451,#18452,
#18453,#18454,#18455,#18456,#18457,#18458,#18459,#18460,#18461,#18462,#18463,
#18464,#18465,#18466,#18467,#18468,#18469,#18470,#18471,#18472,#18473,#18474,
#18475,#18476,#18477,#18478,#18479,#18480,#18481,#18482,#18483,#18484,#18485,
#18486,#18487,#18488,#18489,#18490,#18491,#18492,#18493,#18494,#18495,#18496,
#18497,#18498,#18499,#18500,#18501,#18502,#18503),.UNSPECIFIED.,.F.,.F.)
B_SPLINE_CURVE_WITH_KNOTS((6,1,1,1,1,1,1,1,1,1,1,1,1,1,1,1,1,1,1,1,1,1,
1,1,1,1,1,1,1,1,1,1,1,1,1,1,1,1,1,1,1,1,1,1,1,1,1,1,1,1,1,1,1,1,1,1,1,1,
1,1,1,1,1,1,1,6),(0.,0.0153846153846154,0.0307692307692308,0.0461538461538462,
0.0615384615384615,0.0769230769230769,0.0923076923076923,0.107692307692308,
0.123076923076923,0.138461538461538,0.153846153846154,0.169230769230769,
0.184615384615385,0.2,0.215384615384615,0.230769230769231,0.246153846153846,
0.261538461538462,0.276923076923077,0.292307692307692,0.307692307692308,
0.323076923076923,0.338461538461538,0.353846153846154,0.369230769230769,
0.384615384615385,0.4,0.415384615384615,0.430769230769231,0.446153846153846,
0.461538461538462,0.476923076923077,0.492307692307692,0.507692307692308,
0.523076923076923,0.538461538461538,0.553846153846154,0.569230769230769,
0.584615384615384,0.6,0.615384615384615,0.63076923076923,0.646153846153846,
0.661538461538461,0.676923076923076,0.692307692307692,0.707692307692307,
0.723076923076922,0.738461538461538,0.753846153846153,0.769230769230768,
0.784615384615384,0.799999999999999,0.815384615384614,0.83076923076923,
0.846153846153845,0.86153846153846,0.876923076923076,0.892307692307691,
0.907692307692306,0.923076923076922,0.938461538461537,0.953846153846152,
0.969230769230768,0.984615384615383,1.),.UNSPECIFIED.)
CURVE()
GEOMETRIC_REPRESENTATION_ITEM()
RATIONAL_B_SPLINE_CURVE((1.,1.,1.,1.,1.,1.,1.,1.,1.,1.,1.,1.,1.,1.,1.,1.,
1.,1.,1.,1.,1.,1.,1.,1.,1.,1.,1.,1.,1.,1.,1.,1.,1.,1.,1.,1.,1.,1.,1.,1.,
1.,1.,1.,1.,1.,1.,1.,1.,1.,1.,1.,1.,1.,1.,1.,1.,1.,1.,1.,1.,1.,1.,1.,1.,
1.,1.,1.,1.,1.,1.))
REPRESENTATION_ITEM('')
);
#135=(
BOUNDED_CURVE()
B_SPLINE_CURVE(5,(#18507,#18508,#18509,#18510,#18511,#18512,#18513,#18514,
#18515,#18516,#18517,#18518,#18519,#18520,#18521,#18522,#18523,#18524,#18525,
#18526,#18527,#18528,#18529,#18530,#18531,#18532,#18533,#18534,#18535,#18536,
#18537,#18538,#18539,#18540,#18541,#18542,#18543,#18544,#18545,#18546,#18547,
#18548,#18549,#18550,#18551,#18552,#18553,#18554,#18555,#18556,#18557,#18558,
#18559,#18560,#18561,#18562,#18563,#18564,#18565,#18566,#18567,#18568,#18569,
#18570,#18571,#18572,#18573,#18574,#18575,#18576),.UNSPECIFIED.,.F.,.F.)
B_SPLINE_CURVE_WITH_KNOTS((6,1,1,1,1,1,1,1,1,1,1,1,1,1,1,1,1,1,1,1,1,1,
1,1,1,1,1,1,1,1,1,1,1,1,1,1,1,1,1,1,1,1,1,1,1,1,1,1,1,1,1,1,1,1,1,1,1,1,
1,1,1,1,1,1,1,6),(0.,0.0153846153846154,0.0307692307692308,0.0461538461538462,
0.0615384615384615,0.0769230769230769,0.0923076923076923,0.107692307692308,
0.123076923076923,0.138461538461538,0.153846153846154,0.169230769230769,
0.184615384615385,0.2,0.215384615384615,0.230769230769231,0.246153846153846,
0.261538461538462,0.276923076923077,0.292307692307692,0.307692307692308,
0.323076923076923,0.338461538461538,0.353846153846154,0.369230769230769,
0.384615384615385,0.4,0.415384615384615,0.430769230769231,0.446153846153846,
0.461538461538462,0.476923076923077,0.492307692307692,0.507692307692308,
0.523076923076923,0.538461538461538,0.553846153846154,0.569230769230769,
0.584615384615384,0.6,0.615384615384615,0.63076923076923,0.646153846153846,
0.661538461538461,0.676923076923076,0.692307692307692,0.707692307692307,
0.723076923076922,0.738461538461538,0.753846153846153,0.769230769230768,
0.784615384615384,0.799999999999999,0.815384615384614,0.83076923076923,
0.846153846153845,0.86153846153846,0.876923076923076,0.892307692307691,
0.907692307692306,0.923076923076922,0.938461538461537,0.953846153846152,
0.969230769230768,0.984615384615383,1.),.UNSPECIFIED.)
CURVE()
GEOMETRIC_REPRESENTATION_ITEM()
RATIONAL_B_SPLINE_CURVE((1.,1.,1.,1.,1.,1.,1.,1.,1.,1.,1.,1.,1.,1.,1.,1.,
1.,1.,1.,1.,1.,1.,1.,1.,1.,1.,1.,1.,1.,1.,1.,1.,1.,1.,1.,1.,1.,1.,1.,1.,
1.,1.,1.,1.,1.,1.,1.,1.,1.,1.,1.,1.,1.,1.,1.,1.,1.,1.,1.,1.,1.,1.,1.,1.,
1.,1.,1.,1.,1.,1.))
REPRESENTATION_ITEM('')
);
#136=(
BOUNDED_CURVE()
B_SPLINE_CURVE(5,(#18580,#18581,#18582,#18583,#18584,#18585,#18586,#18587,
#18588,#18589,#18590,#18591,#18592,#18593,#18594,#18595,#18596,#18597,#18598,
#18599,#18600,#18601,#18602,#18603,#18604,#18605,#18606,#18607,#18608,#18609,
#18610,#18611,#18612,#18613,#18614,#18615,#18616,#18617,#18618,#18619,#18620,
#18621,#18622,#18623,#18624,#18625,#18626,#18627,#18628,#18629,#18630,#18631,
#18632,#18633,#18634,#18635,#18636,#18637,#18638,#18639,#18640,#18641,#18642,
#18643,#18644,#18645,#18646,#18647,#18648,#18649),.UNSPECIFIED.,.F.,.F.)
B_SPLINE_CURVE_WITH_KNOTS((6,1,1,1,1,1,1,1,1,1,1,1,1,1,1,1,1,1,1,1,1,1,
1,1,1,1,1,1,1,1,1,1,1,1,1,1,1,1,1,1,1,1,1,1,1,1,1,1,1,1,1,1,1,1,1,1,1,1,
1,1,1,1,1,1,1,6),(0.,0.0153846153846154,0.0307692307692308,0.0461538461538462,
0.0615384615384615,0.0769230769230769,0.0923076923076923,0.107692307692308,
0.123076923076923,0.138461538461538,0.153846153846154,0.169230769230769,
0.184615384615385,0.2,0.215384615384615,0.230769230769231,0.246153846153846,
0.261538461538462,0.276923076923077,0.292307692307692,0.307692307692308,
0.323076923076923,0.338461538461538,0.353846153846154,0.369230769230769,
0.384615384615385,0.4,0.415384615384615,0.430769230769231,0.446153846153846,
0.461538461538462,0.476923076923077,0.492307692307692,0.507692307692308,
0.523076923076923,0.538461538461538,0.553846153846154,0.569230769230769,
0.584615384615384,0.6,0.615384615384615,0.63076923076923,0.646153846153846,
0.661538461538461,0.676923076923076,0.692307692307692,0.707692307692307,
0.723076923076922,0.738461538461538,0.753846153846153,0.769230769230768,
0.784615384615384,0.799999999999999,0.815384615384614,0.83076923076923,
0.846153846153845,0.86153846153846,0.876923076923076,0.892307692307691,
0.907692307692306,0.923076923076922,0.938461538461537,0.953846153846152,
0.969230769230768,0.984615384615383,1.),.UNSPECIFIED.)
CURVE()
GEOMETRIC_REPRESENTATION_ITEM()
RATIONAL_B_SPLINE_CURVE((1.,1.,1.,1.,1.,1.,1.,1.,1.,1.,1.,1.,1.,1.,1.,1.,
1.,1.,1.,1.,1.,1.,1.,1.,1.,1.,1.,1.,1.,1.,1.,1.,1.,1.,1.,1.,1.,1.,1.,1.,
1.,1.,1.,1.,1.,1.,1.,1.,1.,1.,1.,1.,1.,1.,1.,1.,1.,1.,1.,1.,1.,1.,1.,1.,
1.,1.,1.,1.,1.,1.))
REPRESENTATION_ITEM('')
);
#137=(
BOUNDED_CURVE()
B_SPLINE_CURVE(5,(#18653,#18654,#18655,#18656,#18657,#18658,#18659,#18660,
#18661,#18662,#18663,#18664,#18665,#18666,#18667,#18668,#18669,#18670,#18671,
#18672,#18673,#18674,#18675,#18676,#18677,#18678,#18679,#18680,#18681,#18682,
#18683,#18684,#18685,#18686,#18687,#18688,#18689,#18690,#18691,#18692,#18693,
#18694,#18695,#18696,#18697,#18698,#18699,#18700,#18701,#18702,#18703,#18704,
#18705,#18706,#18707,#18708,#18709,#18710,#18711,#18712,#18713,#18714,#18715,
#18716,#18717,#18718,#18719,#18720,#18721,#18722),.UNSPECIFIED.,.F.,.F.)
B_SPLINE_CURVE_WITH_KNOTS((6,1,1,1,1,1,1,1,1,1,1,1,1,1,1,1,1,1,1,1,1,1,
1,1,1,1,1,1,1,1,1,1,1,1,1,1,1,1,1,1,1,1,1,1,1,1,1,1,1,1,1,1,1,1,1,1,1,1,
1,1,1,1,1,1,1,6),(0.,0.0153846153846154,0.0307692307692308,0.0461538461538462,
0.0615384615384615,0.0769230769230769,0.0923076923076923,0.107692307692308,
0.123076923076923,0.138461538461538,0.153846153846154,0.169230769230769,
0.184615384615385,0.2,0.215384615384615,0.230769230769231,0.246153846153846,
0.261538461538462,0.276923076923077,0.292307692307692,0.307692307692308,
0.323076923076923,0.338461538461538,0.353846153846154,0.369230769230769,
0.384615384615385,0.4,0.415384615384615,0.430769230769231,0.446153846153846,
0.461538461538462,0.476923076923077,0.492307692307692,0.507692307692308,
0.523076923076923,0.538461538461538,0.553846153846154,0.569230769230769,
0.584615384615384,0.6,0.615384615384615,0.63076923076923,0.646153846153846,
0.661538461538461,0.676923076923076,0.692307692307692,0.707692307692307,
0.723076923076922,0.738461538461538,0.753846153846153,0.769230769230768,
0.784615384615384,0.799999999999999,0.815384615384614,0.83076923076923,
0.846153846153845,0.86153846153846,0.876923076923076,0.892307692307691,
0.907692307692306,0.923076923076922,0.938461538461537,0.953846153846152,
0.969230769230768,0.984615384615383,1.),.UNSPECIFIED.)
CURVE()
GEOMETRIC_REPRESENTATION_ITEM()
RATIONAL_B_SPLINE_CURVE((1.,1.,1.,1.,1.,1.,1.,1.,1.,1.,1.,1.,1.,1.,1.,1.,
1.,1.,1.,1.,1.,1.,1.,1.,1.,1.,1.,1.,1.,1.,1.,1.,1.,1.,1.,1.,1.,1.,1.,1.,
1.,1.,1.,1.,1.,1.,1.,1.,1.,1.,1.,1.,1.,1.,1.,1.,1.,1.,1.,1.,1.,1.,1.,1.,
1.,1.,1.,1.,1.,1.))
REPRESENTATION_ITEM('')
);
#138=(
BOUNDED_CURVE()
B_SPLINE_CURVE(5,(#18726,#18727,#18728,#18729,#18730,#18731,#18732,#18733,
#18734,#18735,#18736,#18737,#18738,#18739,#18740,#18741,#18742,#18743,#18744,
#18745,#18746,#18747,#18748,#18749,#18750,#18751,#18752,#18753,#18754,#18755,
#18756,#18757,#18758,#18759,#18760,#18761,#18762,#18763,#18764,#18765,#18766,
#18767,#18768,#18769,#18770,#18771,#18772,#18773,#18774,#18775,#18776,#18777,
#18778,#18779,#18780,#18781,#18782,#18783,#18784,#18785,#18786,#18787,#18788,
#18789,#18790,#18791,#18792,#18793,#18794,#18795),.UNSPECIFIED.,.F.,.F.)
B_SPLINE_CURVE_WITH_KNOTS((6,1,1,1,1,1,1,1,1,1,1,1,1,1,1,1,1,1,1,1,1,1,
1,1,1,1,1,1,1,1,1,1,1,1,1,1,1,1,1,1,1,1,1,1,1,1,1,1,1,1,1,1,1,1,1,1,1,1,
1,1,1,1,1,1,1,6),(0.,0.0153846153846154,0.0307692307692308,0.0461538461538462,
0.0615384615384615,0.0769230769230769,0.0923076923076923,0.107692307692308,
0.123076923076923,0.138461538461538,0.153846153846154,0.169230769230769,
0.184615384615385,0.2,0.215384615384615,0.230769230769231,0.246153846153846,
0.261538461538462,0.276923076923077,0.292307692307692,0.307692307692308,
0.323076923076923,0.338461538461538,0.353846153846154,0.369230769230769,
0.384615384615385,0.4,0.415384615384615,0.430769230769231,0.446153846153846,
0.461538461538462,0.476923076923077,0.492307692307692,0.507692307692308,
0.523076923076923,0.538461538461538,0.553846153846154,0.569230769230769,
0.584615384615384,0.6,0.615384615384615,0.63076923076923,0.646153846153846,
0.661538461538461,0.676923076923076,0.692307692307692,0.707692307692307,
0.723076923076922,0.738461538461538,0.753846153846153,0.769230769230768,
0.784615384615384,0.799999999999999,0.815384615384614,0.83076923076923,
0.846153846153845,0.86153846153846,0.876923076923076,0.892307692307691,
0.907692307692306,0.923076923076922,0.938461538461537,0.953846153846152,
0.969230769230768,0.984615384615383,1.),.UNSPECIFIED.)
CURVE()
GEOMETRIC_REPRESENTATION_ITEM()
RATIONAL_B_SPLINE_CURVE((1.,1.,1.,1.,1.,1.,1.,1.,1.,1.,1.,1.,1.,1.,1.,1.,
1.,1.,1.,1.,1.,1.,1.,1.,1.,1.,1.,1.,1.,1.,1.,1.,1.,1.,1.,1.,1.,1.,1.,1.,
1.,1.,1.,1.,1.,1.,1.,1.,1.,1.,1.,1.,1.,1.,1.,1.,1.,1.,1.,1.,1.,1.,1.,1.,
1.,1.,1.,1.,1.,1.))
REPRESENTATION_ITEM('')
);
#139=(
BOUNDED_CURVE()
B_SPLINE_CURVE(5,(#18799,#18800,#18801,#18802,#18803,#18804,#18805,#18806,
#18807,#18808,#18809,#18810,#18811,#18812,#18813,#18814,#18815,#18816,#18817,
#18818,#18819,#18820,#18821,#18822,#18823,#18824,#18825,#18826,#18827,#18828,
#18829,#18830,#18831,#18832,#18833,#18834,#18835,#18836,#18837,#18838,#18839,
#18840,#18841,#18842,#18843,#18844,#18845,#18846,#18847,#18848,#18849,#18850,
#18851,#18852,#18853,#18854,#18855,#18856,#18857,#18858,#18859,#18860,#18861,
#18862,#18863,#18864,#18865,#18866,#18867,#18868),.UNSPECIFIED.,.F.,.F.)
B_SPLINE_CURVE_WITH_KNOTS((6,1,1,1,1,1,1,1,1,1,1,1,1,1,1,1,1,1,1,1,1,1,
1,1,1,1,1,1,1,1,1,1,1,1,1,1,1,1,1,1,1,1,1,1,1,1,1,1,1,1,1,1,1,1,1,1,1,1,
1,1,1,1,1,1,1,6),(0.,0.0153846153846154,0.0307692307692308,0.0461538461538462,
0.0615384615384615,0.0769230769230769,0.0923076923076923,0.107692307692308,
0.123076923076923,0.138461538461538,0.153846153846154,0.169230769230769,
0.184615384615385,0.2,0.215384615384615,0.230769230769231,0.246153846153846,
0.261538461538462,0.276923076923077,0.292307692307692,0.307692307692308,
0.323076923076923,0.338461538461538,0.353846153846154,0.369230769230769,
0.384615384615385,0.4,0.415384615384615,0.430769230769231,0.446153846153846,
0.461538461538462,0.476923076923077,0.492307692307692,0.507692307692308,
0.523076923076923,0.538461538461538,0.553846153846154,0.569230769230769,
0.584615384615384,0.6,0.615384615384615,0.63076923076923,0.646153846153846,
0.661538461538461,0.676923076923076,0.692307692307692,0.707692307692307,
0.723076923076922,0.738461538461538,0.753846153846153,0.769230769230768,
0.784615384615384,0.799999999999999,0.815384615384614,0.83076923076923,
0.846153846153845,0.86153846153846,0.876923076923076,0.892307692307691,
0.907692307692306,0.923076923076922,0.938461538461537,0.953846153846152,
0.969230769230768,0.984615384615383,1.),.UNSPECIFIED.)
CURVE()
GEOMETRIC_REPRESENTATION_ITEM()
RATIONAL_B_SPLINE_CURVE((1.,1.,1.,1.,1.,1.,1.,1.,1.,1.,1.,1.,1.,1.,1.,1.,
1.,1.,1.,1.,1.,1.,1.,1.,1.,1.,1.,1.,1.,1.,1.,1.,1.,1.,1.,1.,1.,1.,1.,1.,
1.,1.,1.,1.,1.,1.,1.,1.,1.,1.,1.,1.,1.,1.,1.,1.,1.,1.,1.,1.,1.,1.,1.,1.,
1.,1.,1.,1.,1.,1.))
REPRESENTATION_ITEM('')
);
#140=(
BOUNDED_CURVE()
B_SPLINE_CURVE(5,(#18872,#18873,#18874,#18875,#18876,#18877,#18878,#18879,
#18880,#18881,#18882,#18883,#18884,#18885,#18886,#18887,#18888,#18889,#18890,
#18891,#18892,#18893,#18894,#18895,#18896,#18897,#18898,#18899,#18900,#18901,
#18902,#18903,#18904,#18905,#18906,#18907,#18908,#18909,#18910,#18911,#18912,
#18913,#18914,#18915,#18916,#18917,#18918,#18919,#18920,#18921,#18922,#18923,
#18924,#18925,#18926,#18927,#18928,#18929,#18930,#18931,#18932,#18933,#18934,
#18935,#18936,#18937,#18938,#18939,#18940,#18941),.UNSPECIFIED.,.F.,.F.)
B_SPLINE_CURVE_WITH_KNOTS((6,1,1,1,1,1,1,1,1,1,1,1,1,1,1,1,1,1,1,1,1,1,
1,1,1,1,1,1,1,1,1,1,1,1,1,1,1,1,1,1,1,1,1,1,1,1,1,1,1,1,1,1,1,1,1,1,1,1,
1,1,1,1,1,1,1,6),(0.,0.0153846153846154,0.0307692307692308,0.0461538461538462,
0.0615384615384615,0.0769230769230769,0.0923076923076923,0.107692307692308,
0.123076923076923,0.138461538461538,0.153846153846154,0.169230769230769,
0.184615384615385,0.2,0.215384615384615,0.230769230769231,0.246153846153846,
0.261538461538462,0.276923076923077,0.292307692307692,0.307692307692308,
0.323076923076923,0.338461538461538,0.353846153846154,0.369230769230769,
0.384615384615385,0.4,0.415384615384615,0.430769230769231,0.446153846153846,
0.461538461538462,0.476923076923077,0.492307692307692,0.507692307692308,
0.523076923076923,0.538461538461538,0.553846153846154,0.569230769230769,
0.584615384615384,0.6,0.615384615384615,0.63076923076923,0.646153846153846,
0.661538461538461,0.676923076923076,0.692307692307692,0.707692307692307,
0.723076923076922,0.738461538461538,0.753846153846153,0.769230769230768,
0.784615384615384,0.799999999999999,0.815384615384614,0.83076923076923,
0.846153846153845,0.86153846153846,0.876923076923076,0.892307692307691,
0.907692307692306,0.923076923076922,0.938461538461537,0.953846153846152,
0.969230769230768,0.984615384615383,1.),.UNSPECIFIED.)
CURVE()
GEOMETRIC_REPRESENTATION_ITEM()
RATIONAL_B_SPLINE_CURVE((1.,1.,1.,1.,1.,1.,1.,1.,1.,1.,1.,1.,1.,1.,1.,1.,
1.,1.,1.,1.,1.,1.,1.,1.,1.,1.,1.,1.,1.,1.,1.,1.,1.,1.,1.,1.,1.,1.,1.,1.,
1.,1.,1.,1.,1.,1.,1.,1.,1.,1.,1.,1.,1.,1.,1.,1.,1.,1.,1.,1.,1.,1.,1.,1.,
1.,1.,1.,1.,1.,1.))
REPRESENTATION_ITEM('')
);
#141=(
BOUNDED_CURVE()
B_SPLINE_CURVE(5,(#18945,#18946,#18947,#18948,#18949,#18950,#18951,#18952,
#18953,#18954,#18955,#18956,#18957,#18958,#18959,#18960,#18961,#18962,#18963,
#18964,#18965,#18966,#18967,#18968,#18969,#18970,#18971,#18972,#18973,#18974,
#18975,#18976,#18977,#18978,#18979,#18980,#18981,#18982,#18983,#18984,#18985,
#18986,#18987,#18988,#18989,#18990,#18991,#18992,#18993,#18994,#18995,#18996,
#18997,#18998,#18999,#19000,#19001,#19002,#19003,#19004,#19005,#19006,#19007,
#19008,#19009,#19010,#19011,#19012,#19013,#19014),.UNSPECIFIED.,.F.,.F.)
B_SPLINE_CURVE_WITH_KNOTS((6,1,1,1,1,1,1,1,1,1,1,1,1,1,1,1,1,1,1,1,1,1,
1,1,1,1,1,1,1,1,1,1,1,1,1,1,1,1,1,1,1,1,1,1,1,1,1,1,1,1,1,1,1,1,1,1,1,1,
1,1,1,1,1,1,1,6),(0.,0.0153846153846154,0.0307692307692308,0.0461538461538462,
0.0615384615384615,0.0769230769230769,0.0923076923076923,0.107692307692308,
0.123076923076923,0.138461538461538,0.153846153846154,0.169230769230769,
0.184615384615385,0.2,0.215384615384615,0.230769230769231,0.246153846153846,
0.261538461538462,0.276923076923077,0.292307692307692,0.307692307692308,
0.323076923076923,0.338461538461538,0.353846153846154,0.369230769230769,
0.384615384615385,0.4,0.415384615384615,0.430769230769231,0.446153846153846,
0.461538461538462,0.476923076923077,0.492307692307692,0.507692307692308,
0.523076923076923,0.538461538461538,0.553846153846154,0.569230769230769,
0.584615384615384,0.6,0.615384615384615,0.63076923076923,0.646153846153846,
0.661538461538461,0.676923076923076,0.692307692307692,0.707692307692307,
0.723076923076922,0.738461538461538,0.753846153846153,0.769230769230768,
0.784615384615384,0.799999999999999,0.815384615384614,0.83076923076923,
0.846153846153845,0.86153846153846,0.876923076923076,0.892307692307691,
0.907692307692306,0.923076923076922,0.938461538461537,0.953846153846152,
0.969230769230768,0.984615384615383,1.),.UNSPECIFIED.)
CURVE()
GEOMETRIC_REPRESENTATION_ITEM()
RATIONAL_B_SPLINE_CURVE((1.,1.,1.,1.,1.,1.,1.,1.,1.,1.,1.,1.,1.,1.,1.,1.,
1.,1.,1.,1.,1.,1.,1.,1.,1.,1.,1.,1.,1.,1.,1.,1.,1.,1.,1.,1.,1.,1.,1.,1.,
1.,1.,1.,1.,1.,1.,1.,1.,1.,1.,1.,1.,1.,1.,1.,1.,1.,1.,1.,1.,1.,1.,1.,1.,
1.,1.,1.,1.,1.,1.))
REPRESENTATION_ITEM('')
);
#142=(
BOUNDED_CURVE()
B_SPLINE_CURVE(5,(#19018,#19019,#19020,#19021,#19022,#19023,#19024,#19025,
#19026,#19027,#19028,#19029,#19030,#19031,#19032,#19033,#19034,#19035,#19036,
#19037,#19038,#19039,#19040,#19041,#19042,#19043,#19044,#19045,#19046,#19047,
#19048,#19049,#19050,#19051,#19052,#19053,#19054,#19055,#19056,#19057,#19058,
#19059,#19060,#19061,#19062,#19063,#19064,#19065,#19066,#19067,#19068,#19069,
#19070,#19071,#19072,#19073,#19074,#19075,#19076,#19077,#19078,#19079,#19080,
#19081,#19082,#19083,#19084,#19085,#19086,#19087),.UNSPECIFIED.,.F.,.F.)
B_SPLINE_CURVE_WITH_KNOTS((6,1,1,1,1,1,1,1,1,1,1,1,1,1,1,1,1,1,1,1,1,1,
1,1,1,1,1,1,1,1,1,1,1,1,1,1,1,1,1,1,1,1,1,1,1,1,1,1,1,1,1,1,1,1,1,1,1,1,
1,1,1,1,1,1,1,6),(0.,0.0153846153846154,0.0307692307692308,0.0461538461538462,
0.0615384615384615,0.0769230769230769,0.0923076923076923,0.107692307692308,
0.123076923076923,0.138461538461538,0.153846153846154,0.169230769230769,
0.184615384615385,0.2,0.215384615384615,0.230769230769231,0.246153846153846,
0.261538461538462,0.276923076923077,0.292307692307692,0.307692307692308,
0.323076923076923,0.338461538461538,0.353846153846154,0.369230769230769,
0.384615384615385,0.4,0.415384615384615,0.430769230769231,0.446153846153846,
0.461538461538462,0.476923076923077,0.492307692307692,0.507692307692308,
0.523076923076923,0.538461538461538,0.553846153846154,0.569230769230769,
0.584615384615384,0.6,0.615384615384615,0.63076923076923,0.646153846153846,
0.661538461538461,0.676923076923076,0.692307692307692,0.707692307692307,
0.723076923076922,0.738461538461538,0.753846153846153,0.769230769230768,
0.784615384615384,0.799999999999999,0.815384615384614,0.83076923076923,
0.846153846153845,0.86153846153846,0.876923076923076,0.892307692307691,
0.907692307692306,0.923076923076922,0.938461538461537,0.953846153846152,
0.969230769230768,0.984615384615383,1.),.UNSPECIFIED.)
CURVE()
GEOMETRIC_REPRESENTATION_ITEM()
RATIONAL_B_SPLINE_CURVE((1.,1.,1.,1.,1.,1.,1.,1.,1.,1.,1.,1.,1.,1.,1.,1.,
1.,1.,1.,1.,1.,1.,1.,1.,1.,1.,1.,1.,1.,1.,1.,1.,1.,1.,1.,1.,1.,1.,1.,1.,
1.,1.,1.,1.,1.,1.,1.,1.,1.,1.,1.,1.,1.,1.,1.,1.,1.,1.,1.,1.,1.,1.,1.,1.,
1.,1.,1.,1.,1.,1.))
REPRESENTATION_ITEM('')
);
#143=(
BOUNDED_CURVE()
B_SPLINE_CURVE(5,(#19091,#19092,#19093,#19094,#19095,#19096,#19097,#19098,
#19099,#19100,#19101,#19102,#19103,#19104,#19105,#19106,#19107,#19108,#19109,
#19110,#19111,#19112,#19113,#19114,#19115,#19116,#19117,#19118,#19119,#19120,
#19121,#19122,#19123,#19124,#19125,#19126,#19127,#19128,#19129,#19130,#19131,
#19132,#19133,#19134,#19135,#19136,#19137,#19138,#19139,#19140,#19141,#19142,
#19143,#19144,#19145,#19146,#19147,#19148,#19149,#19150,#19151,#19152,#19153,
#19154,#19155,#19156,#19157,#19158,#19159,#19160),.UNSPECIFIED.,.F.,.F.)
B_SPLINE_CURVE_WITH_KNOTS((6,1,1,1,1,1,1,1,1,1,1,1,1,1,1,1,1,1,1,1,1,1,
1,1,1,1,1,1,1,1,1,1,1,1,1,1,1,1,1,1,1,1,1,1,1,1,1,1,1,1,1,1,1,1,1,1,1,1,
1,1,1,1,1,1,1,6),(0.,0.0153846153846154,0.0307692307692308,0.0461538461538462,
0.0615384615384615,0.0769230769230769,0.0923076923076923,0.107692307692308,
0.123076923076923,0.138461538461538,0.153846153846154,0.169230769230769,
0.184615384615385,0.2,0.215384615384615,0.230769230769231,0.246153846153846,
0.261538461538462,0.276923076923077,0.292307692307692,0.307692307692308,
0.323076923076923,0.338461538461538,0.353846153846154,0.369230769230769,
0.384615384615385,0.4,0.415384615384615,0.430769230769231,0.446153846153846,
0.461538461538462,0.476923076923077,0.492307692307692,0.507692307692308,
0.523076923076923,0.538461538461538,0.553846153846154,0.569230769230769,
0.584615384615384,0.6,0.615384615384615,0.63076923076923,0.646153846153846,
0.661538461538461,0.676923076923076,0.692307692307692,0.707692307692307,
0.723076923076922,0.738461538461538,0.753846153846153,0.769230769230768,
0.784615384615384,0.799999999999999,0.815384615384614,0.83076923076923,
0.846153846153845,0.86153846153846,0.876923076923076,0.892307692307691,
0.907692307692306,0.923076923076922,0.938461538461537,0.953846153846152,
0.969230769230768,0.984615384615383,1.),.UNSPECIFIED.)
CURVE()
GEOMETRIC_REPRESENTATION_ITEM()
RATIONAL_B_SPLINE_CURVE((1.,1.,1.,1.,1.,1.,1.,1.,1.,1.,1.,1.,1.,1.,1.,1.,
1.,1.,1.,1.,1.,1.,1.,1.,1.,1.,1.,1.,1.,1.,1.,1.,1.,1.,1.,1.,1.,1.,1.,1.,
1.,1.,1.,1.,1.,1.,1.,1.,1.,1.,1.,1.,1.,1.,1.,1.,1.,1.,1.,1.,1.,1.,1.,1.,
1.,1.,1.,1.,1.,1.))
REPRESENTATION_ITEM('')
);
#144=(
BOUNDED_CURVE()
B_SPLINE_CURVE(5,(#19164,#19165,#19166,#19167,#19168,#19169,#19170,#19171,
#19172,#19173,#19174,#19175,#19176,#19177,#19178,#19179,#19180,#19181,#19182,
#19183,#19184,#19185,#19186,#19187,#19188,#19189,#19190,#19191,#19192,#19193,
#19194,#19195,#19196,#19197,#19198,#19199,#19200,#19201,#19202,#19203,#19204,
#19205,#19206,#19207,#19208,#19209,#19210,#19211,#19212,#19213,#19214,#19215,
#19216,#19217,#19218,#19219,#19220,#19221,#19222,#19223,#19224,#19225,#19226,
#19227,#19228,#19229,#19230,#19231,#19232,#19233),.UNSPECIFIED.,.F.,.F.)
B_SPLINE_CURVE_WITH_KNOTS((6,1,1,1,1,1,1,1,1,1,1,1,1,1,1,1,1,1,1,1,1,1,
1,1,1,1,1,1,1,1,1,1,1,1,1,1,1,1,1,1,1,1,1,1,1,1,1,1,1,1,1,1,1,1,1,1,1,1,
1,1,1,1,1,1,1,6),(0.,0.0153846153846154,0.0307692307692308,0.0461538461538462,
0.0615384615384615,0.0769230769230769,0.0923076923076923,0.107692307692308,
0.123076923076923,0.138461538461538,0.153846153846154,0.169230769230769,
0.184615384615385,0.2,0.215384615384615,0.230769230769231,0.246153846153846,
0.261538461538462,0.276923076923077,0.292307692307692,0.307692307692308,
0.323076923076923,0.338461538461538,0.353846153846154,0.369230769230769,
0.384615384615385,0.4,0.415384615384615,0.430769230769231,0.446153846153846,
0.461538461538462,0.476923076923077,0.492307692307692,0.507692307692308,
0.523076923076923,0.538461538461538,0.553846153846154,0.569230769230769,
0.584615384615384,0.6,0.615384615384615,0.63076923076923,0.646153846153846,
0.661538461538461,0.676923076923076,0.692307692307692,0.707692307692307,
0.723076923076922,0.738461538461538,0.753846153846153,0.769230769230768,
0.784615384615384,0.799999999999999,0.815384615384614,0.83076923076923,
0.846153846153845,0.86153846153846,0.876923076923076,0.892307692307691,
0.907692307692306,0.923076923076922,0.938461538461537,0.953846153846152,
0.969230769230768,0.984615384615383,1.),.UNSPECIFIED.)
CURVE()
GEOMETRIC_REPRESENTATION_ITEM()
RATIONAL_B_SPLINE_CURVE((1.,1.,1.,1.,1.,1.,1.,1.,1.,1.,1.,1.,1.,1.,1.,1.,
1.,1.,1.,1.,1.,1.,1.,1.,1.,1.,1.,1.,1.,1.,1.,1.,1.,1.,1.,1.,1.,1.,1.,1.,
1.,1.,1.,1.,1.,1.,1.,1.,1.,1.,1.,1.,1.,1.,1.,1.,1.,1.,1.,1.,1.,1.,1.,1.,
1.,1.,1.,1.,1.,1.))
REPRESENTATION_ITEM('')
);
#145=(
BOUNDED_CURVE()
B_SPLINE_CURVE(5,(#19237,#19238,#19239,#19240,#19241,#19242,#19243,#19244,
#19245,#19246,#19247,#19248,#19249,#19250,#19251,#19252,#19253,#19254,#19255,
#19256,#19257,#19258,#19259,#19260,#19261,#19262,#19263,#19264,#19265,#19266,
#19267,#19268,#19269,#19270,#19271,#19272,#19273,#19274,#19275,#19276,#19277,
#19278,#19279,#19280,#19281,#19282,#19283,#19284,#19285,#19286,#19287,#19288,
#19289,#19290,#19291,#19292,#19293,#19294,#19295,#19296,#19297,#19298,#19299,
#19300,#19301,#19302,#19303,#19304,#19305,#19306),.UNSPECIFIED.,.F.,.F.)
B_SPLINE_CURVE_WITH_KNOTS((6,1,1,1,1,1,1,1,1,1,1,1,1,1,1,1,1,1,1,1,1,1,
1,1,1,1,1,1,1,1,1,1,1,1,1,1,1,1,1,1,1,1,1,1,1,1,1,1,1,1,1,1,1,1,1,1,1,1,
1,1,1,1,1,1,1,6),(0.,0.0153846153846154,0.0307692307692308,0.0461538461538462,
0.0615384615384615,0.0769230769230769,0.0923076923076923,0.107692307692308,
0.123076923076923,0.138461538461538,0.153846153846154,0.169230769230769,
0.184615384615385,0.2,0.215384615384615,0.230769230769231,0.246153846153846,
0.261538461538462,0.276923076923077,0.292307692307692,0.307692307692308,
0.323076923076923,0.338461538461538,0.353846153846154,0.369230769230769,
0.384615384615385,0.4,0.415384615384615,0.430769230769231,0.446153846153846,
0.461538461538462,0.476923076923077,0.492307692307692,0.507692307692308,
0.523076923076923,0.538461538461538,0.553846153846154,0.569230769230769,
0.584615384615384,0.6,0.615384615384615,0.63076923076923,0.646153846153846,
0.661538461538461,0.676923076923076,0.692307692307692,0.707692307692307,
0.723076923076922,0.738461538461538,0.753846153846153,0.769230769230768,
0.784615384615384,0.799999999999999,0.815384615384614,0.83076923076923,
0.846153846153845,0.86153846153846,0.876923076923076,0.892307692307691,
0.907692307692306,0.923076923076922,0.938461538461537,0.953846153846152,
0.969230769230768,0.984615384615383,1.),.UNSPECIFIED.)
CURVE()
GEOMETRIC_REPRESENTATION_ITEM()
RATIONAL_B_SPLINE_CURVE((1.,1.,1.,1.,1.,1.,1.,1.,1.,1.,1.,1.,1.,1.,1.,1.,
1.,1.,1.,1.,1.,1.,1.,1.,1.,1.,1.,1.,1.,1.,1.,1.,1.,1.,1.,1.,1.,1.,1.,1.,
1.,1.,1.,1.,1.,1.,1.,1.,1.,1.,1.,1.,1.,1.,1.,1.,1.,1.,1.,1.,1.,1.,1.,1.,
1.,1.,1.,1.,1.,1.))
REPRESENTATION_ITEM('')
);
#146=(
BOUNDED_CURVE()
B_SPLINE_CURVE(5,(#19310,#19311,#19312,#19313,#19314,#19315,#19316,#19317,
#19318,#19319,#19320,#19321,#19322,#19323,#19324,#19325,#19326,#19327,#19328,
#19329,#19330,#19331,#19332,#19333,#19334,#19335,#19336,#19337,#19338,#19339,
#19340,#19341,#19342,#19343,#19344,#19345,#19346,#19347,#19348,#19349,#19350,
#19351,#19352,#19353,#19354,#19355,#19356,#19357,#19358,#19359,#19360,#19361,
#19362,#19363,#19364,#19365,#19366,#19367,#19368,#19369,#19370,#19371,#19372,
#19373,#19374,#19375,#19376,#19377,#19378,#19379),.UNSPECIFIED.,.F.,.F.)
B_SPLINE_CURVE_WITH_KNOTS((6,1,1,1,1,1,1,1,1,1,1,1,1,1,1,1,1,1,1,1,1,1,
1,1,1,1,1,1,1,1,1,1,1,1,1,1,1,1,1,1,1,1,1,1,1,1,1,1,1,1,1,1,1,1,1,1,1,1,
1,1,1,1,1,1,1,6),(0.,0.0153846153846154,0.0307692307692308,0.0461538461538462,
0.0615384615384615,0.0769230769230769,0.0923076923076923,0.107692307692308,
0.123076923076923,0.138461538461538,0.153846153846154,0.169230769230769,
0.184615384615385,0.2,0.215384615384615,0.230769230769231,0.246153846153846,
0.261538461538462,0.276923076923077,0.292307692307692,0.307692307692308,
0.323076923076923,0.338461538461538,0.353846153846154,0.369230769230769,
0.384615384615385,0.4,0.415384615384615,0.430769230769231,0.446153846153846,
0.461538461538462,0.476923076923077,0.492307692307692,0.507692307692308,
0.523076923076923,0.538461538461538,0.553846153846154,0.569230769230769,
0.584615384615384,0.6,0.615384615384615,0.63076923076923,0.646153846153846,
0.661538461538461,0.676923076923076,0.692307692307692,0.707692307692307,
0.723076923076922,0.738461538461538,0.753846153846153,0.769230769230768,
0.784615384615384,0.799999999999999,0.815384615384614,0.83076923076923,
0.846153846153845,0.86153846153846,0.876923076923076,0.892307692307691,
0.907692307692306,0.923076923076922,0.938461538461537,0.953846153846152,
0.969230769230768,0.984615384615383,1.),.UNSPECIFIED.)
CURVE()
GEOMETRIC_REPRESENTATION_ITEM()
RATIONAL_B_SPLINE_CURVE((1.,1.,1.,1.,1.,1.,1.,1.,1.,1.,1.,1.,1.,1.,1.,1.,
1.,1.,1.,1.,1.,1.,1.,1.,1.,1.,1.,1.,1.,1.,1.,1.,1.,1.,1.,1.,1.,1.,1.,1.,
1.,1.,1.,1.,1.,1.,1.,1.,1.,1.,1.,1.,1.,1.,1.,1.,1.,1.,1.,1.,1.,1.,1.,1.,
1.,1.,1.,1.,1.,1.))
REPRESENTATION_ITEM('')
);
#147=(
BOUNDED_CURVE()
B_SPLINE_CURVE(5,(#19383,#19384,#19385,#19386,#19387,#19388,#19389,#19390,
#19391,#19392,#19393,#19394,#19395,#19396,#19397,#19398,#19399,#19400,#19401,
#19402,#19403,#19404,#19405,#19406,#19407,#19408,#19409,#19410,#19411,#19412,
#19413,#19414,#19415,#19416,#19417,#19418,#19419,#19420,#19421,#19422,#19423,
#19424,#19425,#19426,#19427,#19428,#19429,#19430,#19431,#19432,#19433,#19434,
#19435,#19436,#19437,#19438,#19439,#19440,#19441,#19442,#19443,#19444,#19445,
#19446,#19447,#19448,#19449,#19450,#19451,#19452),.UNSPECIFIED.,.F.,.F.)
B_SPLINE_CURVE_WITH_KNOTS((6,1,1,1,1,1,1,1,1,1,1,1,1,1,1,1,1,1,1,1,1,1,
1,1,1,1,1,1,1,1,1,1,1,1,1,1,1,1,1,1,1,1,1,1,1,1,1,1,1,1,1,1,1,1,1,1,1,1,
1,1,1,1,1,1,1,6),(0.,0.0153846153846154,0.0307692307692308,0.0461538461538462,
0.0615384615384615,0.0769230769230769,0.0923076923076923,0.107692307692308,
0.123076923076923,0.138461538461538,0.153846153846154,0.169230769230769,
0.184615384615385,0.2,0.215384615384615,0.230769230769231,0.246153846153846,
0.261538461538462,0.276923076923077,0.292307692307692,0.307692307692308,
0.323076923076923,0.338461538461538,0.353846153846154,0.369230769230769,
0.384615384615385,0.4,0.415384615384615,0.430769230769231,0.446153846153846,
0.461538461538462,0.476923076923077,0.492307692307692,0.507692307692308,
0.523076923076923,0.538461538461538,0.553846153846154,0.569230769230769,
0.584615384615384,0.6,0.615384615384615,0.63076923076923,0.646153846153846,
0.661538461538461,0.676923076923076,0.692307692307692,0.707692307692307,
0.723076923076922,0.738461538461538,0.753846153846153,0.769230769230768,
0.784615384615384,0.799999999999999,0.815384615384614,0.83076923076923,
0.846153846153845,0.86153846153846,0.876923076923076,0.892307692307691,
0.907692307692306,0.923076923076922,0.938461538461537,0.953846153846152,
0.969230769230768,0.984615384615383,1.),.UNSPECIFIED.)
CURVE()
GEOMETRIC_REPRESENTATION_ITEM()
RATIONAL_B_SPLINE_CURVE((1.,1.,1.,1.,1.,1.,1.,1.,1.,1.,1.,1.,1.,1.,1.,1.,
1.,1.,1.,1.,1.,1.,1.,1.,1.,1.,1.,1.,1.,1.,1.,1.,1.,1.,1.,1.,1.,1.,1.,1.,
1.,1.,1.,1.,1.,1.,1.,1.,1.,1.,1.,1.,1.,1.,1.,1.,1.,1.,1.,1.,1.,1.,1.,1.,
1.,1.,1.,1.,1.,1.))
REPRESENTATION_ITEM('')
);
#148=(
BOUNDED_CURVE()
B_SPLINE_CURVE(5,(#19456,#19457,#19458,#19459,#19460,#19461,#19462,#19463,
#19464,#19465,#19466,#19467,#19468,#19469,#19470,#19471,#19472,#19473,#19474,
#19475,#19476,#19477,#19478,#19479,#19480,#19481,#19482,#19483,#19484,#19485,
#19486,#19487,#19488,#19489,#19490,#19491,#19492,#19493,#19494,#19495,#19496,
#19497,#19498,#19499,#19500,#19501,#19502,#19503,#19504,#19505,#19506,#19507,
#19508,#19509,#19510,#19511,#19512,#19513,#19514,#19515,#19516,#19517,#19518,
#19519,#19520,#19521,#19522,#19523,#19524,#19525),.UNSPECIFIED.,.F.,.F.)
B_SPLINE_CURVE_WITH_KNOTS((6,1,1,1,1,1,1,1,1,1,1,1,1,1,1,1,1,1,1,1,1,1,
1,1,1,1,1,1,1,1,1,1,1,1,1,1,1,1,1,1,1,1,1,1,1,1,1,1,1,1,1,1,1,1,1,1,1,1,
1,1,1,1,1,1,1,6),(0.,0.0153846153846154,0.0307692307692308,0.0461538461538462,
0.0615384615384615,0.0769230769230769,0.0923076923076923,0.107692307692308,
0.123076923076923,0.138461538461538,0.153846153846154,0.169230769230769,
0.184615384615385,0.2,0.215384615384615,0.230769230769231,0.246153846153846,
0.261538461538462,0.276923076923077,0.292307692307692,0.307692307692308,
0.323076923076923,0.338461538461538,0.353846153846154,0.369230769230769,
0.384615384615385,0.4,0.415384615384615,0.430769230769231,0.446153846153846,
0.461538461538462,0.476923076923077,0.492307692307692,0.507692307692308,
0.523076923076923,0.538461538461538,0.553846153846154,0.569230769230769,
0.584615384615384,0.6,0.615384615384615,0.63076923076923,0.646153846153846,
0.661538461538461,0.676923076923076,0.692307692307692,0.707692307692307,
0.723076923076922,0.738461538461538,0.753846153846153,0.769230769230768,
0.784615384615384,0.799999999999999,0.815384615384614,0.83076923076923,
0.846153846153845,0.86153846153846,0.876923076923076,0.892307692307691,
0.907692307692306,0.923076923076922,0.938461538461537,0.953846153846152,
0.969230769230768,0.984615384615383,1.),.UNSPECIFIED.)
CURVE()
GEOMETRIC_REPRESENTATION_ITEM()
RATIONAL_B_SPLINE_CURVE((1.,1.,1.,1.,1.,1.,1.,1.,1.,1.,1.,1.,1.,1.,1.,1.,
1.,1.,1.,1.,1.,1.,1.,1.,1.,1.,1.,1.,1.,1.,1.,1.,1.,1.,1.,1.,1.,1.,1.,1.,
1.,1.,1.,1.,1.,1.,1.,1.,1.,1.,1.,1.,1.,1.,1.,1.,1.,1.,1.,1.,1.,1.,1.,1.,
1.,1.,1.,1.,1.,1.))
REPRESENTATION_ITEM('')
);
#149=(
BOUNDED_CURVE()
B_SPLINE_CURVE(5,(#19529,#19530,#19531,#19532,#19533,#19534,#19535,#19536,
#19537,#19538,#19539,#19540,#19541,#19542,#19543,#19544,#19545,#19546,#19547,
#19548,#19549,#19550,#19551,#19552,#19553,#19554,#19555,#19556,#19557,#19558,
#19559,#19560,#19561,#19562,#19563,#19564,#19565,#19566,#19567,#19568,#19569,
#19570,#19571,#19572,#19573,#19574,#19575,#19576,#19577,#19578,#19579,#19580,
#19581,#19582,#19583,#19584,#19585,#19586,#19587,#19588,#19589,#19590,#19591,
#19592,#19593,#19594,#19595,#19596,#19597,#19598),.UNSPECIFIED.,.F.,.F.)
B_SPLINE_CURVE_WITH_KNOTS((6,1,1,1,1,1,1,1,1,1,1,1,1,1,1,1,1,1,1,1,1,1,
1,1,1,1,1,1,1,1,1,1,1,1,1,1,1,1,1,1,1,1,1,1,1,1,1,1,1,1,1,1,1,1,1,1,1,1,
1,1,1,1,1,1,1,6),(0.,0.0153846153846154,0.0307692307692308,0.0461538461538462,
0.0615384615384615,0.0769230769230769,0.0923076923076923,0.107692307692308,
0.123076923076923,0.138461538461538,0.153846153846154,0.169230769230769,
0.184615384615385,0.2,0.215384615384615,0.230769230769231,0.246153846153846,
0.261538461538462,0.276923076923077,0.292307692307692,0.307692307692308,
0.323076923076923,0.338461538461538,0.353846153846154,0.369230769230769,
0.384615384615385,0.4,0.415384615384615,0.430769230769231,0.446153846153846,
0.461538461538462,0.476923076923077,0.492307692307692,0.507692307692308,
0.523076923076923,0.538461538461538,0.553846153846154,0.569230769230769,
0.584615384615384,0.6,0.615384615384615,0.63076923076923,0.646153846153846,
0.661538461538461,0.676923076923076,0.692307692307692,0.707692307692307,
0.723076923076922,0.738461538461538,0.753846153846153,0.769230769230768,
0.784615384615384,0.799999999999999,0.815384615384614,0.83076923076923,
0.846153846153845,0.86153846153846,0.876923076923076,0.892307692307691,
0.907692307692306,0.923076923076922,0.938461538461537,0.953846153846152,
0.969230769230768,0.984615384615383,1.),.UNSPECIFIED.)
CURVE()
GEOMETRIC_REPRESENTATION_ITEM()
RATIONAL_B_SPLINE_CURVE((1.,1.,1.,1.,1.,1.,1.,1.,1.,1.,1.,1.,1.,1.,1.,1.,
1.,1.,1.,1.,1.,1.,1.,1.,1.,1.,1.,1.,1.,1.,1.,1.,1.,1.,1.,1.,1.,1.,1.,1.,
1.,1.,1.,1.,1.,1.,1.,1.,1.,1.,1.,1.,1.,1.,1.,1.,1.,1.,1.,1.,1.,1.,1.,1.,
1.,1.,1.,1.,1.,1.))
REPRESENTATION_ITEM('')
);
#150=(
BOUNDED_CURVE()
B_SPLINE_CURVE(5,(#19602,#19603,#19604,#19605,#19606,#19607,#19608,#19609,
#19610,#19611,#19612,#19613,#19614,#19615,#19616,#19617,#19618,#19619,#19620,
#19621,#19622,#19623,#19624,#19625,#19626,#19627,#19628,#19629,#19630,#19631,
#19632,#19633,#19634,#19635,#19636,#19637,#19638,#19639,#19640,#19641,#19642,
#19643,#19644,#19645,#19646,#19647,#19648,#19649,#19650,#19651,#19652,#19653,
#19654,#19655,#19656,#19657,#19658,#19659,#19660,#19661,#19662,#19663,#19664,
#19665,#19666,#19667,#19668,#19669,#19670,#19671),.UNSPECIFIED.,.F.,.F.)
B_SPLINE_CURVE_WITH_KNOTS((6,1,1,1,1,1,1,1,1,1,1,1,1,1,1,1,1,1,1,1,1,1,
1,1,1,1,1,1,1,1,1,1,1,1,1,1,1,1,1,1,1,1,1,1,1,1,1,1,1,1,1,1,1,1,1,1,1,1,
1,1,1,1,1,1,1,6),(0.,0.0153846153846154,0.0307692307692308,0.0461538461538462,
0.0615384615384615,0.0769230769230769,0.0923076923076923,0.107692307692308,
0.123076923076923,0.138461538461538,0.153846153846154,0.169230769230769,
0.184615384615385,0.2,0.215384615384615,0.230769230769231,0.246153846153846,
0.261538461538462,0.276923076923077,0.292307692307692,0.307692307692308,
0.323076923076923,0.338461538461538,0.353846153846154,0.369230769230769,
0.384615384615385,0.4,0.415384615384615,0.430769230769231,0.446153846153846,
0.461538461538462,0.476923076923077,0.492307692307692,0.507692307692308,
0.523076923076923,0.538461538461538,0.553846153846154,0.569230769230769,
0.584615384615384,0.6,0.615384615384615,0.63076923076923,0.646153846153846,
0.661538461538461,0.676923076923076,0.692307692307692,0.707692307692307,
0.723076923076922,0.738461538461538,0.753846153846153,0.769230769230768,
0.784615384615384,0.799999999999999,0.815384615384614,0.83076923076923,
0.846153846153845,0.86153846153846,0.876923076923076,0.892307692307691,
0.907692307692306,0.923076923076922,0.938461538461537,0.953846153846152,
0.969230769230768,0.984615384615383,1.),.UNSPECIFIED.)
CURVE()
GEOMETRIC_REPRESENTATION_ITEM()
RATIONAL_B_SPLINE_CURVE((1.,1.,1.,1.,1.,1.,1.,1.,1.,1.,1.,1.,1.,1.,1.,1.,
1.,1.,1.,1.,1.,1.,1.,1.,1.,1.,1.,1.,1.,1.,1.,1.,1.,1.,1.,1.,1.,1.,1.,1.,
1.,1.,1.,1.,1.,1.,1.,1.,1.,1.,1.,1.,1.,1.,1.,1.,1.,1.,1.,1.,1.,1.,1.,1.,
1.,1.,1.,1.,1.,1.))
REPRESENTATION_ITEM('')
);
#151=(
BOUNDED_CURVE()
B_SPLINE_CURVE(5,(#19675,#19676,#19677,#19678,#19679,#19680,#19681,#19682,
#19683,#19684,#19685,#19686,#19687,#19688,#19689,#19690,#19691,#19692,#19693,
#19694,#19695,#19696,#19697,#19698,#19699,#19700,#19701,#19702,#19703,#19704,
#19705,#19706,#19707,#19708,#19709,#19710,#19711,#19712,#19713,#19714,#19715,
#19716,#19717,#19718,#19719,#19720,#19721,#19722,#19723,#19724,#19725,#19726,
#19727,#19728,#19729,#19730,#19731,#19732,#19733,#19734,#19735,#19736,#19737,
#19738,#19739,#19740,#19741,#19742,#19743,#19744),.UNSPECIFIED.,.F.,.F.)
B_SPLINE_CURVE_WITH_KNOTS((6,1,1,1,1,1,1,1,1,1,1,1,1,1,1,1,1,1,1,1,1,1,
1,1,1,1,1,1,1,1,1,1,1,1,1,1,1,1,1,1,1,1,1,1,1,1,1,1,1,1,1,1,1,1,1,1,1,1,
1,1,1,1,1,1,1,6),(0.,0.0153846153846154,0.0307692307692308,0.0461538461538462,
0.0615384615384615,0.0769230769230769,0.0923076923076923,0.107692307692308,
0.123076923076923,0.138461538461538,0.153846153846154,0.169230769230769,
0.184615384615385,0.2,0.215384615384615,0.230769230769231,0.246153846153846,
0.261538461538462,0.276923076923077,0.292307692307692,0.307692307692308,
0.323076923076923,0.338461538461538,0.353846153846154,0.369230769230769,
0.384615384615385,0.4,0.415384615384615,0.430769230769231,0.446153846153846,
0.461538461538462,0.476923076923077,0.492307692307692,0.507692307692308,
0.523076923076923,0.538461538461538,0.553846153846154,0.569230769230769,
0.584615384615384,0.6,0.615384615384615,0.63076923076923,0.646153846153846,
0.661538461538461,0.676923076923076,0.692307692307692,0.707692307692307,
0.723076923076922,0.738461538461538,0.753846153846153,0.769230769230768,
0.784615384615384,0.799999999999999,0.815384615384614,0.83076923076923,
0.846153846153845,0.86153846153846,0.876923076923076,0.892307692307691,
0.907692307692306,0.923076923076922,0.938461538461537,0.953846153846152,
0.969230769230768,0.984615384615383,1.),.UNSPECIFIED.)
CURVE()
GEOMETRIC_REPRESENTATION_ITEM()
RATIONAL_B_SPLINE_CURVE((1.,1.,1.,1.,1.,1.,1.,1.,1.,1.,1.,1.,1.,1.,1.,1.,
1.,1.,1.,1.,1.,1.,1.,1.,1.,1.,1.,1.,1.,1.,1.,1.,1.,1.,1.,1.,1.,1.,1.,1.,
1.,1.,1.,1.,1.,1.,1.,1.,1.,1.,1.,1.,1.,1.,1.,1.,1.,1.,1.,1.,1.,1.,1.,1.,
1.,1.,1.,1.,1.,1.))
REPRESENTATION_ITEM('')
);
#152=(
BOUNDED_CURVE()
B_SPLINE_CURVE(5,(#19748,#19749,#19750,#19751,#19752,#19753,#19754,#19755,
#19756,#19757,#19758,#19759,#19760,#19761,#19762,#19763,#19764,#19765,#19766,
#19767,#19768,#19769,#19770,#19771,#19772,#19773,#19774,#19775,#19776,#19777,
#19778,#19779,#19780,#19781,#19782,#19783,#19784,#19785,#19786,#19787,#19788,
#19789,#19790,#19791,#19792,#19793,#19794,#19795,#19796,#19797,#19798,#19799,
#19800,#19801,#19802,#19803,#19804,#19805,#19806,#19807,#19808,#19809,#19810,
#19811,#19812,#19813,#19814,#19815,#19816,#19817),.UNSPECIFIED.,.F.,.F.)
B_SPLINE_CURVE_WITH_KNOTS((6,1,1,1,1,1,1,1,1,1,1,1,1,1,1,1,1,1,1,1,1,1,
1,1,1,1,1,1,1,1,1,1,1,1,1,1,1,1,1,1,1,1,1,1,1,1,1,1,1,1,1,1,1,1,1,1,1,1,
1,1,1,1,1,1,1,6),(0.,0.0153846153846154,0.0307692307692308,0.0461538461538462,
0.0615384615384615,0.0769230769230769,0.0923076923076923,0.107692307692308,
0.123076923076923,0.138461538461538,0.153846153846154,0.169230769230769,
0.184615384615385,0.2,0.215384615384615,0.230769230769231,0.246153846153846,
0.261538461538462,0.276923076923077,0.292307692307692,0.307692307692308,
0.323076923076923,0.338461538461538,0.353846153846154,0.369230769230769,
0.384615384615385,0.4,0.415384615384615,0.430769230769231,0.446153846153846,
0.461538461538462,0.476923076923077,0.492307692307692,0.507692307692308,
0.523076923076923,0.538461538461538,0.553846153846154,0.569230769230769,
0.584615384615384,0.6,0.615384615384615,0.63076923076923,0.646153846153846,
0.661538461538461,0.676923076923076,0.692307692307692,0.707692307692307,
0.723076923076922,0.738461538461538,0.753846153846153,0.769230769230768,
0.784615384615384,0.799999999999999,0.815384615384614,0.83076923076923,
0.846153846153845,0.86153846153846,0.876923076923076,0.892307692307691,
0.907692307692306,0.923076923076922,0.938461538461537,0.953846153846152,
0.969230769230768,0.984615384615383,1.),.UNSPECIFIED.)
CURVE()
GEOMETRIC_REPRESENTATION_ITEM()
RATIONAL_B_SPLINE_CURVE((1.,1.,1.,1.,1.,1.,1.,1.,1.,1.,1.,1.,1.,1.,1.,1.,
1.,1.,1.,1.,1.,1.,1.,1.,1.,1.,1.,1.,1.,1.,1.,1.,1.,1.,1.,1.,1.,1.,1.,1.,
1.,1.,1.,1.,1.,1.,1.,1.,1.,1.,1.,1.,1.,1.,1.,1.,1.,1.,1.,1.,1.,1.,1.,1.,
1.,1.,1.,1.,1.,1.))
REPRESENTATION_ITEM('')
);
#153=(
BOUNDED_CURVE()
B_SPLINE_CURVE(5,(#19821,#19822,#19823,#19824,#19825,#19826,#19827,#19828,
#19829,#19830,#19831,#19832,#19833,#19834,#19835,#19836,#19837,#19838,#19839,
#19840,#19841,#19842,#19843,#19844,#19845,#19846,#19847,#19848,#19849,#19850,
#19851,#19852,#19853,#19854,#19855,#19856,#19857,#19858,#19859,#19860,#19861,
#19862,#19863,#19864,#19865,#19866,#19867,#19868,#19869,#19870,#19871,#19872,
#19873,#19874,#19875,#19876,#19877,#19878,#19879,#19880,#19881,#19882,#19883,
#19884,#19885,#19886,#19887,#19888,#19889,#19890),.UNSPECIFIED.,.F.,.F.)
B_SPLINE_CURVE_WITH_KNOTS((6,1,1,1,1,1,1,1,1,1,1,1,1,1,1,1,1,1,1,1,1,1,
1,1,1,1,1,1,1,1,1,1,1,1,1,1,1,1,1,1,1,1,1,1,1,1,1,1,1,1,1,1,1,1,1,1,1,1,
1,1,1,1,1,1,1,6),(0.,0.0153846153846154,0.0307692307692308,0.0461538461538462,
0.0615384615384615,0.0769230769230769,0.0923076923076923,0.107692307692308,
0.123076923076923,0.138461538461538,0.153846153846154,0.169230769230769,
0.184615384615385,0.2,0.215384615384615,0.230769230769231,0.246153846153846,
0.261538461538462,0.276923076923077,0.292307692307692,0.307692307692308,
0.323076923076923,0.338461538461538,0.353846153846154,0.369230769230769,
0.384615384615385,0.4,0.415384615384615,0.430769230769231,0.446153846153846,
0.461538461538462,0.476923076923077,0.492307692307692,0.507692307692308,
0.523076923076923,0.538461538461538,0.553846153846154,0.569230769230769,
0.584615384615384,0.6,0.615384615384615,0.63076923076923,0.646153846153846,
0.661538461538461,0.676923076923076,0.692307692307692,0.707692307692307,
0.723076923076922,0.738461538461538,0.753846153846153,0.769230769230768,
0.784615384615384,0.799999999999999,0.815384615384614,0.83076923076923,
0.846153846153845,0.86153846153846,0.876923076923076,0.892307692307691,
0.907692307692306,0.923076923076922,0.938461538461537,0.953846153846152,
0.969230769230768,0.984615384615383,1.),.UNSPECIFIED.)
CURVE()
GEOMETRIC_REPRESENTATION_ITEM()
RATIONAL_B_SPLINE_CURVE((1.,1.,1.,1.,1.,1.,1.,1.,1.,1.,1.,1.,1.,1.,1.,1.,
1.,1.,1.,1.,1.,1.,1.,1.,1.,1.,1.,1.,1.,1.,1.,1.,1.,1.,1.,1.,1.,1.,1.,1.,
1.,1.,1.,1.,1.,1.,1.,1.,1.,1.,1.,1.,1.,1.,1.,1.,1.,1.,1.,1.,1.,1.,1.,1.,
1.,1.,1.,1.,1.,1.))
REPRESENTATION_ITEM('')
);
#154=(
BOUNDED_CURVE()
B_SPLINE_CURVE(5,(#19894,#19895,#19896,#19897,#19898,#19899,#19900,#19901,
#19902,#19903,#19904,#19905,#19906,#19907,#19908,#19909,#19910,#19911,#19912,
#19913,#19914,#19915,#19916,#19917,#19918,#19919,#19920,#19921,#19922,#19923,
#19924,#19925,#19926,#19927,#19928,#19929,#19930,#19931,#19932,#19933,#19934,
#19935,#19936,#19937,#19938,#19939,#19940,#19941,#19942,#19943,#19944,#19945,
#19946,#19947,#19948,#19949,#19950,#19951,#19952,#19953,#19954,#19955,#19956,
#19957,#19958,#19959,#19960,#19961,#19962,#19963),.UNSPECIFIED.,.F.,.F.)
B_SPLINE_CURVE_WITH_KNOTS((6,1,1,1,1,1,1,1,1,1,1,1,1,1,1,1,1,1,1,1,1,1,
1,1,1,1,1,1,1,1,1,1,1,1,1,1,1,1,1,1,1,1,1,1,1,1,1,1,1,1,1,1,1,1,1,1,1,1,
1,1,1,1,1,1,1,6),(0.,0.0153846153846154,0.0307692307692308,0.0461538461538462,
0.0615384615384615,0.0769230769230769,0.0923076923076923,0.107692307692308,
0.123076923076923,0.138461538461538,0.153846153846154,0.169230769230769,
0.184615384615385,0.2,0.215384615384615,0.230769230769231,0.246153846153846,
0.261538461538462,0.276923076923077,0.292307692307692,0.307692307692308,
0.323076923076923,0.338461538461538,0.353846153846154,0.369230769230769,
0.384615384615385,0.4,0.415384615384615,0.430769230769231,0.446153846153846,
0.461538461538462,0.476923076923077,0.492307692307692,0.507692307692308,
0.523076923076923,0.538461538461538,0.553846153846154,0.569230769230769,
0.584615384615384,0.6,0.615384615384615,0.63076923076923,0.646153846153846,
0.661538461538461,0.676923076923076,0.692307692307692,0.707692307692307,
0.723076923076922,0.738461538461538,0.753846153846153,0.769230769230768,
0.784615384615384,0.799999999999999,0.815384615384614,0.83076923076923,
0.846153846153845,0.86153846153846,0.876923076923076,0.892307692307691,
0.907692307692306,0.923076923076922,0.938461538461537,0.953846153846152,
0.969230769230768,0.984615384615383,1.),.UNSPECIFIED.)
CURVE()
GEOMETRIC_REPRESENTATION_ITEM()
RATIONAL_B_SPLINE_CURVE((1.,1.,1.,1.,1.,1.,1.,1.,1.,1.,1.,1.,1.,1.,1.,1.,
1.,1.,1.,1.,1.,1.,1.,1.,1.,1.,1.,1.,1.,1.,1.,1.,1.,1.,1.,1.,1.,1.,1.,1.,
1.,1.,1.,1.,1.,1.,1.,1.,1.,1.,1.,1.,1.,1.,1.,1.,1.,1.,1.,1.,1.,1.,1.,1.,
1.,1.,1.,1.,1.,1.))
REPRESENTATION_ITEM('')
);
#155=(
BOUNDED_CURVE()
B_SPLINE_CURVE(5,(#19967,#19968,#19969,#19970,#19971,#19972,#19973,#19974,
#19975,#19976,#19977,#19978,#19979,#19980,#19981,#19982,#19983,#19984,#19985,
#19986,#19987,#19988,#19989,#19990,#19991,#19992,#19993,#19994,#19995,#19996,
#19997,#19998,#19999,#20000,#20001,#20002,#20003,#20004,#20005,#20006,#20007,
#20008,#20009,#20010,#20011,#20012,#20013,#20014,#20015,#20016,#20017,#20018,
#20019,#20020,#20021,#20022,#20023,#20024,#20025,#20026,#20027,#20028,#20029,
#20030,#20031,#20032,#20033,#20034,#20035,#20036),.UNSPECIFIED.,.F.,.F.)
B_SPLINE_CURVE_WITH_KNOTS((6,1,1,1,1,1,1,1,1,1,1,1,1,1,1,1,1,1,1,1,1,1,
1,1,1,1,1,1,1,1,1,1,1,1,1,1,1,1,1,1,1,1,1,1,1,1,1,1,1,1,1,1,1,1,1,1,1,1,
1,1,1,1,1,1,1,6),(0.,0.0153846153846154,0.0307692307692308,0.0461538461538462,
0.0615384615384615,0.0769230769230769,0.0923076923076923,0.107692307692308,
0.123076923076923,0.138461538461538,0.153846153846154,0.169230769230769,
0.184615384615385,0.2,0.215384615384615,0.230769230769231,0.246153846153846,
0.261538461538462,0.276923076923077,0.292307692307692,0.307692307692308,
0.323076923076923,0.338461538461538,0.353846153846154,0.369230769230769,
0.384615384615385,0.4,0.415384615384615,0.430769230769231,0.446153846153846,
0.461538461538462,0.476923076923077,0.492307692307692,0.507692307692308,
0.523076923076923,0.538461538461538,0.553846153846154,0.569230769230769,
0.584615384615384,0.6,0.615384615384615,0.63076923076923,0.646153846153846,
0.661538461538461,0.676923076923076,0.692307692307692,0.707692307692307,
0.723076923076922,0.738461538461538,0.753846153846153,0.769230769230768,
0.784615384615384,0.799999999999999,0.815384615384614,0.83076923076923,
0.846153846153845,0.86153846153846,0.876923076923076,0.892307692307691,
0.907692307692306,0.923076923076922,0.938461538461537,0.953846153846152,
0.969230769230768,0.984615384615383,1.),.UNSPECIFIED.)
CURVE()
GEOMETRIC_REPRESENTATION_ITEM()
RATIONAL_B_SPLINE_CURVE((1.,1.,1.,1.,1.,1.,1.,1.,1.,1.,1.,1.,1.,1.,1.,1.,
1.,1.,1.,1.,1.,1.,1.,1.,1.,1.,1.,1.,1.,1.,1.,1.,1.,1.,1.,1.,1.,1.,1.,1.,
1.,1.,1.,1.,1.,1.,1.,1.,1.,1.,1.,1.,1.,1.,1.,1.,1.,1.,1.,1.,1.,1.,1.,1.,
1.,1.,1.,1.,1.,1.))
REPRESENTATION_ITEM('')
);
#156=(
BOUNDED_CURVE()
B_SPLINE_CURVE(5,(#20040,#20041,#20042,#20043,#20044,#20045,#20046,#20047,
#20048,#20049,#20050,#20051,#20052,#20053,#20054,#20055,#20056,#20057,#20058,
#20059,#20060,#20061,#20062,#20063,#20064,#20065,#20066,#20067,#20068,#20069,
#20070,#20071,#20072,#20073,#20074,#20075,#20076,#20077,#20078,#20079,#20080,
#20081,#20082,#20083,#20084,#20085,#20086,#20087,#20088,#20089,#20090,#20091,
#20092,#20093,#20094,#20095,#20096,#20097,#20098,#20099,#20100,#20101,#20102,
#20103,#20104,#20105,#20106,#20107,#20108,#20109),.UNSPECIFIED.,.F.,.F.)
B_SPLINE_CURVE_WITH_KNOTS((6,1,1,1,1,1,1,1,1,1,1,1,1,1,1,1,1,1,1,1,1,1,
1,1,1,1,1,1,1,1,1,1,1,1,1,1,1,1,1,1,1,1,1,1,1,1,1,1,1,1,1,1,1,1,1,1,1,1,
1,1,1,1,1,1,1,6),(0.,0.0153846153846154,0.0307692307692308,0.0461538461538462,
0.0615384615384615,0.0769230769230769,0.0923076923076923,0.107692307692308,
0.123076923076923,0.138461538461538,0.153846153846154,0.169230769230769,
0.184615384615385,0.2,0.215384615384615,0.230769230769231,0.246153846153846,
0.261538461538462,0.276923076923077,0.292307692307692,0.307692307692308,
0.323076923076923,0.338461538461538,0.353846153846154,0.369230769230769,
0.384615384615385,0.4,0.415384615384615,0.430769230769231,0.446153846153846,
0.461538461538462,0.476923076923077,0.492307692307692,0.507692307692308,
0.523076923076923,0.538461538461538,0.553846153846154,0.569230769230769,
0.584615384615384,0.6,0.615384615384615,0.63076923076923,0.646153846153846,
0.661538461538461,0.676923076923076,0.692307692307692,0.707692307692307,
0.723076923076922,0.738461538461538,0.753846153846153,0.769230769230768,
0.784615384615384,0.799999999999999,0.815384615384614,0.83076923076923,
0.846153846153845,0.86153846153846,0.876923076923076,0.892307692307691,
0.907692307692306,0.923076923076922,0.938461538461537,0.953846153846152,
0.969230769230768,0.984615384615383,1.),.UNSPECIFIED.)
CURVE()
GEOMETRIC_REPRESENTATION_ITEM()
RATIONAL_B_SPLINE_CURVE((1.,1.,1.,1.,1.,1.,1.,1.,1.,1.,1.,1.,1.,1.,1.,1.,
1.,1.,1.,1.,1.,1.,1.,1.,1.,1.,1.,1.,1.,1.,1.,1.,1.,1.,1.,1.,1.,1.,1.,1.,
1.,1.,1.,1.,1.,1.,1.,1.,1.,1.,1.,1.,1.,1.,1.,1.,1.,1.,1.,1.,1.,1.,1.,1.,
1.,1.,1.,1.,1.,1.))
REPRESENTATION_ITEM('')
);
#157=(
BOUNDED_CURVE()
B_SPLINE_CURVE(5,(#20113,#20114,#20115,#20116,#20117,#20118,#20119,#20120,
#20121,#20122,#20123,#20124,#20125,#20126,#20127,#20128,#20129,#20130,#20131,
#20132,#20133,#20134,#20135,#20136,#20137,#20138,#20139,#20140,#20141,#20142,
#20143,#20144,#20145,#20146,#20147,#20148,#20149,#20150,#20151,#20152,#20153,
#20154,#20155,#20156,#20157,#20158,#20159,#20160,#20161,#20162,#20163,#20164,
#20165,#20166,#20167,#20168,#20169,#20170,#20171,#20172,#20173,#20174,#20175,
#20176,#20177,#20178,#20179,#20180,#20181,#20182),.UNSPECIFIED.,.F.,.F.)
B_SPLINE_CURVE_WITH_KNOTS((6,1,1,1,1,1,1,1,1,1,1,1,1,1,1,1,1,1,1,1,1,1,
1,1,1,1,1,1,1,1,1,1,1,1,1,1,1,1,1,1,1,1,1,1,1,1,1,1,1,1,1,1,1,1,1,1,1,1,
1,1,1,1,1,1,1,6),(0.,0.0153846153846154,0.0307692307692308,0.0461538461538462,
0.0615384615384615,0.0769230769230769,0.0923076923076923,0.107692307692308,
0.123076923076923,0.138461538461538,0.153846153846154,0.169230769230769,
0.184615384615385,0.2,0.215384615384615,0.230769230769231,0.246153846153846,
0.261538461538462,0.276923076923077,0.292307692307692,0.307692307692308,
0.323076923076923,0.338461538461538,0.353846153846154,0.369230769230769,
0.384615384615385,0.4,0.415384615384615,0.430769230769231,0.446153846153846,
0.461538461538462,0.476923076923077,0.492307692307692,0.507692307692308,
0.523076923076923,0.538461538461538,0.553846153846154,0.569230769230769,
0.584615384615384,0.6,0.615384615384615,0.63076923076923,0.646153846153846,
0.661538461538461,0.676923076923076,0.692307692307692,0.707692307692307,
0.723076923076922,0.738461538461538,0.753846153846153,0.769230769230768,
0.784615384615384,0.799999999999999,0.815384615384614,0.83076923076923,
0.846153846153845,0.86153846153846,0.876923076923076,0.892307692307691,
0.907692307692306,0.923076923076922,0.938461538461537,0.953846153846152,
0.969230769230768,0.984615384615383,1.),.UNSPECIFIED.)
CURVE()
GEOMETRIC_REPRESENTATION_ITEM()
RATIONAL_B_SPLINE_CURVE((1.,1.,1.,1.,1.,1.,1.,1.,1.,1.,1.,1.,1.,1.,1.,1.,
1.,1.,1.,1.,1.,1.,1.,1.,1.,1.,1.,1.,1.,1.,1.,1.,1.,1.,1.,1.,1.,1.,1.,1.,
1.,1.,1.,1.,1.,1.,1.,1.,1.,1.,1.,1.,1.,1.,1.,1.,1.,1.,1.,1.,1.,1.,1.,1.,
1.,1.,1.,1.,1.,1.))
REPRESENTATION_ITEM('')
);
#158=(
BOUNDED_CURVE()
B_SPLINE_CURVE(5,(#20186,#20187,#20188,#20189,#20190,#20191,#20192,#20193,
#20194,#20195,#20196,#20197,#20198,#20199,#20200,#20201,#20202,#20203,#20204,
#20205,#20206,#20207,#20208,#20209,#20210,#20211,#20212,#20213,#20214,#20215,
#20216,#20217,#20218,#20219,#20220,#20221,#20222,#20223,#20224,#20225,#20226,
#20227,#20228,#20229,#20230,#20231,#20232,#20233,#20234,#20235,#20236,#20237,
#20238,#20239,#20240,#20241,#20242,#20243,#20244,#20245,#20246,#20247,#20248,
#20249,#20250,#20251,#20252,#20253,#20254,#20255),.UNSPECIFIED.,.F.,.F.)
B_SPLINE_CURVE_WITH_KNOTS((6,1,1,1,1,1,1,1,1,1,1,1,1,1,1,1,1,1,1,1,1,1,
1,1,1,1,1,1,1,1,1,1,1,1,1,1,1,1,1,1,1,1,1,1,1,1,1,1,1,1,1,1,1,1,1,1,1,1,
1,1,1,1,1,1,1,6),(0.,0.0153846153846154,0.0307692307692308,0.0461538461538462,
0.0615384615384615,0.0769230769230769,0.0923076923076923,0.107692307692308,
0.123076923076923,0.138461538461538,0.153846153846154,0.169230769230769,
0.184615384615385,0.2,0.215384615384615,0.230769230769231,0.246153846153846,
0.261538461538462,0.276923076923077,0.292307692307692,0.307692307692308,
0.323076923076923,0.338461538461538,0.353846153846154,0.369230769230769,
0.384615384615385,0.4,0.415384615384615,0.430769230769231,0.446153846153846,
0.461538461538462,0.476923076923077,0.492307692307692,0.507692307692308,
0.523076923076923,0.538461538461538,0.553846153846154,0.569230769230769,
0.584615384615384,0.6,0.615384615384615,0.63076923076923,0.646153846153846,
0.661538461538461,0.676923076923076,0.692307692307692,0.707692307692307,
0.723076923076922,0.738461538461538,0.753846153846153,0.769230769230768,
0.784615384615384,0.799999999999999,0.815384615384614,0.83076923076923,
0.846153846153845,0.86153846153846,0.876923076923076,0.892307692307691,
0.907692307692306,0.923076923076922,0.938461538461537,0.953846153846152,
0.969230769230768,0.984615384615383,1.),.UNSPECIFIED.)
CURVE()
GEOMETRIC_REPRESENTATION_ITEM()
RATIONAL_B_SPLINE_CURVE((1.,1.,1.,1.,1.,1.,1.,1.,1.,1.,1.,1.,1.,1.,1.,1.,
1.,1.,1.,1.,1.,1.,1.,1.,1.,1.,1.,1.,1.,1.,1.,1.,1.,1.,1.,1.,1.,1.,1.,1.,
1.,1.,1.,1.,1.,1.,1.,1.,1.,1.,1.,1.,1.,1.,1.,1.,1.,1.,1.,1.,1.,1.,1.,1.,
1.,1.,1.,1.,1.,1.))
REPRESENTATION_ITEM('')
);
#159=(
BOUNDED_CURVE()
B_SPLINE_CURVE(5,(#20259,#20260,#20261,#20262,#20263,#20264,#20265,#20266,
#20267,#20268,#20269,#20270,#20271,#20272,#20273,#20274,#20275,#20276,#20277,
#20278,#20279,#20280,#20281,#20282,#20283,#20284,#20285,#20286,#20287,#20288,
#20289,#20290,#20291,#20292,#20293,#20294,#20295,#20296,#20297,#20298,#20299,
#20300,#20301,#20302,#20303,#20304,#20305,#20306,#20307,#20308,#20309,#20310,
#20311,#20312,#20313,#20314,#20315,#20316,#20317,#20318,#20319,#20320,#20321,
#20322,#20323,#20324,#20325,#20326,#20327,#20328),.UNSPECIFIED.,.F.,.F.)
B_SPLINE_CURVE_WITH_KNOTS((6,1,1,1,1,1,1,1,1,1,1,1,1,1,1,1,1,1,1,1,1,1,
1,1,1,1,1,1,1,1,1,1,1,1,1,1,1,1,1,1,1,1,1,1,1,1,1,1,1,1,1,1,1,1,1,1,1,1,
1,1,1,1,1,1,1,6),(0.,0.0153846153846154,0.0307692307692308,0.0461538461538462,
0.0615384615384615,0.0769230769230769,0.0923076923076923,0.107692307692308,
0.123076923076923,0.138461538461538,0.153846153846154,0.169230769230769,
0.184615384615385,0.2,0.215384615384615,0.230769230769231,0.246153846153846,
0.261538461538462,0.276923076923077,0.292307692307692,0.307692307692308,
0.323076923076923,0.338461538461538,0.353846153846154,0.369230769230769,
0.384615384615385,0.4,0.415384615384615,0.430769230769231,0.446153846153846,
0.461538461538462,0.476923076923077,0.492307692307692,0.507692307692308,
0.523076923076923,0.538461538461538,0.553846153846154,0.569230769230769,
0.584615384615384,0.6,0.615384615384615,0.63076923076923,0.646153846153846,
0.661538461538461,0.676923076923076,0.692307692307692,0.707692307692307,
0.723076923076922,0.738461538461538,0.753846153846153,0.769230769230768,
0.784615384615384,0.799999999999999,0.815384615384614,0.83076923076923,
0.846153846153845,0.86153846153846,0.876923076923076,0.892307692307691,
0.907692307692306,0.923076923076922,0.938461538461537,0.953846153846152,
0.969230769230768,0.984615384615383,1.),.UNSPECIFIED.)
CURVE()
GEOMETRIC_REPRESENTATION_ITEM()
RATIONAL_B_SPLINE_CURVE((1.,1.,1.,1.,1.,1.,1.,1.,1.,1.,1.,1.,1.,1.,1.,1.,
1.,1.,1.,1.,1.,1.,1.,1.,1.,1.,1.,1.,1.,1.,1.,1.,1.,1.,1.,1.,1.,1.,1.,1.,
1.,1.,1.,1.,1.,1.,1.,1.,1.,1.,1.,1.,1.,1.,1.,1.,1.,1.,1.,1.,1.,1.,1.,1.,
1.,1.,1.,1.,1.,1.))
REPRESENTATION_ITEM('')
);
#160=(
BOUNDED_CURVE()
B_SPLINE_CURVE(5,(#20332,#20333,#20334,#20335,#20336,#20337,#20338,#20339,
#20340,#20341,#20342,#20343,#20344,#20345,#20346,#20347,#20348,#20349,#20350,
#20351,#20352,#20353,#20354,#20355,#20356,#20357,#20358,#20359,#20360,#20361,
#20362,#20363,#20364,#20365,#20366,#20367,#20368,#20369,#20370,#20371,#20372,
#20373,#20374,#20375,#20376,#20377,#20378,#20379,#20380,#20381,#20382,#20383,
#20384,#20385,#20386,#20387,#20388,#20389,#20390,#20391,#20392,#20393,#20394,
#20395,#20396,#20397,#20398,#20399,#20400,#20401),.UNSPECIFIED.,.F.,.F.)
B_SPLINE_CURVE_WITH_KNOTS((6,1,1,1,1,1,1,1,1,1,1,1,1,1,1,1,1,1,1,1,1,1,
1,1,1,1,1,1,1,1,1,1,1,1,1,1,1,1,1,1,1,1,1,1,1,1,1,1,1,1,1,1,1,1,1,1,1,1,
1,1,1,1,1,1,1,6),(0.,0.0153846153846154,0.0307692307692308,0.0461538461538462,
0.0615384615384615,0.0769230769230769,0.0923076923076923,0.107692307692308,
0.123076923076923,0.138461538461538,0.153846153846154,0.169230769230769,
0.184615384615385,0.2,0.215384615384615,0.230769230769231,0.246153846153846,
0.261538461538462,0.276923076923077,0.292307692307692,0.307692307692308,
0.323076923076923,0.338461538461538,0.353846153846154,0.369230769230769,
0.384615384615385,0.4,0.415384615384615,0.430769230769231,0.446153846153846,
0.461538461538462,0.476923076923077,0.492307692307692,0.507692307692308,
0.523076923076923,0.538461538461538,0.553846153846154,0.569230769230769,
0.584615384615384,0.6,0.615384615384615,0.63076923076923,0.646153846153846,
0.661538461538461,0.676923076923076,0.692307692307692,0.707692307692307,
0.723076923076922,0.738461538461538,0.753846153846153,0.769230769230768,
0.784615384615384,0.799999999999999,0.815384615384614,0.83076923076923,
0.846153846153845,0.86153846153846,0.876923076923076,0.892307692307691,
0.907692307692306,0.923076923076922,0.938461538461537,0.953846153846152,
0.969230769230768,0.984615384615383,1.),.UNSPECIFIED.)
CURVE()
GEOMETRIC_REPRESENTATION_ITEM()
RATIONAL_B_SPLINE_CURVE((1.,1.,1.,1.,1.,1.,1.,1.,1.,1.,1.,1.,1.,1.,1.,1.,
1.,1.,1.,1.,1.,1.,1.,1.,1.,1.,1.,1.,1.,1.,1.,1.,1.,1.,1.,1.,1.,1.,1.,1.,
1.,1.,1.,1.,1.,1.,1.,1.,1.,1.,1.,1.,1.,1.,1.,1.,1.,1.,1.,1.,1.,1.,1.,1.,
1.,1.,1.,1.,1.,1.))
REPRESENTATION_ITEM('')
);
#161=(
BOUNDED_CURVE()
B_SPLINE_CURVE(5,(#20405,#20406,#20407,#20408,#20409,#20410,#20411,#20412,
#20413,#20414,#20415,#20416,#20417,#20418,#20419,#20420,#20421,#20422,#20423,
#20424,#20425,#20426,#20427,#20428,#20429,#20430,#20431,#20432,#20433,#20434,
#20435,#20436,#20437,#20438,#20439,#20440,#20441,#20442,#20443,#20444,#20445,
#20446,#20447,#20448,#20449,#20450,#20451,#20452,#20453,#20454,#20455,#20456,
#20457,#20458,#20459,#20460,#20461,#20462,#20463,#20464,#20465,#20466,#20467,
#20468,#20469,#20470,#20471,#20472,#20473,#20474),.UNSPECIFIED.,.F.,.F.)
B_SPLINE_CURVE_WITH_KNOTS((6,1,1,1,1,1,1,1,1,1,1,1,1,1,1,1,1,1,1,1,1,1,
1,1,1,1,1,1,1,1,1,1,1,1,1,1,1,1,1,1,1,1,1,1,1,1,1,1,1,1,1,1,1,1,1,1,1,1,
1,1,1,1,1,1,1,6),(0.,0.0153846153846154,0.0307692307692308,0.0461538461538462,
0.0615384615384615,0.0769230769230769,0.0923076923076923,0.107692307692308,
0.123076923076923,0.138461538461538,0.153846153846154,0.169230769230769,
0.184615384615385,0.2,0.215384615384615,0.230769230769231,0.246153846153846,
0.261538461538462,0.276923076923077,0.292307692307692,0.307692307692308,
0.323076923076923,0.338461538461538,0.353846153846154,0.369230769230769,
0.384615384615385,0.4,0.415384615384615,0.430769230769231,0.446153846153846,
0.461538461538462,0.476923076923077,0.492307692307692,0.507692307692308,
0.523076923076923,0.538461538461538,0.553846153846154,0.569230769230769,
0.584615384615384,0.6,0.615384615384615,0.63076923076923,0.646153846153846,
0.661538461538461,0.676923076923076,0.692307692307692,0.707692307692307,
0.723076923076922,0.738461538461538,0.753846153846153,0.769230769230768,
0.784615384615384,0.799999999999999,0.815384615384614,0.83076923076923,
0.846153846153845,0.86153846153846,0.876923076923076,0.892307692307691,
0.907692307692306,0.923076923076922,0.938461538461537,0.953846153846152,
0.969230769230768,0.984615384615383,1.),.UNSPECIFIED.)
CURVE()
GEOMETRIC_REPRESENTATION_ITEM()
RATIONAL_B_SPLINE_CURVE((1.,1.,1.,1.,1.,1.,1.,1.,1.,1.,1.,1.,1.,1.,1.,1.,
1.,1.,1.,1.,1.,1.,1.,1.,1.,1.,1.,1.,1.,1.,1.,1.,1.,1.,1.,1.,1.,1.,1.,1.,
1.,1.,1.,1.,1.,1.,1.,1.,1.,1.,1.,1.,1.,1.,1.,1.,1.,1.,1.,1.,1.,1.,1.,1.,
1.,1.,1.,1.,1.,1.))
REPRESENTATION_ITEM('')
);
#162=(
BOUNDED_CURVE()
B_SPLINE_CURVE(5,(#20478,#20479,#20480,#20481,#20482,#20483,#20484,#20485,
#20486,#20487,#20488,#20489,#20490,#20491,#20492,#20493,#20494,#20495,#20496,
#20497,#20498,#20499,#20500,#20501,#20502,#20503,#20504,#20505,#20506,#20507,
#20508,#20509,#20510,#20511,#20512,#20513,#20514,#20515,#20516,#20517,#20518,
#20519,#20520,#20521,#20522,#20523,#20524,#20525,#20526,#20527,#20528,#20529,
#20530,#20531,#20532,#20533,#20534,#20535,#20536,#20537,#20538,#20539,#20540,
#20541,#20542,#20543,#20544,#20545,#20546,#20547),.UNSPECIFIED.,.F.,.F.)
B_SPLINE_CURVE_WITH_KNOTS((6,1,1,1,1,1,1,1,1,1,1,1,1,1,1,1,1,1,1,1,1,1,
1,1,1,1,1,1,1,1,1,1,1,1,1,1,1,1,1,1,1,1,1,1,1,1,1,1,1,1,1,1,1,1,1,1,1,1,
1,1,1,1,1,1,1,6),(0.,0.0153846153846154,0.0307692307692308,0.0461538461538462,
0.0615384615384615,0.0769230769230769,0.0923076923076923,0.107692307692308,
0.123076923076923,0.138461538461538,0.153846153846154,0.169230769230769,
0.184615384615385,0.2,0.215384615384615,0.230769230769231,0.246153846153846,
0.261538461538462,0.276923076923077,0.292307692307692,0.307692307692308,
0.323076923076923,0.338461538461538,0.353846153846154,0.369230769230769,
0.384615384615385,0.4,0.415384615384615,0.430769230769231,0.446153846153846,
0.461538461538462,0.476923076923077,0.492307692307692,0.507692307692308,
0.523076923076923,0.538461538461538,0.553846153846154,0.569230769230769,
0.584615384615384,0.6,0.615384615384615,0.63076923076923,0.646153846153846,
0.661538461538461,0.676923076923076,0.692307692307692,0.707692307692307,
0.723076923076922,0.738461538461538,0.753846153846153,0.769230769230768,
0.784615384615384,0.799999999999999,0.815384615384614,0.83076923076923,
0.846153846153845,0.86153846153846,0.876923076923076,0.892307692307691,
0.907692307692306,0.923076923076922,0.938461538461537,0.953846153846152,
0.969230769230768,0.984615384615383,1.),.UNSPECIFIED.)
CURVE()
GEOMETRIC_REPRESENTATION_ITEM()
RATIONAL_B_SPLINE_CURVE((1.,1.,1.,1.,1.,1.,1.,1.,1.,1.,1.,1.,1.,1.,1.,1.,
1.,1.,1.,1.,1.,1.,1.,1.,1.,1.,1.,1.,1.,1.,1.,1.,1.,1.,1.,1.,1.,1.,1.,1.,
1.,1.,1.,1.,1.,1.,1.,1.,1.,1.,1.,1.,1.,1.,1.,1.,1.,1.,1.,1.,1.,1.,1.,1.,
1.,1.,1.,1.,1.,1.))
REPRESENTATION_ITEM('')
);
#163=(
BOUNDED_CURVE()
B_SPLINE_CURVE(5,(#20551,#20552,#20553,#20554,#20555,#20556,#20557,#20558,
#20559,#20560,#20561,#20562,#20563,#20564,#20565,#20566,#20567,#20568,#20569,
#20570,#20571,#20572,#20573,#20574,#20575,#20576,#20577,#20578,#20579,#20580,
#20581,#20582,#20583,#20584,#20585,#20586,#20587,#20588,#20589,#20590,#20591,
#20592,#20593,#20594,#20595,#20596,#20597,#20598,#20599,#20600,#20601,#20602,
#20603,#20604,#20605,#20606,#20607,#20608,#20609,#20610,#20611,#20612,#20613,
#20614,#20615,#20616,#20617,#20618,#20619,#20620),.UNSPECIFIED.,.F.,.F.)
B_SPLINE_CURVE_WITH_KNOTS((6,1,1,1,1,1,1,1,1,1,1,1,1,1,1,1,1,1,1,1,1,1,
1,1,1,1,1,1,1,1,1,1,1,1,1,1,1,1,1,1,1,1,1,1,1,1,1,1,1,1,1,1,1,1,1,1,1,1,
1,1,1,1,1,1,1,6),(0.,0.0153846153846154,0.0307692307692308,0.0461538461538462,
0.0615384615384615,0.0769230769230769,0.0923076923076923,0.107692307692308,
0.123076923076923,0.138461538461538,0.153846153846154,0.169230769230769,
0.184615384615385,0.2,0.215384615384615,0.230769230769231,0.246153846153846,
0.261538461538462,0.276923076923077,0.292307692307692,0.307692307692308,
0.323076923076923,0.338461538461538,0.353846153846154,0.369230769230769,
0.384615384615385,0.4,0.415384615384615,0.430769230769231,0.446153846153846,
0.461538461538462,0.476923076923077,0.492307692307692,0.507692307692308,
0.523076923076923,0.538461538461538,0.553846153846154,0.569230769230769,
0.584615384615384,0.6,0.615384615384615,0.63076923076923,0.646153846153846,
0.661538461538461,0.676923076923076,0.692307692307692,0.707692307692307,
0.723076923076922,0.738461538461538,0.753846153846153,0.769230769230768,
0.784615384615384,0.799999999999999,0.815384615384614,0.83076923076923,
0.846153846153845,0.86153846153846,0.876923076923076,0.892307692307691,
0.907692307692306,0.923076923076922,0.938461538461537,0.953846153846152,
0.969230769230768,0.984615384615383,1.),.UNSPECIFIED.)
CURVE()
GEOMETRIC_REPRESENTATION_ITEM()
RATIONAL_B_SPLINE_CURVE((1.,1.,1.,1.,1.,1.,1.,1.,1.,1.,1.,1.,1.,1.,1.,1.,
1.,1.,1.,1.,1.,1.,1.,1.,1.,1.,1.,1.,1.,1.,1.,1.,1.,1.,1.,1.,1.,1.,1.,1.,
1.,1.,1.,1.,1.,1.,1.,1.,1.,1.,1.,1.,1.,1.,1.,1.,1.,1.,1.,1.,1.,1.,1.,1.,
1.,1.,1.,1.,1.,1.))
REPRESENTATION_ITEM('')
);
#164=(
BOUNDED_CURVE()
B_SPLINE_CURVE(5,(#20624,#20625,#20626,#20627,#20628,#20629,#20630,#20631,
#20632,#20633,#20634,#20635,#20636,#20637,#20638,#20639,#20640,#20641,#20642,
#20643,#20644,#20645,#20646,#20647,#20648,#20649,#20650,#20651,#20652,#20653,
#20654,#20655,#20656,#20657,#20658,#20659,#20660,#20661,#20662,#20663,#20664,
#20665,#20666,#20667,#20668,#20669,#20670,#20671,#20672,#20673,#20674,#20675,
#20676,#20677,#20678,#20679,#20680,#20681,#20682,#20683,#20684,#20685,#20686,
#20687,#20688,#20689,#20690,#20691,#20692,#20693),.UNSPECIFIED.,.F.,.F.)
B_SPLINE_CURVE_WITH_KNOTS((6,1,1,1,1,1,1,1,1,1,1,1,1,1,1,1,1,1,1,1,1,1,
1,1,1,1,1,1,1,1,1,1,1,1,1,1,1,1,1,1,1,1,1,1,1,1,1,1,1,1,1,1,1,1,1,1,1,1,
1,1,1,1,1,1,1,6),(0.,0.0153846153846154,0.0307692307692308,0.0461538461538462,
0.0615384615384615,0.0769230769230769,0.0923076923076923,0.107692307692308,
0.123076923076923,0.138461538461538,0.153846153846154,0.169230769230769,
0.184615384615385,0.2,0.215384615384615,0.230769230769231,0.246153846153846,
0.261538461538462,0.276923076923077,0.292307692307692,0.307692307692308,
0.323076923076923,0.338461538461538,0.353846153846154,0.369230769230769,
0.384615384615385,0.4,0.415384615384615,0.430769230769231,0.446153846153846,
0.461538461538462,0.476923076923077,0.492307692307692,0.507692307692308,
0.523076923076923,0.538461538461538,0.553846153846154,0.569230769230769,
0.584615384615384,0.6,0.615384615384615,0.63076923076923,0.646153846153846,
0.661538461538461,0.676923076923076,0.692307692307692,0.707692307692307,
0.723076923076922,0.738461538461538,0.753846153846153,0.769230769230768,
0.784615384615384,0.799999999999999,0.815384615384614,0.83076923076923,
0.846153846153845,0.86153846153846,0.876923076923076,0.892307692307691,
0.907692307692306,0.923076923076922,0.938461538461537,0.953846153846152,
0.969230769230768,0.984615384615383,1.),.UNSPECIFIED.)
CURVE()
GEOMETRIC_REPRESENTATION_ITEM()
RATIONAL_B_SPLINE_CURVE((1.,1.,1.,1.,1.,1.,1.,1.,1.,1.,1.,1.,1.,1.,1.,1.,
1.,1.,1.,1.,1.,1.,1.,1.,1.,1.,1.,1.,1.,1.,1.,1.,1.,1.,1.,1.,1.,1.,1.,1.,
1.,1.,1.,1.,1.,1.,1.,1.,1.,1.,1.,1.,1.,1.,1.,1.,1.,1.,1.,1.,1.,1.,1.,1.,
1.,1.,1.,1.,1.,1.))
REPRESENTATION_ITEM('')
);
#165=(
BOUNDED_CURVE()
B_SPLINE_CURVE(5,(#20697,#20698,#20699,#20700,#20701,#20702,#20703,#20704,
#20705,#20706,#20707,#20708,#20709,#20710,#20711,#20712,#20713,#20714,#20715,
#20716,#20717,#20718,#20719,#20720,#20721,#20722,#20723,#20724,#20725,#20726,
#20727,#20728,#20729,#20730,#20731,#20732,#20733,#20734,#20735,#20736,#20737,
#20738,#20739,#20740,#20741,#20742,#20743,#20744,#20745,#20746,#20747,#20748,
#20749,#20750,#20751,#20752,#20753,#20754,#20755,#20756,#20757,#20758,#20759,
#20760,#20761,#20762,#20763,#20764,#20765,#20766),.UNSPECIFIED.,.F.,.F.)
B_SPLINE_CURVE_WITH_KNOTS((6,1,1,1,1,1,1,1,1,1,1,1,1,1,1,1,1,1,1,1,1,1,
1,1,1,1,1,1,1,1,1,1,1,1,1,1,1,1,1,1,1,1,1,1,1,1,1,1,1,1,1,1,1,1,1,1,1,1,
1,1,1,1,1,1,1,6),(0.,0.0153846153846154,0.0307692307692308,0.0461538461538462,
0.0615384615384615,0.0769230769230769,0.0923076923076923,0.107692307692308,
0.123076923076923,0.138461538461538,0.153846153846154,0.169230769230769,
0.184615384615385,0.2,0.215384615384615,0.230769230769231,0.246153846153846,
0.261538461538462,0.276923076923077,0.292307692307692,0.307692307692308,
0.323076923076923,0.338461538461538,0.353846153846154,0.369230769230769,
0.384615384615385,0.4,0.415384615384615,0.430769230769231,0.446153846153846,
0.461538461538462,0.476923076923077,0.492307692307692,0.507692307692308,
0.523076923076923,0.538461538461538,0.553846153846154,0.569230769230769,
0.584615384615384,0.6,0.615384615384615,0.63076923076923,0.646153846153846,
0.661538461538461,0.676923076923076,0.692307692307692,0.707692307692307,
0.723076923076922,0.738461538461538,0.753846153846153,0.769230769230768,
0.784615384615384,0.799999999999999,0.815384615384614,0.83076923076923,
0.846153846153845,0.86153846153846,0.876923076923076,0.892307692307691,
0.907692307692306,0.923076923076922,0.938461538461537,0.953846153846152,
0.969230769230768,0.984615384615383,1.),.UNSPECIFIED.)
CURVE()
GEOMETRIC_REPRESENTATION_ITEM()
RATIONAL_B_SPLINE_CURVE((1.,1.,1.,1.,1.,1.,1.,1.,1.,1.,1.,1.,1.,1.,1.,1.,
1.,1.,1.,1.,1.,1.,1.,1.,1.,1.,1.,1.,1.,1.,1.,1.,1.,1.,1.,1.,1.,1.,1.,1.,
1.,1.,1.,1.,1.,1.,1.,1.,1.,1.,1.,1.,1.,1.,1.,1.,1.,1.,1.,1.,1.,1.,1.,1.,
1.,1.,1.,1.,1.,1.))
REPRESENTATION_ITEM('')
);
#166=(
BOUNDED_CURVE()
B_SPLINE_CURVE(5,(#20770,#20771,#20772,#20773,#20774,#20775,#20776,#20777,
#20778,#20779,#20780,#20781,#20782,#20783,#20784,#20785,#20786,#20787,#20788,
#20789,#20790,#20791,#20792,#20793,#20794,#20795,#20796,#20797,#20798,#20799,
#20800,#20801,#20802,#20803,#20804,#20805,#20806,#20807,#20808,#20809,#20810,
#20811,#20812,#20813,#20814,#20815,#20816,#20817,#20818,#20819,#20820,#20821,
#20822,#20823,#20824,#20825,#20826,#20827,#20828,#20829,#20830,#20831,#20832,
#20833,#20834,#20835,#20836,#20837,#20838,#20839),.UNSPECIFIED.,.F.,.F.)
B_SPLINE_CURVE_WITH_KNOTS((6,1,1,1,1,1,1,1,1,1,1,1,1,1,1,1,1,1,1,1,1,1,
1,1,1,1,1,1,1,1,1,1,1,1,1,1,1,1,1,1,1,1,1,1,1,1,1,1,1,1,1,1,1,1,1,1,1,1,
1,1,1,1,1,1,1,6),(0.,0.0153846153846154,0.0307692307692308,0.0461538461538462,
0.0615384615384615,0.0769230769230769,0.0923076923076923,0.107692307692308,
0.123076923076923,0.138461538461538,0.153846153846154,0.169230769230769,
0.184615384615385,0.2,0.215384615384615,0.230769230769231,0.246153846153846,
0.261538461538462,0.276923076923077,0.292307692307692,0.307692307692308,
0.323076923076923,0.338461538461538,0.353846153846154,0.369230769230769,
0.384615384615385,0.4,0.415384615384615,0.430769230769231,0.446153846153846,
0.461538461538462,0.476923076923077,0.492307692307692,0.507692307692308,
0.523076923076923,0.538461538461538,0.553846153846154,0.569230769230769,
0.584615384615384,0.6,0.615384615384615,0.63076923076923,0.646153846153846,
0.661538461538461,0.676923076923076,0.692307692307692,0.707692307692307,
0.723076923076922,0.738461538461538,0.753846153846153,0.769230769230768,
0.784615384615384,0.799999999999999,0.815384615384614,0.83076923076923,
0.846153846153845,0.86153846153846,0.876923076923076,0.892307692307691,
0.907692307692306,0.923076923076922,0.938461538461537,0.953846153846152,
0.969230769230768,0.984615384615383,1.),.UNSPECIFIED.)
CURVE()
GEOMETRIC_REPRESENTATION_ITEM()
RATIONAL_B_SPLINE_CURVE((1.,1.,1.,1.,1.,1.,1.,1.,1.,1.,1.,1.,1.,1.,1.,1.,
1.,1.,1.,1.,1.,1.,1.,1.,1.,1.,1.,1.,1.,1.,1.,1.,1.,1.,1.,1.,1.,1.,1.,1.,
1.,1.,1.,1.,1.,1.,1.,1.,1.,1.,1.,1.,1.,1.,1.,1.,1.,1.,1.,1.,1.,1.,1.,1.,
1.,1.,1.,1.,1.,1.))
REPRESENTATION_ITEM('')
);
#167=(
BOUNDED_CURVE()
B_SPLINE_CURVE(5,(#20843,#20844,#20845,#20846,#20847,#20848,#20849,#20850,
#20851,#20852,#20853,#20854,#20855,#20856,#20857,#20858,#20859,#20860,#20861,
#20862,#20863,#20864,#20865,#20866,#20867,#20868,#20869,#20870,#20871,#20872,
#20873,#20874,#20875,#20876,#20877,#20878,#20879,#20880,#20881,#20882,#20883,
#20884,#20885,#20886,#20887,#20888,#20889,#20890,#20891,#20892,#20893,#20894,
#20895,#20896,#20897,#20898,#20899,#20900,#20901,#20902,#20903,#20904,#20905,
#20906,#20907,#20908,#20909,#20910,#20911,#20912),.UNSPECIFIED.,.F.,.F.)
B_SPLINE_CURVE_WITH_KNOTS((6,1,1,1,1,1,1,1,1,1,1,1,1,1,1,1,1,1,1,1,1,1,
1,1,1,1,1,1,1,1,1,1,1,1,1,1,1,1,1,1,1,1,1,1,1,1,1,1,1,1,1,1,1,1,1,1,1,1,
1,1,1,1,1,1,1,6),(0.,0.0153846153846154,0.0307692307692308,0.0461538461538462,
0.0615384615384615,0.0769230769230769,0.0923076923076923,0.107692307692308,
0.123076923076923,0.138461538461538,0.153846153846154,0.169230769230769,
0.184615384615385,0.2,0.215384615384615,0.230769230769231,0.246153846153846,
0.261538461538462,0.276923076923077,0.292307692307692,0.307692307692308,
0.323076923076923,0.338461538461538,0.353846153846154,0.369230769230769,
0.384615384615385,0.4,0.415384615384615,0.430769230769231,0.446153846153846,
0.461538461538462,0.476923076923077,0.492307692307692,0.507692307692308,
0.523076923076923,0.538461538461538,0.553846153846154,0.569230769230769,
0.584615384615384,0.6,0.615384615384615,0.63076923076923,0.646153846153846,
0.661538461538461,0.676923076923076,0.692307692307692,0.707692307692307,
0.723076923076922,0.738461538461538,0.753846153846153,0.769230769230768,
0.784615384615384,0.799999999999999,0.815384615384614,0.83076923076923,
0.846153846153845,0.86153846153846,0.876923076923076,0.892307692307691,
0.907692307692306,0.923076923076922,0.938461538461537,0.953846153846152,
0.969230769230768,0.984615384615383,1.),.UNSPECIFIED.)
CURVE()
GEOMETRIC_REPRESENTATION_ITEM()
RATIONAL_B_SPLINE_CURVE((1.,1.,1.,1.,1.,1.,1.,1.,1.,1.,1.,1.,1.,1.,1.,1.,
1.,1.,1.,1.,1.,1.,1.,1.,1.,1.,1.,1.,1.,1.,1.,1.,1.,1.,1.,1.,1.,1.,1.,1.,
1.,1.,1.,1.,1.,1.,1.,1.,1.,1.,1.,1.,1.,1.,1.,1.,1.,1.,1.,1.,1.,1.,1.,1.,
1.,1.,1.,1.,1.,1.))
REPRESENTATION_ITEM('')
);
#168=(
BOUNDED_CURVE()
B_SPLINE_CURVE(5,(#20916,#20917,#20918,#20919,#20920,#20921,#20922,#20923,
#20924,#20925,#20926,#20927,#20928,#20929,#20930,#20931,#20932,#20933,#20934,
#20935,#20936,#20937,#20938,#20939,#20940,#20941,#20942,#20943,#20944,#20945,
#20946,#20947,#20948,#20949,#20950,#20951,#20952,#20953,#20954,#20955,#20956,
#20957,#20958,#20959,#20960,#20961,#20962,#20963,#20964,#20965,#20966,#20967,
#20968,#20969,#20970,#20971,#20972,#20973,#20974,#20975,#20976,#20977,#20978,
#20979,#20980,#20981,#20982,#20983,#20984,#20985),.UNSPECIFIED.,.F.,.F.)
B_SPLINE_CURVE_WITH_KNOTS((6,1,1,1,1,1,1,1,1,1,1,1,1,1,1,1,1,1,1,1,1,1,
1,1,1,1,1,1,1,1,1,1,1,1,1,1,1,1,1,1,1,1,1,1,1,1,1,1,1,1,1,1,1,1,1,1,1,1,
1,1,1,1,1,1,1,6),(0.,0.0153846153846154,0.0307692307692308,0.0461538461538462,
0.0615384615384615,0.0769230769230769,0.0923076923076923,0.107692307692308,
0.123076923076923,0.138461538461538,0.153846153846154,0.169230769230769,
0.184615384615385,0.2,0.215384615384615,0.230769230769231,0.246153846153846,
0.261538461538462,0.276923076923077,0.292307692307692,0.307692307692308,
0.323076923076923,0.338461538461538,0.353846153846154,0.369230769230769,
0.384615384615385,0.4,0.415384615384615,0.430769230769231,0.446153846153846,
0.461538461538462,0.476923076923077,0.492307692307692,0.507692307692308,
0.523076923076923,0.538461538461538,0.553846153846154,0.569230769230769,
0.584615384615384,0.6,0.615384615384615,0.63076923076923,0.646153846153846,
0.661538461538461,0.676923076923076,0.692307692307692,0.707692307692307,
0.723076923076922,0.738461538461538,0.753846153846153,0.769230769230768,
0.784615384615384,0.799999999999999,0.815384615384614,0.83076923076923,
0.846153846153845,0.86153846153846,0.876923076923076,0.892307692307691,
0.907692307692306,0.923076923076922,0.938461538461537,0.953846153846152,
0.969230769230768,0.984615384615383,1.),.UNSPECIFIED.)
CURVE()
GEOMETRIC_REPRESENTATION_ITEM()
RATIONAL_B_SPLINE_CURVE((1.,1.,1.,1.,1.,1.,1.,1.,1.,1.,1.,1.,1.,1.,1.,1.,
1.,1.,1.,1.,1.,1.,1.,1.,1.,1.,1.,1.,1.,1.,1.,1.,1.,1.,1.,1.,1.,1.,1.,1.,
1.,1.,1.,1.,1.,1.,1.,1.,1.,1.,1.,1.,1.,1.,1.,1.,1.,1.,1.,1.,1.,1.,1.,1.,
1.,1.,1.,1.,1.,1.))
REPRESENTATION_ITEM('')
);
#169=(
BOUNDED_CURVE()
B_SPLINE_CURVE(5,(#20989,#20990,#20991,#20992,#20993,#20994,#20995,#20996,
#20997,#20998,#20999,#21000,#21001,#21002,#21003,#21004,#21005,#21006,#21007,
#21008,#21009,#21010,#21011,#21012,#21013,#21014,#21015,#21016,#21017,#21018,
#21019,#21020,#21021,#21022,#21023,#21024,#21025,#21026,#21027,#21028,#21029,
#21030,#21031,#21032,#21033,#21034,#21035,#21036,#21037,#21038,#21039,#21040,
#21041,#21042,#21043,#21044,#21045,#21046,#21047,#21048,#21049,#21050,#21051,
#21052,#21053,#21054,#21055,#21056,#21057,#21058),.UNSPECIFIED.,.F.,.F.)
B_SPLINE_CURVE_WITH_KNOTS((6,1,1,1,1,1,1,1,1,1,1,1,1,1,1,1,1,1,1,1,1,1,
1,1,1,1,1,1,1,1,1,1,1,1,1,1,1,1,1,1,1,1,1,1,1,1,1,1,1,1,1,1,1,1,1,1,1,1,
1,1,1,1,1,1,1,6),(0.,0.0153846153846154,0.0307692307692308,0.0461538461538462,
0.0615384615384615,0.0769230769230769,0.0923076923076923,0.107692307692308,
0.123076923076923,0.138461538461538,0.153846153846154,0.169230769230769,
0.184615384615385,0.2,0.215384615384615,0.230769230769231,0.246153846153846,
0.261538461538462,0.276923076923077,0.292307692307692,0.307692307692308,
0.323076923076923,0.338461538461538,0.353846153846154,0.369230769230769,
0.384615384615385,0.4,0.415384615384615,0.430769230769231,0.446153846153846,
0.461538461538462,0.476923076923077,0.492307692307692,0.507692307692308,
0.523076923076923,0.538461538461538,0.553846153846154,0.569230769230769,
0.584615384615384,0.6,0.615384615384615,0.63076923076923,0.646153846153846,
0.661538461538461,0.676923076923076,0.692307692307692,0.707692307692307,
0.723076923076922,0.738461538461538,0.753846153846153,0.769230769230768,
0.784615384615384,0.799999999999999,0.815384615384614,0.83076923076923,
0.846153846153845,0.86153846153846,0.876923076923076,0.892307692307691,
0.907692307692306,0.923076923076922,0.938461538461537,0.953846153846152,
0.969230769230768,0.984615384615383,1.),.UNSPECIFIED.)
CURVE()
GEOMETRIC_REPRESENTATION_ITEM()
RATIONAL_B_SPLINE_CURVE((1.,1.,1.,1.,1.,1.,1.,1.,1.,1.,1.,1.,1.,1.,1.,1.,
1.,1.,1.,1.,1.,1.,1.,1.,1.,1.,1.,1.,1.,1.,1.,1.,1.,1.,1.,1.,1.,1.,1.,1.,
1.,1.,1.,1.,1.,1.,1.,1.,1.,1.,1.,1.,1.,1.,1.,1.,1.,1.,1.,1.,1.,1.,1.,1.,
1.,1.,1.,1.,1.,1.))
REPRESENTATION_ITEM('')
);
#170=(
BOUNDED_CURVE()
B_SPLINE_CURVE(5,(#21061,#21062,#21063,#21064,#21065,#21066,#21067,#21068,
#21069,#21070,#21071,#21072,#21073,#21074,#21075,#21076,#21077,#21078,#21079,
#21080,#21081,#21082,#21083,#21084,#21085,#21086,#21087,#21088,#21089,#21090,
#21091,#21092,#21093,#21094,#21095,#21096,#21097,#21098,#21099,#21100,#21101,
#21102,#21103,#21104,#21105,#21106,#21107,#21108,#21109,#21110,#21111,#21112,
#21113,#21114,#21115,#21116,#21117,#21118,#21119,#21120,#21121,#21122,#21123,
#21124,#21125,#21126,#21127,#21128,#21129,#21130),.UNSPECIFIED.,.F.,.F.)
B_SPLINE_CURVE_WITH_KNOTS((6,1,1,1,1,1,1,1,1,1,1,1,1,1,1,1,1,1,1,1,1,1,
1,1,1,1,1,1,1,1,1,1,1,1,1,1,1,1,1,1,1,1,1,1,1,1,1,1,1,1,1,1,1,1,1,1,1,1,
1,1,1,1,1,1,1,6),(0.,0.0153846153846154,0.0307692307692308,0.0461538461538462,
0.0615384615384615,0.0769230769230769,0.0923076923076923,0.107692307692308,
0.123076923076923,0.138461538461538,0.153846153846154,0.169230769230769,
0.184615384615385,0.2,0.215384615384615,0.230769230769231,0.246153846153846,
0.261538461538462,0.276923076923077,0.292307692307692,0.307692307692308,
0.323076923076923,0.338461538461538,0.353846153846154,0.369230769230769,
0.384615384615385,0.4,0.415384615384615,0.430769230769231,0.446153846153846,
0.461538461538462,0.476923076923077,0.492307692307692,0.507692307692308,
0.523076923076923,0.538461538461538,0.553846153846154,0.569230769230769,
0.584615384615384,0.6,0.615384615384615,0.63076923076923,0.646153846153846,
0.661538461538461,0.676923076923076,0.692307692307692,0.707692307692307,
0.723076923076922,0.738461538461538,0.753846153846153,0.769230769230768,
0.784615384615384,0.799999999999999,0.815384615384614,0.83076923076923,
0.846153846153845,0.86153846153846,0.876923076923076,0.892307692307691,
0.907692307692306,0.923076923076922,0.938461538461537,0.953846153846152,
0.969230769230768,0.984615384615383,1.),.UNSPECIFIED.)
CURVE()
GEOMETRIC_REPRESENTATION_ITEM()
RATIONAL_B_SPLINE_CURVE((1.,1.,1.,1.,1.,1.,1.,1.,1.,1.,1.,1.,1.,1.,1.,1.,
1.,1.,1.,1.,1.,1.,1.,1.,1.,1.,1.,1.,1.,1.,1.,1.,1.,1.,1.,1.,1.,1.,1.,1.,
1.,1.,1.,1.,1.,1.,1.,1.,1.,1.,1.,1.,1.,1.,1.,1.,1.,1.,1.,1.,1.,1.,1.,1.,
1.,1.,1.,1.,1.,1.))
REPRESENTATION_ITEM('')
);
#171=(
BOUNDED_CURVE()
B_SPLINE_CURVE(5,(#21284,#21285,#21286,#21287,#21288,#21289,#21290,#21291,
#21292,#21293,#21294,#21295,#21296,#21297,#21298,#21299,#21300,#21301,#21302,
#21303,#21304,#21305,#21306,#21307,#21308,#21309,#21310,#21311,#21312,#21313,
#21314,#21315,#21316,#21317,#21318,#21319,#21320,#21321,#21322,#21323,#21324,
#21325,#21326,#21327,#21328,#21329,#21330,#21331,#21332,#21333,#21334,#21335,
#21336,#21337,#21338,#21339,#21340,#21341,#21342,#21343,#21344,#21345,#21346,
#21347,#21348,#21349,#21350,#21351,#21352,#21353),.UNSPECIFIED.,.F.,.F.)
B_SPLINE_CURVE_WITH_KNOTS((6,1,1,1,1,1,1,1,1,1,1,1,1,1,1,1,1,1,1,1,1,1,
1,1,1,1,1,1,1,1,1,1,1,1,1,1,1,1,1,1,1,1,1,1,1,1,1,1,1,1,1,1,1,1,1,1,1,1,
1,1,1,1,1,1,1,6),(-1.,-0.984615384615383,-0.969230769230768,-0.953846153846152,
-0.938461538461537,-0.923076923076922,-0.907692307692306,-0.892307692307691,
-0.876923076923076,-0.86153846153846,-0.846153846153845,-0.83076923076923,
-0.815384615384614,-0.799999999999999,-0.784615384615384,-0.769230769230768,
-0.753846153846153,-0.738461538461538,-0.723076923076922,-0.707692307692307,
-0.692307692307692,-0.676923076923076,-0.661538461538461,-0.646153846153846,
-0.63076923076923,-0.615384615384615,-0.6,-0.584615384615384,-0.569230769230769,
-0.553846153846154,-0.538461538461538,-0.523076923076923,-0.507692307692308,
-0.492307692307692,-0.476923076923077,-0.461538461538462,-0.446153846153846,
-0.430769230769231,-0.415384615384615,-0.4,-0.384615384615385,-0.369230769230769,
-0.353846153846154,-0.338461538461538,-0.323076923076923,-0.307692307692308,
-0.292307692307692,-0.276923076923077,-0.261538461538462,-0.246153846153846,
-0.230769230769231,-0.215384615384615,-0.2,-0.184615384615385,-0.169230769230769,
-0.153846153846154,-0.138461538461538,-0.123076923076923,-0.107692307692308,
-0.0923076923076923,-0.0769230769230769,-0.0615384615384615,-0.0461538461538462,
-0.0307692307692308,-0.0153846153846154,0.),.UNSPECIFIED.)
CURVE()
GEOMETRIC_REPRESENTATION_ITEM()
RATIONAL_B_SPLINE_CURVE((1.,1.,1.,1.,1.,1.,1.,1.,1.,1.,1.,1.,1.,1.,1.,1.,
1.,1.,1.,1.,1.,1.,1.,1.,1.,1.,1.,1.,1.,1.,1.,1.,1.,1.,1.,1.,1.,1.,1.,1.,
1.,1.,1.,1.,1.,1.,1.,1.,1.,1.,1.,1.,1.,1.,1.,1.,1.,1.,1.,1.,1.,1.,1.,1.,
1.,1.,1.,1.,1.,1.))
REPRESENTATION_ITEM('')
);
#172=(
BOUNDED_CURVE()
B_SPLINE_CURVE(5,(#21500,#21501,#21502,#21503,#21504,#21505,#21506,#21507,
#21508,#21509,#21510,#21511,#21512,#21513,#21514,#21515,#21516,#21517,#21518,
#21519,#21520,#21521,#21522,#21523,#21524,#21525,#21526,#21527,#21528,#21529,
#21530,#21531,#21532,#21533,#21534,#21535,#21536,#21537,#21538,#21539,#21540,
#21541,#21542,#21543,#21544,#21545,#21546,#21547,#21548,#21549,#21550,#21551,
#21552,#21553,#21554,#21555,#21556,#21557,#21558,#21559,#21560,#21561,#21562,
#21563,#21564,#21565,#21566,#21567,#21568,#21569),.UNSPECIFIED.,.F.,.F.)
B_SPLINE_CURVE_WITH_KNOTS((6,1,1,1,1,1,1,1,1,1,1,1,1,1,1,1,1,1,1,1,1,1,
1,1,1,1,1,1,1,1,1,1,1,1,1,1,1,1,1,1,1,1,1,1,1,1,1,1,1,1,1,1,1,1,1,1,1,1,
1,1,1,1,1,1,1,6),(-1.,-0.984615384615383,-0.969230769230768,-0.953846153846152,
-0.938461538461537,-0.923076923076922,-0.907692307692306,-0.892307692307691,
-0.876923076923076,-0.86153846153846,-0.846153846153845,-0.83076923076923,
-0.815384615384614,-0.799999999999999,-0.784615384615384,-0.769230769230768,
-0.753846153846153,-0.738461538461538,-0.723076923076922,-0.707692307692307,
-0.692307692307692,-0.676923076923076,-0.661538461538461,-0.646153846153846,
-0.63076923076923,-0.615384615384615,-0.6,-0.584615384615384,-0.569230769230769,
-0.553846153846154,-0.538461538461538,-0.523076923076923,-0.507692307692308,
-0.492307692307692,-0.476923076923077,-0.461538461538462,-0.446153846153846,
-0.430769230769231,-0.415384615384615,-0.4,-0.384615384615385,-0.369230769230769,
-0.353846153846154,-0.338461538461538,-0.323076923076923,-0.307692307692308,
-0.292307692307692,-0.276923076923077,-0.261538461538462,-0.246153846153846,
-0.230769230769231,-0.215384615384615,-0.2,-0.184615384615385,-0.169230769230769,
-0.153846153846154,-0.138461538461538,-0.123076923076923,-0.107692307692308,
-0.0923076923076923,-0.0769230769230769,-0.0615384615384615,-0.0461538461538462,
-0.0307692307692308,-0.0153846153846154,0.),.UNSPECIFIED.)
CURVE()
GEOMETRIC_REPRESENTATION_ITEM()
RATIONAL_B_SPLINE_CURVE((1.,1.,1.,1.,1.,1.,1.,1.,1.,1.,1.,1.,1.,1.,1.,1.,
1.,1.,1.,1.,1.,1.,1.,1.,1.,1.,1.,1.,1.,1.,1.,1.,1.,1.,1.,1.,1.,1.,1.,1.,
1.,1.,1.,1.,1.,1.,1.,1.,1.,1.,1.,1.,1.,1.,1.,1.,1.,1.,1.,1.,1.,1.,1.,1.,
1.,1.,1.,1.,1.,1.))
REPRESENTATION_ITEM('')
);
#173=(
BOUNDED_CURVE()
B_SPLINE_CURVE(5,(#21716,#21717,#21718,#21719,#21720,#21721,#21722,#21723,
#21724,#21725,#21726,#21727,#21728,#21729,#21730,#21731,#21732,#21733,#21734,
#21735,#21736,#21737,#21738,#21739,#21740,#21741,#21742,#21743,#21744,#21745,
#21746,#21747,#21748,#21749,#21750,#21751,#21752,#21753,#21754,#21755,#21756,
#21757,#21758,#21759,#21760,#21761,#21762,#21763,#21764,#21765,#21766,#21767,
#21768,#21769,#21770,#21771,#21772,#21773,#21774,#21775,#21776,#21777,#21778,
#21779,#21780,#21781,#21782,#21783,#21784,#21785),.UNSPECIFIED.,.F.,.F.)
B_SPLINE_CURVE_WITH_KNOTS((6,1,1,1,1,1,1,1,1,1,1,1,1,1,1,1,1,1,1,1,1,1,
1,1,1,1,1,1,1,1,1,1,1,1,1,1,1,1,1,1,1,1,1,1,1,1,1,1,1,1,1,1,1,1,1,1,1,1,
1,1,1,1,1,1,1,6),(-1.,-0.984615384615383,-0.969230769230768,-0.953846153846152,
-0.938461538461537,-0.923076923076922,-0.907692307692306,-0.892307692307691,
-0.876923076923076,-0.86153846153846,-0.846153846153845,-0.83076923076923,
-0.815384615384614,-0.799999999999999,-0.784615384615384,-0.769230769230768,
-0.753846153846153,-0.738461538461538,-0.723076923076922,-0.707692307692307,
-0.692307692307692,-0.676923076923076,-0.661538461538461,-0.646153846153846,
-0.63076923076923,-0.615384615384615,-0.6,-0.584615384615384,-0.569230769230769,
-0.553846153846154,-0.538461538461538,-0.523076923076923,-0.507692307692308,
-0.492307692307692,-0.476923076923077,-0.461538461538462,-0.446153846153846,
-0.430769230769231,-0.415384615384615,-0.4,-0.384615384615385,-0.369230769230769,
-0.353846153846154,-0.338461538461538,-0.323076923076923,-0.307692307692308,
-0.292307692307692,-0.276923076923077,-0.261538461538462,-0.246153846153846,
-0.230769230769231,-0.215384615384615,-0.2,-0.184615384615385,-0.169230769230769,
-0.153846153846154,-0.138461538461538,-0.123076923076923,-0.107692307692308,
-0.0923076923076923,-0.0769230769230769,-0.0615384615384615,-0.0461538461538462,
-0.0307692307692308,-0.0153846153846154,0.),.UNSPECIFIED.)
CURVE()
GEOMETRIC_REPRESENTATION_ITEM()
RATIONAL_B_SPLINE_CURVE((1.,1.,1.,1.,1.,1.,1.,1.,1.,1.,1.,1.,1.,1.,1.,1.,
1.,1.,1.,1.,1.,1.,1.,1.,1.,1.,1.,1.,1.,1.,1.,1.,1.,1.,1.,1.,1.,1.,1.,1.,
1.,1.,1.,1.,1.,1.,1.,1.,1.,1.,1.,1.,1.,1.,1.,1.,1.,1.,1.,1.,1.,1.,1.,1.,
1.,1.,1.,1.,1.,1.))
REPRESENTATION_ITEM('')
);
#174=(
BOUNDED_CURVE()
B_SPLINE_CURVE(5,(#21932,#21933,#21934,#21935,#21936,#21937,#21938,#21939,
#21940,#21941,#21942,#21943,#21944,#21945,#21946,#21947,#21948,#21949,#21950,
#21951,#21952,#21953,#21954,#21955,#21956,#21957,#21958,#21959,#21960,#21961,
#21962,#21963,#21964,#21965,#21966,#21967,#21968,#21969,#21970,#21971,#21972,
#21973,#21974,#21975,#21976,#21977,#21978,#21979,#21980,#21981,#21982,#21983,
#21984,#21985,#21986,#21987,#21988,#21989,#21990,#21991,#21992,#21993,#21994,
#21995,#21996,#21997,#21998,#21999,#22000,#22001),.UNSPECIFIED.,.F.,.F.)
B_SPLINE_CURVE_WITH_KNOTS((6,1,1,1,1,1,1,1,1,1,1,1,1,1,1,1,1,1,1,1,1,1,
1,1,1,1,1,1,1,1,1,1,1,1,1,1,1,1,1,1,1,1,1,1,1,1,1,1,1,1,1,1,1,1,1,1,1,1,
1,1,1,1,1,1,1,6),(-1.,-0.984615384615383,-0.969230769230768,-0.953846153846152,
-0.938461538461537,-0.923076923076922,-0.907692307692306,-0.892307692307691,
-0.876923076923076,-0.86153846153846,-0.846153846153845,-0.83076923076923,
-0.815384615384614,-0.799999999999999,-0.784615384615384,-0.769230769230768,
-0.753846153846153,-0.738461538461538,-0.723076923076922,-0.707692307692307,
-0.692307692307692,-0.676923076923076,-0.661538461538461,-0.646153846153846,
-0.63076923076923,-0.615384615384615,-0.6,-0.584615384615384,-0.569230769230769,
-0.553846153846154,-0.538461538461538,-0.523076923076923,-0.507692307692308,
-0.492307692307692,-0.476923076923077,-0.461538461538462,-0.446153846153846,
-0.430769230769231,-0.415384615384615,-0.4,-0.384615384615385,-0.369230769230769,
-0.353846153846154,-0.338461538461538,-0.323076923076923,-0.307692307692308,
-0.292307692307692,-0.276923076923077,-0.261538461538462,-0.246153846153846,
-0.230769230769231,-0.215384615384615,-0.2,-0.184615384615385,-0.169230769230769,
-0.153846153846154,-0.138461538461538,-0.123076923076923,-0.107692307692308,
-0.0923076923076923,-0.0769230769230769,-0.0615384615384615,-0.0461538461538462,
-0.0307692307692308,-0.0153846153846154,0.),.UNSPECIFIED.)
CURVE()
GEOMETRIC_REPRESENTATION_ITEM()
RATIONAL_B_SPLINE_CURVE((1.,1.,1.,1.,1.,1.,1.,1.,1.,1.,1.,1.,1.,1.,1.,1.,
1.,1.,1.,1.,1.,1.,1.,1.,1.,1.,1.,1.,1.,1.,1.,1.,1.,1.,1.,1.,1.,1.,1.,1.,
1.,1.,1.,1.,1.,1.,1.,1.,1.,1.,1.,1.,1.,1.,1.,1.,1.,1.,1.,1.,1.,1.,1.,1.,
1.,1.,1.,1.,1.,1.))
REPRESENTATION_ITEM('')
);
#175=(
BOUNDED_CURVE()
B_SPLINE_CURVE(5,(#22148,#22149,#22150,#22151,#22152,#22153,#22154,#22155,
#22156,#22157,#22158,#22159,#22160,#22161,#22162,#22163,#22164,#22165,#22166,
#22167,#22168,#22169,#22170,#22171,#22172,#22173,#22174,#22175,#22176,#22177,
#22178,#22179,#22180,#22181,#22182,#22183,#22184,#22185,#22186,#22187,#22188,
#22189,#22190,#22191,#22192,#22193,#22194,#22195,#22196,#22197,#22198,#22199,
#22200,#22201,#22202,#22203,#22204,#22205,#22206,#22207,#22208,#22209,#22210,
#22211,#22212,#22213,#22214,#22215,#22216,#22217),.UNSPECIFIED.,.F.,.F.)
B_SPLINE_CURVE_WITH_KNOTS((6,1,1,1,1,1,1,1,1,1,1,1,1,1,1,1,1,1,1,1,1,1,
1,1,1,1,1,1,1,1,1,1,1,1,1,1,1,1,1,1,1,1,1,1,1,1,1,1,1,1,1,1,1,1,1,1,1,1,
1,1,1,1,1,1,1,6),(-1.,-0.984615384615383,-0.969230769230768,-0.953846153846152,
-0.938461538461537,-0.923076923076922,-0.907692307692306,-0.892307692307691,
-0.876923076923076,-0.86153846153846,-0.846153846153845,-0.83076923076923,
-0.815384615384614,-0.799999999999999,-0.784615384615384,-0.769230769230768,
-0.753846153846153,-0.738461538461538,-0.723076923076922,-0.707692307692307,
-0.692307692307692,-0.676923076923076,-0.661538461538461,-0.646153846153846,
-0.63076923076923,-0.615384615384615,-0.6,-0.584615384615384,-0.569230769230769,
-0.553846153846154,-0.538461538461538,-0.523076923076923,-0.507692307692308,
-0.492307692307692,-0.476923076923077,-0.461538461538462,-0.446153846153846,
-0.430769230769231,-0.415384615384615,-0.4,-0.384615384615385,-0.369230769230769,
-0.353846153846154,-0.338461538461538,-0.323076923076923,-0.307692307692308,
-0.292307692307692,-0.276923076923077,-0.261538461538462,-0.246153846153846,
-0.230769230769231,-0.215384615384615,-0.2,-0.184615384615385,-0.169230769230769,
-0.153846153846154,-0.138461538461538,-0.123076923076923,-0.107692307692308,
-0.0923076923076923,-0.0769230769230769,-0.0615384615384615,-0.0461538461538462,
-0.0307692307692308,-0.0153846153846154,0.),.UNSPECIFIED.)
CURVE()
GEOMETRIC_REPRESENTATION_ITEM()
RATIONAL_B_SPLINE_CURVE((1.,1.,1.,1.,1.,1.,1.,1.,1.,1.,1.,1.,1.,1.,1.,1.,
1.,1.,1.,1.,1.,1.,1.,1.,1.,1.,1.,1.,1.,1.,1.,1.,1.,1.,1.,1.,1.,1.,1.,1.,
1.,1.,1.,1.,1.,1.,1.,1.,1.,1.,1.,1.,1.,1.,1.,1.,1.,1.,1.,1.,1.,1.,1.,1.,
1.,1.,1.,1.,1.,1.))
REPRESENTATION_ITEM('')
);
#176=(
BOUNDED_CURVE()
B_SPLINE_CURVE(5,(#22364,#22365,#22366,#22367,#22368,#22369,#22370,#22371,
#22372,#22373,#22374,#22375,#22376,#22377,#22378,#22379,#22380,#22381,#22382,
#22383,#22384,#22385,#22386,#22387,#22388,#22389,#22390,#22391,#22392,#22393,
#22394,#22395,#22396,#22397,#22398,#22399,#22400,#22401,#22402,#22403,#22404,
#22405,#22406,#22407,#22408,#22409,#22410,#22411,#22412,#22413,#22414,#22415,
#22416,#22417,#22418,#22419,#22420,#22421,#22422,#22423,#22424,#22425,#22426,
#22427,#22428,#22429,#22430,#22431,#22432,#22433),.UNSPECIFIED.,.F.,.F.)
B_SPLINE_CURVE_WITH_KNOTS((6,1,1,1,1,1,1,1,1,1,1,1,1,1,1,1,1,1,1,1,1,1,
1,1,1,1,1,1,1,1,1,1,1,1,1,1,1,1,1,1,1,1,1,1,1,1,1,1,1,1,1,1,1,1,1,1,1,1,
1,1,1,1,1,1,1,6),(-1.,-0.984615384615383,-0.969230769230768,-0.953846153846152,
-0.938461538461537,-0.923076923076922,-0.907692307692306,-0.892307692307691,
-0.876923076923076,-0.86153846153846,-0.846153846153845,-0.83076923076923,
-0.815384615384614,-0.799999999999999,-0.784615384615384,-0.769230769230768,
-0.753846153846153,-0.738461538461538,-0.723076923076922,-0.707692307692307,
-0.692307692307692,-0.676923076923076,-0.661538461538461,-0.646153846153846,
-0.63076923076923,-0.615384615384615,-0.6,-0.584615384615384,-0.569230769230769,
-0.553846153846154,-0.538461538461538,-0.523076923076923,-0.507692307692308,
-0.492307692307692,-0.476923076923077,-0.461538461538462,-0.446153846153846,
-0.430769230769231,-0.415384615384615,-0.4,-0.384615384615385,-0.369230769230769,
-0.353846153846154,-0.338461538461538,-0.323076923076923,-0.307692307692308,
-0.292307692307692,-0.276923076923077,-0.261538461538462,-0.246153846153846,
-0.230769230769231,-0.215384615384615,-0.2,-0.184615384615385,-0.169230769230769,
-0.153846153846154,-0.138461538461538,-0.123076923076923,-0.107692307692308,
-0.0923076923076923,-0.0769230769230769,-0.0615384615384615,-0.0461538461538462,
-0.0307692307692308,-0.0153846153846154,0.),.UNSPECIFIED.)
CURVE()
GEOMETRIC_REPRESENTATION_ITEM()
RATIONAL_B_SPLINE_CURVE((1.,1.,1.,1.,1.,1.,1.,1.,1.,1.,1.,1.,1.,1.,1.,1.,
1.,1.,1.,1.,1.,1.,1.,1.,1.,1.,1.,1.,1.,1.,1.,1.,1.,1.,1.,1.,1.,1.,1.,1.,
1.,1.,1.,1.,1.,1.,1.,1.,1.,1.,1.,1.,1.,1.,1.,1.,1.,1.,1.,1.,1.,1.,1.,1.,
1.,1.,1.,1.,1.,1.))
REPRESENTATION_ITEM('')
);
#177=(
BOUNDED_CURVE()
B_SPLINE_CURVE(5,(#22580,#22581,#22582,#22583,#22584,#22585,#22586,#22587,
#22588,#22589,#22590,#22591,#22592,#22593,#22594,#22595,#22596,#22597,#22598,
#22599,#22600,#22601,#22602,#22603,#22604,#22605,#22606,#22607,#22608,#22609,
#22610,#22611,#22612,#22613,#22614,#22615,#22616,#22617,#22618,#22619,#22620,
#22621,#22622,#22623,#22624,#22625,#22626,#22627,#22628,#22629,#22630,#22631,
#22632,#22633,#22634,#22635,#22636,#22637,#22638,#22639,#22640,#22641,#22642,
#22643,#22644,#22645,#22646,#22647,#22648,#22649),.UNSPECIFIED.,.F.,.F.)
B_SPLINE_CURVE_WITH_KNOTS((6,1,1,1,1,1,1,1,1,1,1,1,1,1,1,1,1,1,1,1,1,1,
1,1,1,1,1,1,1,1,1,1,1,1,1,1,1,1,1,1,1,1,1,1,1,1,1,1,1,1,1,1,1,1,1,1,1,1,
1,1,1,1,1,1,1,6),(-1.,-0.984615384615383,-0.969230769230768,-0.953846153846152,
-0.938461538461537,-0.923076923076922,-0.907692307692306,-0.892307692307691,
-0.876923076923076,-0.86153846153846,-0.846153846153845,-0.83076923076923,
-0.815384615384614,-0.799999999999999,-0.784615384615384,-0.769230769230768,
-0.753846153846153,-0.738461538461538,-0.723076923076922,-0.707692307692307,
-0.692307692307692,-0.676923076923076,-0.661538461538461,-0.646153846153846,
-0.63076923076923,-0.615384615384615,-0.6,-0.584615384615384,-0.569230769230769,
-0.553846153846154,-0.538461538461538,-0.523076923076923,-0.507692307692308,
-0.492307692307692,-0.476923076923077,-0.461538461538462,-0.446153846153846,
-0.430769230769231,-0.415384615384615,-0.4,-0.384615384615385,-0.369230769230769,
-0.353846153846154,-0.338461538461538,-0.323076923076923,-0.307692307692308,
-0.292307692307692,-0.276923076923077,-0.261538461538462,-0.246153846153846,
-0.230769230769231,-0.215384615384615,-0.2,-0.184615384615385,-0.169230769230769,
-0.153846153846154,-0.138461538461538,-0.123076923076923,-0.107692307692308,
-0.0923076923076923,-0.0769230769230769,-0.0615384615384615,-0.0461538461538462,
-0.0307692307692308,-0.0153846153846154,0.),.UNSPECIFIED.)
CURVE()
GEOMETRIC_REPRESENTATION_ITEM()
RATIONAL_B_SPLINE_CURVE((1.,1.,1.,1.,1.,1.,1.,1.,1.,1.,1.,1.,1.,1.,1.,1.,
1.,1.,1.,1.,1.,1.,1.,1.,1.,1.,1.,1.,1.,1.,1.,1.,1.,1.,1.,1.,1.,1.,1.,1.,
1.,1.,1.,1.,1.,1.,1.,1.,1.,1.,1.,1.,1.,1.,1.,1.,1.,1.,1.,1.,1.,1.,1.,1.,
1.,1.,1.,1.,1.,1.))
REPRESENTATION_ITEM('')
);
#178=(
BOUNDED_CURVE()
B_SPLINE_CURVE(5,(#22796,#22797,#22798,#22799,#22800,#22801,#22802,#22803,
#22804,#22805,#22806,#22807,#22808,#22809,#22810,#22811,#22812,#22813,#22814,
#22815,#22816,#22817,#22818,#22819,#22820,#22821,#22822,#22823,#22824,#22825,
#22826,#22827,#22828,#22829,#22830,#22831,#22832,#22833,#22834,#22835,#22836,
#22837,#22838,#22839,#22840,#22841,#22842,#22843,#22844,#22845,#22846,#22847,
#22848,#22849,#22850,#22851,#22852,#22853,#22854,#22855,#22856,#22857,#22858,
#22859,#22860,#22861,#22862,#22863,#22864,#22865),.UNSPECIFIED.,.F.,.F.)
B_SPLINE_CURVE_WITH_KNOTS((6,1,1,1,1,1,1,1,1,1,1,1,1,1,1,1,1,1,1,1,1,1,
1,1,1,1,1,1,1,1,1,1,1,1,1,1,1,1,1,1,1,1,1,1,1,1,1,1,1,1,1,1,1,1,1,1,1,1,
1,1,1,1,1,1,1,6),(-1.,-0.984615384615383,-0.969230769230768,-0.953846153846152,
-0.938461538461537,-0.923076923076922,-0.907692307692306,-0.892307692307691,
-0.876923076923076,-0.86153846153846,-0.846153846153845,-0.83076923076923,
-0.815384615384614,-0.799999999999999,-0.784615384615384,-0.769230769230768,
-0.753846153846153,-0.738461538461538,-0.723076923076922,-0.707692307692307,
-0.692307692307692,-0.676923076923076,-0.661538461538461,-0.646153846153846,
-0.63076923076923,-0.615384615384615,-0.6,-0.584615384615384,-0.569230769230769,
-0.553846153846154,-0.538461538461538,-0.523076923076923,-0.507692307692308,
-0.492307692307692,-0.476923076923077,-0.461538461538462,-0.446153846153846,
-0.430769230769231,-0.415384615384615,-0.4,-0.384615384615385,-0.369230769230769,
-0.353846153846154,-0.338461538461538,-0.323076923076923,-0.307692307692308,
-0.292307692307692,-0.276923076923077,-0.261538461538462,-0.246153846153846,
-0.230769230769231,-0.215384615384615,-0.2,-0.184615384615385,-0.169230769230769,
-0.153846153846154,-0.138461538461538,-0.123076923076923,-0.107692307692308,
-0.0923076923076923,-0.0769230769230769,-0.0615384615384615,-0.0461538461538462,
-0.0307692307692308,-0.0153846153846154,0.),.UNSPECIFIED.)
CURVE()
GEOMETRIC_REPRESENTATION_ITEM()
RATIONAL_B_SPLINE_CURVE((1.,1.,1.,1.,1.,1.,1.,1.,1.,1.,1.,1.,1.,1.,1.,1.,
1.,1.,1.,1.,1.,1.,1.,1.,1.,1.,1.,1.,1.,1.,1.,1.,1.,1.,1.,1.,1.,1.,1.,1.,
1.,1.,1.,1.,1.,1.,1.,1.,1.,1.,1.,1.,1.,1.,1.,1.,1.,1.,1.,1.,1.,1.,1.,1.,
1.,1.,1.,1.,1.,1.))
REPRESENTATION_ITEM('')
);
#179=(
BOUNDED_CURVE()
B_SPLINE_CURVE(5,(#23012,#23013,#23014,#23015,#23016,#23017,#23018,#23019,
#23020,#23021,#23022,#23023,#23024,#23025,#23026,#23027,#23028,#23029,#23030,
#23031,#23032,#23033,#23034,#23035,#23036,#23037,#23038,#23039,#23040,#23041,
#23042,#23043,#23044,#23045,#23046,#23047,#23048,#23049,#23050,#23051,#23052,
#23053,#23054,#23055,#23056,#23057,#23058,#23059,#23060,#23061,#23062,#23063,
#23064,#23065,#23066,#23067,#23068,#23069,#23070,#23071,#23072,#23073,#23074,
#23075,#23076,#23077,#23078,#23079,#23080,#23081),.UNSPECIFIED.,.F.,.F.)
B_SPLINE_CURVE_WITH_KNOTS((6,1,1,1,1,1,1,1,1,1,1,1,1,1,1,1,1,1,1,1,1,1,
1,1,1,1,1,1,1,1,1,1,1,1,1,1,1,1,1,1,1,1,1,1,1,1,1,1,1,1,1,1,1,1,1,1,1,1,
1,1,1,1,1,1,1,6),(-1.,-0.984615384615383,-0.969230769230768,-0.953846153846152,
-0.938461538461537,-0.923076923076922,-0.907692307692306,-0.892307692307691,
-0.876923076923076,-0.86153846153846,-0.846153846153845,-0.83076923076923,
-0.815384615384614,-0.799999999999999,-0.784615384615384,-0.769230769230768,
-0.753846153846153,-0.738461538461538,-0.723076923076922,-0.707692307692307,
-0.692307692307692,-0.676923076923076,-0.661538461538461,-0.646153846153846,
-0.63076923076923,-0.615384615384615,-0.6,-0.584615384615384,-0.569230769230769,
-0.553846153846154,-0.538461538461538,-0.523076923076923,-0.507692307692308,
-0.492307692307692,-0.476923076923077,-0.461538461538462,-0.446153846153846,
-0.430769230769231,-0.415384615384615,-0.4,-0.384615384615385,-0.369230769230769,
-0.353846153846154,-0.338461538461538,-0.323076923076923,-0.307692307692308,
-0.292307692307692,-0.276923076923077,-0.261538461538462,-0.246153846153846,
-0.230769230769231,-0.215384615384615,-0.2,-0.184615384615385,-0.169230769230769,
-0.153846153846154,-0.138461538461538,-0.123076923076923,-0.107692307692308,
-0.0923076923076923,-0.0769230769230769,-0.0615384615384615,-0.0461538461538462,
-0.0307692307692308,-0.0153846153846154,0.),.UNSPECIFIED.)
CURVE()
GEOMETRIC_REPRESENTATION_ITEM()
RATIONAL_B_SPLINE_CURVE((1.,1.,1.,1.,1.,1.,1.,1.,1.,1.,1.,1.,1.,1.,1.,1.,
1.,1.,1.,1.,1.,1.,1.,1.,1.,1.,1.,1.,1.,1.,1.,1.,1.,1.,1.,1.,1.,1.,1.,1.,
1.,1.,1.,1.,1.,1.,1.,1.,1.,1.,1.,1.,1.,1.,1.,1.,1.,1.,1.,1.,1.,1.,1.,1.,
1.,1.,1.,1.,1.,1.))
REPRESENTATION_ITEM('')
);
#180=(
BOUNDED_CURVE()
B_SPLINE_CURVE(5,(#23228,#23229,#23230,#23231,#23232,#23233,#23234,#23235,
#23236,#23237,#23238,#23239,#23240,#23241,#23242,#23243,#23244,#23245,#23246,
#23247,#23248,#23249,#23250,#23251,#23252,#23253,#23254,#23255,#23256,#23257,
#23258,#23259,#23260,#23261,#23262,#23263,#23264,#23265,#23266,#23267,#23268,
#23269,#23270,#23271,#23272,#23273,#23274,#23275,#23276,#23277,#23278,#23279,
#23280,#23281,#23282,#23283,#23284,#23285,#23286,#23287,#23288,#23289,#23290,
#23291,#23292,#23293,#23294,#23295,#23296,#23297),.UNSPECIFIED.,.F.,.F.)
B_SPLINE_CURVE_WITH_KNOTS((6,1,1,1,1,1,1,1,1,1,1,1,1,1,1,1,1,1,1,1,1,1,
1,1,1,1,1,1,1,1,1,1,1,1,1,1,1,1,1,1,1,1,1,1,1,1,1,1,1,1,1,1,1,1,1,1,1,1,
1,1,1,1,1,1,1,6),(-1.,-0.984615384615383,-0.969230769230768,-0.953846153846152,
-0.938461538461537,-0.923076923076922,-0.907692307692306,-0.892307692307691,
-0.876923076923076,-0.86153846153846,-0.846153846153845,-0.83076923076923,
-0.815384615384614,-0.799999999999999,-0.784615384615384,-0.769230769230768,
-0.753846153846153,-0.738461538461538,-0.723076923076922,-0.707692307692307,
-0.692307692307692,-0.676923076923076,-0.661538461538461,-0.646153846153846,
-0.63076923076923,-0.615384615384615,-0.6,-0.584615384615384,-0.569230769230769,
-0.553846153846154,-0.538461538461538,-0.523076923076923,-0.507692307692308,
-0.492307692307692,-0.476923076923077,-0.461538461538462,-0.446153846153846,
-0.430769230769231,-0.415384615384615,-0.4,-0.384615384615385,-0.369230769230769,
-0.353846153846154,-0.338461538461538,-0.323076923076923,-0.307692307692308,
-0.292307692307692,-0.276923076923077,-0.261538461538462,-0.246153846153846,
-0.230769230769231,-0.215384615384615,-0.2,-0.184615384615385,-0.169230769230769,
-0.153846153846154,-0.138461538461538,-0.123076923076923,-0.107692307692308,
-0.0923076923076923,-0.0769230769230769,-0.0615384615384615,-0.0461538461538462,
-0.0307692307692308,-0.0153846153846154,0.),.UNSPECIFIED.)
CURVE()
GEOMETRIC_REPRESENTATION_ITEM()
RATIONAL_B_SPLINE_CURVE((1.,1.,1.,1.,1.,1.,1.,1.,1.,1.,1.,1.,1.,1.,1.,1.,
1.,1.,1.,1.,1.,1.,1.,1.,1.,1.,1.,1.,1.,1.,1.,1.,1.,1.,1.,1.,1.,1.,1.,1.,
1.,1.,1.,1.,1.,1.,1.,1.,1.,1.,1.,1.,1.,1.,1.,1.,1.,1.,1.,1.,1.,1.,1.,1.,
1.,1.,1.,1.,1.,1.))
REPRESENTATION_ITEM('')
);
#181=(
BOUNDED_CURVE()
B_SPLINE_CURVE(5,(#23444,#23445,#23446,#23447,#23448,#23449,#23450,#23451,
#23452,#23453,#23454,#23455,#23456,#23457,#23458,#23459,#23460,#23461,#23462,
#23463,#23464,#23465,#23466,#23467,#23468,#23469,#23470,#23471,#23472,#23473,
#23474,#23475,#23476,#23477,#23478,#23479,#23480,#23481,#23482,#23483,#23484,
#23485,#23486,#23487,#23488,#23489,#23490,#23491,#23492,#23493,#23494,#23495,
#23496,#23497,#23498,#23499,#23500,#23501,#23502,#23503,#23504,#23505,#23506,
#23507,#23508,#23509,#23510,#23511,#23512,#23513),.UNSPECIFIED.,.F.,.F.)
B_SPLINE_CURVE_WITH_KNOTS((6,1,1,1,1,1,1,1,1,1,1,1,1,1,1,1,1,1,1,1,1,1,
1,1,1,1,1,1,1,1,1,1,1,1,1,1,1,1,1,1,1,1,1,1,1,1,1,1,1,1,1,1,1,1,1,1,1,1,
1,1,1,1,1,1,1,6),(-1.,-0.984615384615383,-0.969230769230768,-0.953846153846152,
-0.938461538461537,-0.923076923076922,-0.907692307692306,-0.892307692307691,
-0.876923076923076,-0.86153846153846,-0.846153846153845,-0.83076923076923,
-0.815384615384614,-0.799999999999999,-0.784615384615384,-0.769230769230768,
-0.753846153846153,-0.738461538461538,-0.723076923076922,-0.707692307692307,
-0.692307692307692,-0.676923076923076,-0.661538461538461,-0.646153846153846,
-0.63076923076923,-0.615384615384615,-0.6,-0.584615384615384,-0.569230769230769,
-0.553846153846154,-0.538461538461538,-0.523076923076923,-0.507692307692308,
-0.492307692307692,-0.476923076923077,-0.461538461538462,-0.446153846153846,
-0.430769230769231,-0.415384615384615,-0.4,-0.384615384615385,-0.369230769230769,
-0.353846153846154,-0.338461538461538,-0.323076923076923,-0.307692307692308,
-0.292307692307692,-0.276923076923077,-0.261538461538462,-0.246153846153846,
-0.230769230769231,-0.215384615384615,-0.2,-0.184615384615385,-0.169230769230769,
-0.153846153846154,-0.138461538461538,-0.123076923076923,-0.107692307692308,
-0.0923076923076923,-0.0769230769230769,-0.0615384615384615,-0.0461538461538462,
-0.0307692307692308,-0.0153846153846154,0.),.UNSPECIFIED.)
CURVE()
GEOMETRIC_REPRESENTATION_ITEM()
RATIONAL_B_SPLINE_CURVE((1.,1.,1.,1.,1.,1.,1.,1.,1.,1.,1.,1.,1.,1.,1.,1.,
1.,1.,1.,1.,1.,1.,1.,1.,1.,1.,1.,1.,1.,1.,1.,1.,1.,1.,1.,1.,1.,1.,1.,1.,
1.,1.,1.,1.,1.,1.,1.,1.,1.,1.,1.,1.,1.,1.,1.,1.,1.,1.,1.,1.,1.,1.,1.,1.,
1.,1.,1.,1.,1.,1.))
REPRESENTATION_ITEM('')
);
#182=(
BOUNDED_CURVE()
B_SPLINE_CURVE(5,(#23660,#23661,#23662,#23663,#23664,#23665,#23666,#23667,
#23668,#23669,#23670,#23671,#23672,#23673,#23674,#23675,#23676,#23677,#23678,
#23679,#23680,#23681,#23682,#23683,#23684,#23685,#23686,#23687,#23688,#23689,
#23690,#23691,#23692,#23693,#23694,#23695,#23696,#23697,#23698,#23699,#23700,
#23701,#23702,#23703,#23704,#23705,#23706,#23707,#23708,#23709,#23710,#23711,
#23712,#23713,#23714,#23715,#23716,#23717,#23718,#23719,#23720,#23721,#23722,
#23723,#23724,#23725,#23726,#23727,#23728,#23729),.UNSPECIFIED.,.F.,.F.)
B_SPLINE_CURVE_WITH_KNOTS((6,1,1,1,1,1,1,1,1,1,1,1,1,1,1,1,1,1,1,1,1,1,
1,1,1,1,1,1,1,1,1,1,1,1,1,1,1,1,1,1,1,1,1,1,1,1,1,1,1,1,1,1,1,1,1,1,1,1,
1,1,1,1,1,1,1,6),(-1.,-0.984615384615383,-0.969230769230768,-0.953846153846152,
-0.938461538461537,-0.923076923076922,-0.907692307692306,-0.892307692307691,
-0.876923076923076,-0.86153846153846,-0.846153846153845,-0.83076923076923,
-0.815384615384614,-0.799999999999999,-0.784615384615384,-0.769230769230768,
-0.753846153846153,-0.738461538461538,-0.723076923076922,-0.707692307692307,
-0.692307692307692,-0.676923076923076,-0.661538461538461,-0.646153846153846,
-0.63076923076923,-0.615384615384615,-0.6,-0.584615384615384,-0.569230769230769,
-0.553846153846154,-0.538461538461538,-0.523076923076923,-0.507692307692308,
-0.492307692307692,-0.476923076923077,-0.461538461538462,-0.446153846153846,
-0.430769230769231,-0.415384615384615,-0.4,-0.384615384615385,-0.369230769230769,
-0.353846153846154,-0.338461538461538,-0.323076923076923,-0.307692307692308,
-0.292307692307692,-0.276923076923077,-0.261538461538462,-0.246153846153846,
-0.230769230769231,-0.215384615384615,-0.2,-0.184615384615385,-0.169230769230769,
-0.153846153846154,-0.138461538461538,-0.123076923076923,-0.107692307692308,
-0.0923076923076923,-0.0769230769230769,-0.0615384615384615,-0.0461538461538462,
-0.0307692307692308,-0.0153846153846154,0.),.UNSPECIFIED.)
CURVE()
GEOMETRIC_REPRESENTATION_ITEM()
RATIONAL_B_SPLINE_CURVE((1.,1.,1.,1.,1.,1.,1.,1.,1.,1.,1.,1.,1.,1.,1.,1.,
1.,1.,1.,1.,1.,1.,1.,1.,1.,1.,1.,1.,1.,1.,1.,1.,1.,1.,1.,1.,1.,1.,1.,1.,
1.,1.,1.,1.,1.,1.,1.,1.,1.,1.,1.,1.,1.,1.,1.,1.,1.,1.,1.,1.,1.,1.,1.,1.,
1.,1.,1.,1.,1.,1.))
REPRESENTATION_ITEM('')
);
#183=(
BOUNDED_CURVE()
B_SPLINE_CURVE(5,(#23876,#23877,#23878,#23879,#23880,#23881,#23882,#23883,
#23884,#23885,#23886,#23887,#23888,#23889,#23890,#23891,#23892,#23893,#23894,
#23895,#23896,#23897,#23898,#23899,#23900,#23901,#23902,#23903,#23904,#23905,
#23906,#23907,#23908,#23909,#23910,#23911,#23912,#23913,#23914,#23915,#23916,
#23917,#23918,#23919,#23920,#23921,#23922,#23923,#23924,#23925,#23926,#23927,
#23928,#23929,#23930,#23931,#23932,#23933,#23934,#23935,#23936,#23937,#23938,
#23939,#23940,#23941,#23942,#23943,#23944,#23945),.UNSPECIFIED.,.F.,.F.)
B_SPLINE_CURVE_WITH_KNOTS((6,1,1,1,1,1,1,1,1,1,1,1,1,1,1,1,1,1,1,1,1,1,
1,1,1,1,1,1,1,1,1,1,1,1,1,1,1,1,1,1,1,1,1,1,1,1,1,1,1,1,1,1,1,1,1,1,1,1,
1,1,1,1,1,1,1,6),(-1.,-0.984615384615383,-0.969230769230768,-0.953846153846152,
-0.938461538461537,-0.923076923076922,-0.907692307692306,-0.892307692307691,
-0.876923076923076,-0.86153846153846,-0.846153846153845,-0.83076923076923,
-0.815384615384614,-0.799999999999999,-0.784615384615384,-0.769230769230768,
-0.753846153846153,-0.738461538461538,-0.723076923076922,-0.707692307692307,
-0.692307692307692,-0.676923076923076,-0.661538461538461,-0.646153846153846,
-0.63076923076923,-0.615384615384615,-0.6,-0.584615384615384,-0.569230769230769,
-0.553846153846154,-0.538461538461538,-0.523076923076923,-0.507692307692308,
-0.492307692307692,-0.476923076923077,-0.461538461538462,-0.446153846153846,
-0.430769230769231,-0.415384615384615,-0.4,-0.384615384615385,-0.369230769230769,
-0.353846153846154,-0.338461538461538,-0.323076923076923,-0.307692307692308,
-0.292307692307692,-0.276923076923077,-0.261538461538462,-0.246153846153846,
-0.230769230769231,-0.215384615384615,-0.2,-0.184615384615385,-0.169230769230769,
-0.153846153846154,-0.138461538461538,-0.123076923076923,-0.107692307692308,
-0.0923076923076923,-0.0769230769230769,-0.0615384615384615,-0.0461538461538462,
-0.0307692307692308,-0.0153846153846154,0.),.UNSPECIFIED.)
CURVE()
GEOMETRIC_REPRESENTATION_ITEM()
RATIONAL_B_SPLINE_CURVE((1.,1.,1.,1.,1.,1.,1.,1.,1.,1.,1.,1.,1.,1.,1.,1.,
1.,1.,1.,1.,1.,1.,1.,1.,1.,1.,1.,1.,1.,1.,1.,1.,1.,1.,1.,1.,1.,1.,1.,1.,
1.,1.,1.,1.,1.,1.,1.,1.,1.,1.,1.,1.,1.,1.,1.,1.,1.,1.,1.,1.,1.,1.,1.,1.,
1.,1.,1.,1.,1.,1.))
REPRESENTATION_ITEM('')
);
#184=(
BOUNDED_CURVE()
B_SPLINE_CURVE(5,(#24092,#24093,#24094,#24095,#24096,#24097,#24098,#24099,
#24100,#24101,#24102,#24103,#24104,#24105,#24106,#24107,#24108,#24109,#24110,
#24111,#24112,#24113,#24114,#24115,#24116,#24117,#24118,#24119,#24120,#24121,
#24122,#24123,#24124,#24125,#24126,#24127,#24128,#24129,#24130,#24131,#24132,
#24133,#24134,#24135,#24136,#24137,#24138,#24139,#24140,#24141,#24142,#24143,
#24144,#24145,#24146,#24147,#24148,#24149,#24150,#24151,#24152,#24153,#24154,
#24155,#24156,#24157,#24158,#24159,#24160,#24161),.UNSPECIFIED.,.F.,.F.)
B_SPLINE_CURVE_WITH_KNOTS((6,1,1,1,1,1,1,1,1,1,1,1,1,1,1,1,1,1,1,1,1,1,
1,1,1,1,1,1,1,1,1,1,1,1,1,1,1,1,1,1,1,1,1,1,1,1,1,1,1,1,1,1,1,1,1,1,1,1,
1,1,1,1,1,1,1,6),(-1.,-0.984615384615383,-0.969230769230768,-0.953846153846152,
-0.938461538461537,-0.923076923076922,-0.907692307692306,-0.892307692307691,
-0.876923076923076,-0.86153846153846,-0.846153846153845,-0.83076923076923,
-0.815384615384614,-0.799999999999999,-0.784615384615384,-0.769230769230768,
-0.753846153846153,-0.738461538461538,-0.723076923076922,-0.707692307692307,
-0.692307692307692,-0.676923076923076,-0.661538461538461,-0.646153846153846,
-0.63076923076923,-0.615384615384615,-0.6,-0.584615384615384,-0.569230769230769,
-0.553846153846154,-0.538461538461538,-0.523076923076923,-0.507692307692308,
-0.492307692307692,-0.476923076923077,-0.461538461538462,-0.446153846153846,
-0.430769230769231,-0.415384615384615,-0.4,-0.384615384615385,-0.369230769230769,
-0.353846153846154,-0.338461538461538,-0.323076923076923,-0.307692307692308,
-0.292307692307692,-0.276923076923077,-0.261538461538462,-0.246153846153846,
-0.230769230769231,-0.215384615384615,-0.2,-0.184615384615385,-0.169230769230769,
-0.153846153846154,-0.138461538461538,-0.123076923076923,-0.107692307692308,
-0.0923076923076923,-0.0769230769230769,-0.0615384615384615,-0.0461538461538462,
-0.0307692307692308,-0.0153846153846154,0.),.UNSPECIFIED.)
CURVE()
GEOMETRIC_REPRESENTATION_ITEM()
RATIONAL_B_SPLINE_CURVE((1.,1.,1.,1.,1.,1.,1.,1.,1.,1.,1.,1.,1.,1.,1.,1.,
1.,1.,1.,1.,1.,1.,1.,1.,1.,1.,1.,1.,1.,1.,1.,1.,1.,1.,1.,1.,1.,1.,1.,1.,
1.,1.,1.,1.,1.,1.,1.,1.,1.,1.,1.,1.,1.,1.,1.,1.,1.,1.,1.,1.,1.,1.,1.,1.,
1.,1.,1.,1.,1.,1.))
REPRESENTATION_ITEM('')
);
#185=(
BOUNDED_CURVE()
B_SPLINE_CURVE(5,(#24308,#24309,#24310,#24311,#24312,#24313,#24314,#24315,
#24316,#24317,#24318,#24319,#24320,#24321,#24322,#24323,#24324,#24325,#24326,
#24327,#24328,#24329,#24330,#24331,#24332,#24333,#24334,#24335,#24336,#24337,
#24338,#24339,#24340,#24341,#24342,#24343,#24344,#24345,#24346,#24347,#24348,
#24349,#24350,#24351,#24352,#24353,#24354,#24355,#24356,#24357,#24358,#24359,
#24360,#24361,#24362,#24363,#24364,#24365,#24366,#24367,#24368,#24369,#24370,
#24371,#24372,#24373,#24374,#24375,#24376,#24377),.UNSPECIFIED.,.F.,.F.)
B_SPLINE_CURVE_WITH_KNOTS((6,1,1,1,1,1,1,1,1,1,1,1,1,1,1,1,1,1,1,1,1,1,
1,1,1,1,1,1,1,1,1,1,1,1,1,1,1,1,1,1,1,1,1,1,1,1,1,1,1,1,1,1,1,1,1,1,1,1,
1,1,1,1,1,1,1,6),(-1.,-0.984615384615383,-0.969230769230768,-0.953846153846152,
-0.938461538461537,-0.923076923076922,-0.907692307692306,-0.892307692307691,
-0.876923076923076,-0.86153846153846,-0.846153846153845,-0.83076923076923,
-0.815384615384614,-0.799999999999999,-0.784615384615384,-0.769230769230768,
-0.753846153846153,-0.738461538461538,-0.723076923076922,-0.707692307692307,
-0.692307692307692,-0.676923076923076,-0.661538461538461,-0.646153846153846,
-0.63076923076923,-0.615384615384615,-0.6,-0.584615384615384,-0.569230769230769,
-0.553846153846154,-0.538461538461538,-0.523076923076923,-0.507692307692308,
-0.492307692307692,-0.476923076923077,-0.461538461538462,-0.446153846153846,
-0.430769230769231,-0.415384615384615,-0.4,-0.384615384615385,-0.369230769230769,
-0.353846153846154,-0.338461538461538,-0.323076923076923,-0.307692307692308,
-0.292307692307692,-0.276923076923077,-0.261538461538462,-0.246153846153846,
-0.230769230769231,-0.215384615384615,-0.2,-0.184615384615385,-0.169230769230769,
-0.153846153846154,-0.138461538461538,-0.123076923076923,-0.107692307692308,
-0.0923076923076923,-0.0769230769230769,-0.0615384615384615,-0.0461538461538462,
-0.0307692307692308,-0.0153846153846154,0.),.UNSPECIFIED.)
CURVE()
GEOMETRIC_REPRESENTATION_ITEM()
RATIONAL_B_SPLINE_CURVE((1.,1.,1.,1.,1.,1.,1.,1.,1.,1.,1.,1.,1.,1.,1.,1.,
1.,1.,1.,1.,1.,1.,1.,1.,1.,1.,1.,1.,1.,1.,1.,1.,1.,1.,1.,1.,1.,1.,1.,1.,
1.,1.,1.,1.,1.,1.,1.,1.,1.,1.,1.,1.,1.,1.,1.,1.,1.,1.,1.,1.,1.,1.,1.,1.,
1.,1.,1.,1.,1.,1.))
REPRESENTATION_ITEM('')
);
#186=(
BOUNDED_CURVE()
B_SPLINE_CURVE(5,(#24524,#24525,#24526,#24527,#24528,#24529,#24530,#24531,
#24532,#24533,#24534,#24535,#24536,#24537,#24538,#24539,#24540,#24541,#24542,
#24543,#24544,#24545,#24546,#24547,#24548,#24549,#24550,#24551,#24552,#24553,
#24554,#24555,#24556,#24557,#24558,#24559,#24560,#24561,#24562,#24563,#24564,
#24565,#24566,#24567,#24568,#24569,#24570,#24571,#24572,#24573,#24574,#24575,
#24576,#24577,#24578,#24579,#24580,#24581,#24582,#24583,#24584,#24585,#24586,
#24587,#24588,#24589,#24590,#24591,#24592,#24593),.UNSPECIFIED.,.F.,.F.)
B_SPLINE_CURVE_WITH_KNOTS((6,1,1,1,1,1,1,1,1,1,1,1,1,1,1,1,1,1,1,1,1,1,
1,1,1,1,1,1,1,1,1,1,1,1,1,1,1,1,1,1,1,1,1,1,1,1,1,1,1,1,1,1,1,1,1,1,1,1,
1,1,1,1,1,1,1,6),(-1.,-0.984615384615383,-0.969230769230768,-0.953846153846152,
-0.938461538461537,-0.923076923076922,-0.907692307692306,-0.892307692307691,
-0.876923076923076,-0.86153846153846,-0.846153846153845,-0.83076923076923,
-0.815384615384614,-0.799999999999999,-0.784615384615384,-0.769230769230768,
-0.753846153846153,-0.738461538461538,-0.723076923076922,-0.707692307692307,
-0.692307692307692,-0.676923076923076,-0.661538461538461,-0.646153846153846,
-0.63076923076923,-0.615384615384615,-0.6,-0.584615384615384,-0.569230769230769,
-0.553846153846154,-0.538461538461538,-0.523076923076923,-0.507692307692308,
-0.492307692307692,-0.476923076923077,-0.461538461538462,-0.446153846153846,
-0.430769230769231,-0.415384615384615,-0.4,-0.384615384615385,-0.369230769230769,
-0.353846153846154,-0.338461538461538,-0.323076923076923,-0.307692307692308,
-0.292307692307692,-0.276923076923077,-0.261538461538462,-0.246153846153846,
-0.230769230769231,-0.215384615384615,-0.2,-0.184615384615385,-0.169230769230769,
-0.153846153846154,-0.138461538461538,-0.123076923076923,-0.107692307692308,
-0.0923076923076923,-0.0769230769230769,-0.0615384615384615,-0.0461538461538462,
-0.0307692307692308,-0.0153846153846154,0.),.UNSPECIFIED.)
CURVE()
GEOMETRIC_REPRESENTATION_ITEM()
RATIONAL_B_SPLINE_CURVE((1.,1.,1.,1.,1.,1.,1.,1.,1.,1.,1.,1.,1.,1.,1.,1.,
1.,1.,1.,1.,1.,1.,1.,1.,1.,1.,1.,1.,1.,1.,1.,1.,1.,1.,1.,1.,1.,1.,1.,1.,
1.,1.,1.,1.,1.,1.,1.,1.,1.,1.,1.,1.,1.,1.,1.,1.,1.,1.,1.,1.,1.,1.,1.,1.,
1.,1.,1.,1.,1.,1.))
REPRESENTATION_ITEM('')
);
#187=(
BOUNDED_CURVE()
B_SPLINE_CURVE(5,(#24740,#24741,#24742,#24743,#24744,#24745,#24746,#24747,
#24748,#24749,#24750,#24751,#24752,#24753,#24754,#24755,#24756,#24757,#24758,
#24759,#24760,#24761,#24762,#24763,#24764,#24765,#24766,#24767,#24768,#24769,
#24770,#24771,#24772,#24773,#24774,#24775,#24776,#24777,#24778,#24779,#24780,
#24781,#24782,#24783,#24784,#24785,#24786,#24787,#24788,#24789,#24790,#24791,
#24792,#24793,#24794,#24795,#24796,#24797,#24798,#24799,#24800,#24801,#24802,
#24803,#24804,#24805,#24806,#24807,#24808,#24809),.UNSPECIFIED.,.F.,.F.)
B_SPLINE_CURVE_WITH_KNOTS((6,1,1,1,1,1,1,1,1,1,1,1,1,1,1,1,1,1,1,1,1,1,
1,1,1,1,1,1,1,1,1,1,1,1,1,1,1,1,1,1,1,1,1,1,1,1,1,1,1,1,1,1,1,1,1,1,1,1,
1,1,1,1,1,1,1,6),(-1.,-0.984615384615383,-0.969230769230768,-0.953846153846152,
-0.938461538461537,-0.923076923076922,-0.907692307692306,-0.892307692307691,
-0.876923076923076,-0.86153846153846,-0.846153846153845,-0.83076923076923,
-0.815384615384614,-0.799999999999999,-0.784615384615384,-0.769230769230768,
-0.753846153846153,-0.738461538461538,-0.723076923076922,-0.707692307692307,
-0.692307692307692,-0.676923076923076,-0.661538461538461,-0.646153846153846,
-0.63076923076923,-0.615384615384615,-0.6,-0.584615384615384,-0.569230769230769,
-0.553846153846154,-0.538461538461538,-0.523076923076923,-0.507692307692308,
-0.492307692307692,-0.476923076923077,-0.461538461538462,-0.446153846153846,
-0.430769230769231,-0.415384615384615,-0.4,-0.384615384615385,-0.369230769230769,
-0.353846153846154,-0.338461538461538,-0.323076923076923,-0.307692307692308,
-0.292307692307692,-0.276923076923077,-0.261538461538462,-0.246153846153846,
-0.230769230769231,-0.215384615384615,-0.2,-0.184615384615385,-0.169230769230769,
-0.153846153846154,-0.138461538461538,-0.123076923076923,-0.107692307692308,
-0.0923076923076923,-0.0769230769230769,-0.0615384615384615,-0.0461538461538462,
-0.0307692307692308,-0.0153846153846154,0.),.UNSPECIFIED.)
CURVE()
GEOMETRIC_REPRESENTATION_ITEM()
RATIONAL_B_SPLINE_CURVE((1.,1.,1.,1.,1.,1.,1.,1.,1.,1.,1.,1.,1.,1.,1.,1.,
1.,1.,1.,1.,1.,1.,1.,1.,1.,1.,1.,1.,1.,1.,1.,1.,1.,1.,1.,1.,1.,1.,1.,1.,
1.,1.,1.,1.,1.,1.,1.,1.,1.,1.,1.,1.,1.,1.,1.,1.,1.,1.,1.,1.,1.,1.,1.,1.,
1.,1.,1.,1.,1.,1.))
REPRESENTATION_ITEM('')
);
#188=(
BOUNDED_CURVE()
B_SPLINE_CURVE(5,(#24956,#24957,#24958,#24959,#24960,#24961,#24962,#24963,
#24964,#24965,#24966,#24967,#24968,#24969,#24970,#24971,#24972,#24973,#24974,
#24975,#24976,#24977,#24978,#24979,#24980,#24981,#24982,#24983,#24984,#24985,
#24986,#24987,#24988,#24989,#24990,#24991,#24992,#24993,#24994,#24995,#24996,
#24997,#24998,#24999,#25000,#25001,#25002,#25003,#25004,#25005,#25006,#25007,
#25008,#25009,#25010,#25011,#25012,#25013,#25014,#25015,#25016,#25017,#25018,
#25019,#25020,#25021,#25022,#25023,#25024,#25025),.UNSPECIFIED.,.F.,.F.)
B_SPLINE_CURVE_WITH_KNOTS((6,1,1,1,1,1,1,1,1,1,1,1,1,1,1,1,1,1,1,1,1,1,
1,1,1,1,1,1,1,1,1,1,1,1,1,1,1,1,1,1,1,1,1,1,1,1,1,1,1,1,1,1,1,1,1,1,1,1,
1,1,1,1,1,1,1,6),(-1.,-0.984615384615383,-0.969230769230768,-0.953846153846152,
-0.938461538461537,-0.923076923076922,-0.907692307692306,-0.892307692307691,
-0.876923076923076,-0.86153846153846,-0.846153846153845,-0.83076923076923,
-0.815384615384614,-0.799999999999999,-0.784615384615384,-0.769230769230768,
-0.753846153846153,-0.738461538461538,-0.723076923076922,-0.707692307692307,
-0.692307692307692,-0.676923076923076,-0.661538461538461,-0.646153846153846,
-0.63076923076923,-0.615384615384615,-0.6,-0.584615384615384,-0.569230769230769,
-0.553846153846154,-0.538461538461538,-0.523076923076923,-0.507692307692308,
-0.492307692307692,-0.476923076923077,-0.461538461538462,-0.446153846153846,
-0.430769230769231,-0.415384615384615,-0.4,-0.384615384615385,-0.369230769230769,
-0.353846153846154,-0.338461538461538,-0.323076923076923,-0.307692307692308,
-0.292307692307692,-0.276923076923077,-0.261538461538462,-0.246153846153846,
-0.230769230769231,-0.215384615384615,-0.2,-0.184615384615385,-0.169230769230769,
-0.153846153846154,-0.138461538461538,-0.123076923076923,-0.107692307692308,
-0.0923076923076923,-0.0769230769230769,-0.0615384615384615,-0.0461538461538462,
-0.0307692307692308,-0.0153846153846154,0.),.UNSPECIFIED.)
CURVE()
GEOMETRIC_REPRESENTATION_ITEM()
RATIONAL_B_SPLINE_CURVE((1.,1.,1.,1.,1.,1.,1.,1.,1.,1.,1.,1.,1.,1.,1.,1.,
1.,1.,1.,1.,1.,1.,1.,1.,1.,1.,1.,1.,1.,1.,1.,1.,1.,1.,1.,1.,1.,1.,1.,1.,
1.,1.,1.,1.,1.,1.,1.,1.,1.,1.,1.,1.,1.,1.,1.,1.,1.,1.,1.,1.,1.,1.,1.,1.,
1.,1.,1.,1.,1.,1.))
REPRESENTATION_ITEM('')
);
#189=(
BOUNDED_CURVE()
B_SPLINE_CURVE(5,(#25172,#25173,#25174,#25175,#25176,#25177,#25178,#25179,
#25180,#25181,#25182,#25183,#25184,#25185,#25186,#25187,#25188,#25189,#25190,
#25191,#25192,#25193,#25194,#25195,#25196,#25197,#25198,#25199,#25200,#25201,
#25202,#25203,#25204,#25205,#25206,#25207,#25208,#25209,#25210,#25211,#25212,
#25213,#25214,#25215,#25216,#25217,#25218,#25219,#25220,#25221,#25222,#25223,
#25224,#25225,#25226,#25227,#25228,#25229,#25230,#25231,#25232,#25233,#25234,
#25235,#25236,#25237,#25238,#25239,#25240,#25241),.UNSPECIFIED.,.F.,.F.)
B_SPLINE_CURVE_WITH_KNOTS((6,1,1,1,1,1,1,1,1,1,1,1,1,1,1,1,1,1,1,1,1,1,
1,1,1,1,1,1,1,1,1,1,1,1,1,1,1,1,1,1,1,1,1,1,1,1,1,1,1,1,1,1,1,1,1,1,1,1,
1,1,1,1,1,1,1,6),(-1.,-0.984615384615383,-0.969230769230768,-0.953846153846152,
-0.938461538461537,-0.923076923076922,-0.907692307692306,-0.892307692307691,
-0.876923076923076,-0.86153846153846,-0.846153846153845,-0.83076923076923,
-0.815384615384614,-0.799999999999999,-0.784615384615384,-0.769230769230768,
-0.753846153846153,-0.738461538461538,-0.723076923076922,-0.707692307692307,
-0.692307692307692,-0.676923076923076,-0.661538461538461,-0.646153846153846,
-0.63076923076923,-0.615384615384615,-0.6,-0.584615384615384,-0.569230769230769,
-0.553846153846154,-0.538461538461538,-0.523076923076923,-0.507692307692308,
-0.492307692307692,-0.476923076923077,-0.461538461538462,-0.446153846153846,
-0.430769230769231,-0.415384615384615,-0.4,-0.384615384615385,-0.369230769230769,
-0.353846153846154,-0.338461538461538,-0.323076923076923,-0.307692307692308,
-0.292307692307692,-0.276923076923077,-0.261538461538462,-0.246153846153846,
-0.230769230769231,-0.215384615384615,-0.2,-0.184615384615385,-0.169230769230769,
-0.153846153846154,-0.138461538461538,-0.123076923076923,-0.107692307692308,
-0.0923076923076923,-0.0769230769230769,-0.0615384615384615,-0.0461538461538462,
-0.0307692307692308,-0.0153846153846154,0.),.UNSPECIFIED.)
CURVE()
GEOMETRIC_REPRESENTATION_ITEM()
RATIONAL_B_SPLINE_CURVE((1.,1.,1.,1.,1.,1.,1.,1.,1.,1.,1.,1.,1.,1.,1.,1.,
1.,1.,1.,1.,1.,1.,1.,1.,1.,1.,1.,1.,1.,1.,1.,1.,1.,1.,1.,1.,1.,1.,1.,1.,
1.,1.,1.,1.,1.,1.,1.,1.,1.,1.,1.,1.,1.,1.,1.,1.,1.,1.,1.,1.,1.,1.,1.,1.,
1.,1.,1.,1.,1.,1.))
REPRESENTATION_ITEM('')
);
#190=(
BOUNDED_CURVE()
B_SPLINE_CURVE(5,(#25388,#25389,#25390,#25391,#25392,#25393,#25394,#25395,
#25396,#25397,#25398,#25399,#25400,#25401,#25402,#25403,#25404,#25405,#25406,
#25407,#25408,#25409,#25410,#25411,#25412,#25413,#25414,#25415,#25416,#25417,
#25418,#25419,#25420,#25421,#25422,#25423,#25424,#25425,#25426,#25427,#25428,
#25429,#25430,#25431,#25432,#25433,#25434,#25435,#25436,#25437,#25438,#25439,
#25440,#25441,#25442,#25443,#25444,#25445,#25446,#25447,#25448,#25449,#25450,
#25451,#25452,#25453,#25454,#25455,#25456,#25457),.UNSPECIFIED.,.F.,.F.)
B_SPLINE_CURVE_WITH_KNOTS((6,1,1,1,1,1,1,1,1,1,1,1,1,1,1,1,1,1,1,1,1,1,
1,1,1,1,1,1,1,1,1,1,1,1,1,1,1,1,1,1,1,1,1,1,1,1,1,1,1,1,1,1,1,1,1,1,1,1,
1,1,1,1,1,1,1,6),(-1.,-0.984615384615383,-0.969230769230768,-0.953846153846152,
-0.938461538461537,-0.923076923076922,-0.907692307692306,-0.892307692307691,
-0.876923076923076,-0.86153846153846,-0.846153846153845,-0.83076923076923,
-0.815384615384614,-0.799999999999999,-0.784615384615384,-0.769230769230768,
-0.753846153846153,-0.738461538461538,-0.723076923076922,-0.707692307692307,
-0.692307692307692,-0.676923076923076,-0.661538461538461,-0.646153846153846,
-0.63076923076923,-0.615384615384615,-0.6,-0.584615384615384,-0.569230769230769,
-0.553846153846154,-0.538461538461538,-0.523076923076923,-0.507692307692308,
-0.492307692307692,-0.476923076923077,-0.461538461538462,-0.446153846153846,
-0.430769230769231,-0.415384615384615,-0.4,-0.384615384615385,-0.369230769230769,
-0.353846153846154,-0.338461538461538,-0.323076923076923,-0.307692307692308,
-0.292307692307692,-0.276923076923077,-0.261538461538462,-0.246153846153846,
-0.230769230769231,-0.215384615384615,-0.2,-0.184615384615385,-0.169230769230769,
-0.153846153846154,-0.138461538461538,-0.123076923076923,-0.107692307692308,
-0.0923076923076923,-0.0769230769230769,-0.0615384615384615,-0.0461538461538462,
-0.0307692307692308,-0.0153846153846154,0.),.UNSPECIFIED.)
CURVE()
GEOMETRIC_REPRESENTATION_ITEM()
RATIONAL_B_SPLINE_CURVE((1.,1.,1.,1.,1.,1.,1.,1.,1.,1.,1.,1.,1.,1.,1.,1.,
1.,1.,1.,1.,1.,1.,1.,1.,1.,1.,1.,1.,1.,1.,1.,1.,1.,1.,1.,1.,1.,1.,1.,1.,
1.,1.,1.,1.,1.,1.,1.,1.,1.,1.,1.,1.,1.,1.,1.,1.,1.,1.,1.,1.,1.,1.,1.,1.,
1.,1.,1.,1.,1.,1.))
REPRESENTATION_ITEM('')
);
#191=(
BOUNDED_CURVE()
B_SPLINE_CURVE(5,(#25604,#25605,#25606,#25607,#25608,#25609,#25610,#25611,
#25612,#25613,#25614,#25615,#25616,#25617,#25618,#25619,#25620,#25621,#25622,
#25623,#25624,#25625,#25626,#25627,#25628,#25629,#25630,#25631,#25632,#25633,
#25634,#25635,#25636,#25637,#25638,#25639,#25640,#25641,#25642,#25643,#25644,
#25645,#25646,#25647,#25648,#25649,#25650,#25651,#25652,#25653,#25654,#25655,
#25656,#25657,#25658,#25659,#25660,#25661,#25662,#25663,#25664,#25665,#25666,
#25667,#25668,#25669,#25670,#25671,#25672,#25673),.UNSPECIFIED.,.F.,.F.)
B_SPLINE_CURVE_WITH_KNOTS((6,1,1,1,1,1,1,1,1,1,1,1,1,1,1,1,1,1,1,1,1,1,
1,1,1,1,1,1,1,1,1,1,1,1,1,1,1,1,1,1,1,1,1,1,1,1,1,1,1,1,1,1,1,1,1,1,1,1,
1,1,1,1,1,1,1,6),(-1.,-0.984615384615383,-0.969230769230768,-0.953846153846152,
-0.938461538461537,-0.923076923076922,-0.907692307692306,-0.892307692307691,
-0.876923076923076,-0.86153846153846,-0.846153846153845,-0.83076923076923,
-0.815384615384614,-0.799999999999999,-0.784615384615384,-0.769230769230768,
-0.753846153846153,-0.738461538461538,-0.723076923076922,-0.707692307692307,
-0.692307692307692,-0.676923076923076,-0.661538461538461,-0.646153846153846,
-0.63076923076923,-0.615384615384615,-0.6,-0.584615384615384,-0.569230769230769,
-0.553846153846154,-0.538461538461538,-0.523076923076923,-0.507692307692308,
-0.492307692307692,-0.476923076923077,-0.461538461538462,-0.446153846153846,
-0.430769230769231,-0.415384615384615,-0.4,-0.384615384615385,-0.369230769230769,
-0.353846153846154,-0.338461538461538,-0.323076923076923,-0.307692307692308,
-0.292307692307692,-0.276923076923077,-0.261538461538462,-0.246153846153846,
-0.230769230769231,-0.215384615384615,-0.2,-0.184615384615385,-0.169230769230769,
-0.153846153846154,-0.138461538461538,-0.123076923076923,-0.107692307692308,
-0.0923076923076923,-0.0769230769230769,-0.0615384615384615,-0.0461538461538462,
-0.0307692307692308,-0.0153846153846154,0.),.UNSPECIFIED.)
CURVE()
GEOMETRIC_REPRESENTATION_ITEM()
RATIONAL_B_SPLINE_CURVE((1.,1.,1.,1.,1.,1.,1.,1.,1.,1.,1.,1.,1.,1.,1.,1.,
1.,1.,1.,1.,1.,1.,1.,1.,1.,1.,1.,1.,1.,1.,1.,1.,1.,1.,1.,1.,1.,1.,1.,1.,
1.,1.,1.,1.,1.,1.,1.,1.,1.,1.,1.,1.,1.,1.,1.,1.,1.,1.,1.,1.,1.,1.,1.,1.,
1.,1.,1.,1.,1.,1.))
REPRESENTATION_ITEM('')
);
#192=(
BOUNDED_CURVE()
B_SPLINE_CURVE(5,(#25820,#25821,#25822,#25823,#25824,#25825,#25826,#25827,
#25828,#25829,#25830,#25831,#25832,#25833,#25834,#25835,#25836,#25837,#25838,
#25839,#25840,#25841,#25842,#25843,#25844,#25845,#25846,#25847,#25848,#25849,
#25850,#25851,#25852,#25853,#25854,#25855,#25856,#25857,#25858,#25859,#25860,
#25861,#25862,#25863,#25864,#25865,#25866,#25867,#25868,#25869,#25870,#25871,
#25872,#25873,#25874,#25875,#25876,#25877,#25878,#25879,#25880,#25881,#25882,
#25883,#25884,#25885,#25886,#25887,#25888,#25889),.UNSPECIFIED.,.F.,.F.)
B_SPLINE_CURVE_WITH_KNOTS((6,1,1,1,1,1,1,1,1,1,1,1,1,1,1,1,1,1,1,1,1,1,
1,1,1,1,1,1,1,1,1,1,1,1,1,1,1,1,1,1,1,1,1,1,1,1,1,1,1,1,1,1,1,1,1,1,1,1,
1,1,1,1,1,1,1,6),(-1.,-0.984615384615383,-0.969230769230768,-0.953846153846152,
-0.938461538461537,-0.923076923076922,-0.907692307692306,-0.892307692307691,
-0.876923076923076,-0.86153846153846,-0.846153846153845,-0.83076923076923,
-0.815384615384614,-0.799999999999999,-0.784615384615384,-0.769230769230768,
-0.753846153846153,-0.738461538461538,-0.723076923076922,-0.707692307692307,
-0.692307692307692,-0.676923076923076,-0.661538461538461,-0.646153846153846,
-0.63076923076923,-0.615384615384615,-0.6,-0.584615384615384,-0.569230769230769,
-0.553846153846154,-0.538461538461538,-0.523076923076923,-0.507692307692308,
-0.492307692307692,-0.476923076923077,-0.461538461538462,-0.446153846153846,
-0.430769230769231,-0.415384615384615,-0.4,-0.384615384615385,-0.369230769230769,
-0.353846153846154,-0.338461538461538,-0.323076923076923,-0.307692307692308,
-0.292307692307692,-0.276923076923077,-0.261538461538462,-0.246153846153846,
-0.230769230769231,-0.215384615384615,-0.2,-0.184615384615385,-0.169230769230769,
-0.153846153846154,-0.138461538461538,-0.123076923076923,-0.107692307692308,
-0.0923076923076923,-0.0769230769230769,-0.0615384615384615,-0.0461538461538462,
-0.0307692307692308,-0.0153846153846154,0.),.UNSPECIFIED.)
CURVE()
GEOMETRIC_REPRESENTATION_ITEM()
RATIONAL_B_SPLINE_CURVE((1.,1.,1.,1.,1.,1.,1.,1.,1.,1.,1.,1.,1.,1.,1.,1.,
1.,1.,1.,1.,1.,1.,1.,1.,1.,1.,1.,1.,1.,1.,1.,1.,1.,1.,1.,1.,1.,1.,1.,1.,
1.,1.,1.,1.,1.,1.,1.,1.,1.,1.,1.,1.,1.,1.,1.,1.,1.,1.,1.,1.,1.,1.,1.,1.,
1.,1.,1.,1.,1.,1.))
REPRESENTATION_ITEM('')
);
#193=(
BOUNDED_CURVE()
B_SPLINE_CURVE(5,(#26036,#26037,#26038,#26039,#26040,#26041,#26042,#26043,
#26044,#26045,#26046,#26047,#26048,#26049,#26050,#26051,#26052,#26053,#26054,
#26055,#26056,#26057,#26058,#26059,#26060,#26061,#26062,#26063,#26064,#26065,
#26066,#26067,#26068,#26069,#26070,#26071,#26072,#26073,#26074,#26075,#26076,
#26077,#26078,#26079,#26080,#26081,#26082,#26083,#26084,#26085,#26086,#26087,
#26088,#26089,#26090,#26091,#26092,#26093,#26094,#26095,#26096,#26097,#26098,
#26099,#26100,#26101,#26102,#26103,#26104,#26105),.UNSPECIFIED.,.F.,.F.)
B_SPLINE_CURVE_WITH_KNOTS((6,1,1,1,1,1,1,1,1,1,1,1,1,1,1,1,1,1,1,1,1,1,
1,1,1,1,1,1,1,1,1,1,1,1,1,1,1,1,1,1,1,1,1,1,1,1,1,1,1,1,1,1,1,1,1,1,1,1,
1,1,1,1,1,1,1,6),(-1.,-0.984615384615383,-0.969230769230768,-0.953846153846152,
-0.938461538461537,-0.923076923076922,-0.907692307692306,-0.892307692307691,
-0.876923076923076,-0.86153846153846,-0.846153846153845,-0.83076923076923,
-0.815384615384614,-0.799999999999999,-0.784615384615384,-0.769230769230768,
-0.753846153846153,-0.738461538461538,-0.723076923076922,-0.707692307692307,
-0.692307692307692,-0.676923076923076,-0.661538461538461,-0.646153846153846,
-0.63076923076923,-0.615384615384615,-0.6,-0.584615384615384,-0.569230769230769,
-0.553846153846154,-0.538461538461538,-0.523076923076923,-0.507692307692308,
-0.492307692307692,-0.476923076923077,-0.461538461538462,-0.446153846153846,
-0.430769230769231,-0.415384615384615,-0.4,-0.384615384615385,-0.369230769230769,
-0.353846153846154,-0.338461538461538,-0.323076923076923,-0.307692307692308,
-0.292307692307692,-0.276923076923077,-0.261538461538462,-0.246153846153846,
-0.230769230769231,-0.215384615384615,-0.2,-0.184615384615385,-0.169230769230769,
-0.153846153846154,-0.138461538461538,-0.123076923076923,-0.107692307692308,
-0.0923076923076923,-0.0769230769230769,-0.0615384615384615,-0.0461538461538462,
-0.0307692307692308,-0.0153846153846154,0.),.UNSPECIFIED.)
CURVE()
GEOMETRIC_REPRESENTATION_ITEM()
RATIONAL_B_SPLINE_CURVE((1.,1.,1.,1.,1.,1.,1.,1.,1.,1.,1.,1.,1.,1.,1.,1.,
1.,1.,1.,1.,1.,1.,1.,1.,1.,1.,1.,1.,1.,1.,1.,1.,1.,1.,1.,1.,1.,1.,1.,1.,
1.,1.,1.,1.,1.,1.,1.,1.,1.,1.,1.,1.,1.,1.,1.,1.,1.,1.,1.,1.,1.,1.,1.,1.,
1.,1.,1.,1.,1.,1.))
REPRESENTATION_ITEM('')
);
#194=(
BOUNDED_CURVE()
B_SPLINE_CURVE(5,(#26252,#26253,#26254,#26255,#26256,#26257,#26258,#26259,
#26260,#26261,#26262,#26263,#26264,#26265,#26266,#26267,#26268,#26269,#26270,
#26271,#26272,#26273,#26274,#26275,#26276,#26277,#26278,#26279,#26280,#26281,
#26282,#26283,#26284,#26285,#26286,#26287,#26288,#26289,#26290,#26291,#26292,
#26293,#26294,#26295,#26296,#26297,#26298,#26299,#26300,#26301,#26302,#26303,
#26304,#26305,#26306,#26307,#26308,#26309,#26310,#26311,#26312,#26313,#26314,
#26315,#26316,#26317,#26318,#26319,#26320,#26321),.UNSPECIFIED.,.F.,.F.)
B_SPLINE_CURVE_WITH_KNOTS((6,1,1,1,1,1,1,1,1,1,1,1,1,1,1,1,1,1,1,1,1,1,
1,1,1,1,1,1,1,1,1,1,1,1,1,1,1,1,1,1,1,1,1,1,1,1,1,1,1,1,1,1,1,1,1,1,1,1,
1,1,1,1,1,1,1,6),(-1.,-0.984615384615383,-0.969230769230768,-0.953846153846152,
-0.938461538461537,-0.923076923076922,-0.907692307692306,-0.892307692307691,
-0.876923076923076,-0.86153846153846,-0.846153846153845,-0.83076923076923,
-0.815384615384614,-0.799999999999999,-0.784615384615384,-0.769230769230768,
-0.753846153846153,-0.738461538461538,-0.723076923076922,-0.707692307692307,
-0.692307692307692,-0.676923076923076,-0.661538461538461,-0.646153846153846,
-0.63076923076923,-0.615384615384615,-0.6,-0.584615384615384,-0.569230769230769,
-0.553846153846154,-0.538461538461538,-0.523076923076923,-0.507692307692308,
-0.492307692307692,-0.476923076923077,-0.461538461538462,-0.446153846153846,
-0.430769230769231,-0.415384615384615,-0.4,-0.384615384615385,-0.369230769230769,
-0.353846153846154,-0.338461538461538,-0.323076923076923,-0.307692307692308,
-0.292307692307692,-0.276923076923077,-0.261538461538462,-0.246153846153846,
-0.230769230769231,-0.215384615384615,-0.2,-0.184615384615385,-0.169230769230769,
-0.153846153846154,-0.138461538461538,-0.123076923076923,-0.107692307692308,
-0.0923076923076923,-0.0769230769230769,-0.0615384615384615,-0.0461538461538462,
-0.0307692307692308,-0.0153846153846154,0.),.UNSPECIFIED.)
CURVE()
GEOMETRIC_REPRESENTATION_ITEM()
RATIONAL_B_SPLINE_CURVE((1.,1.,1.,1.,1.,1.,1.,1.,1.,1.,1.,1.,1.,1.,1.,1.,
1.,1.,1.,1.,1.,1.,1.,1.,1.,1.,1.,1.,1.,1.,1.,1.,1.,1.,1.,1.,1.,1.,1.,1.,
1.,1.,1.,1.,1.,1.,1.,1.,1.,1.,1.,1.,1.,1.,1.,1.,1.,1.,1.,1.,1.,1.,1.,1.,
1.,1.,1.,1.,1.,1.))
REPRESENTATION_ITEM('')
);
#195=(
BOUNDED_CURVE()
B_SPLINE_CURVE(5,(#26468,#26469,#26470,#26471,#26472,#26473,#26474,#26475,
#26476,#26477,#26478,#26479,#26480,#26481,#26482,#26483,#26484,#26485,#26486,
#26487,#26488,#26489,#26490,#26491,#26492,#26493,#26494,#26495,#26496,#26497,
#26498,#26499,#26500,#26501,#26502,#26503,#26504,#26505,#26506,#26507,#26508,
#26509,#26510,#26511,#26512,#26513,#26514,#26515,#26516,#26517,#26518,#26519,
#26520,#26521,#26522,#26523,#26524,#26525,#26526,#26527,#26528,#26529,#26530,
#26531,#26532,#26533,#26534,#26535,#26536,#26537),.UNSPECIFIED.,.F.,.F.)
B_SPLINE_CURVE_WITH_KNOTS((6,1,1,1,1,1,1,1,1,1,1,1,1,1,1,1,1,1,1,1,1,1,
1,1,1,1,1,1,1,1,1,1,1,1,1,1,1,1,1,1,1,1,1,1,1,1,1,1,1,1,1,1,1,1,1,1,1,1,
1,1,1,1,1,1,1,6),(-1.,-0.984615384615383,-0.969230769230768,-0.953846153846152,
-0.938461538461537,-0.923076923076922,-0.907692307692306,-0.892307692307691,
-0.876923076923076,-0.86153846153846,-0.846153846153845,-0.83076923076923,
-0.815384615384614,-0.799999999999999,-0.784615384615384,-0.769230769230768,
-0.753846153846153,-0.738461538461538,-0.723076923076922,-0.707692307692307,
-0.692307692307692,-0.676923076923076,-0.661538461538461,-0.646153846153846,
-0.63076923076923,-0.615384615384615,-0.6,-0.584615384615384,-0.569230769230769,
-0.553846153846154,-0.538461538461538,-0.523076923076923,-0.507692307692308,
-0.492307692307692,-0.476923076923077,-0.461538461538462,-0.446153846153846,
-0.430769230769231,-0.415384615384615,-0.4,-0.384615384615385,-0.369230769230769,
-0.353846153846154,-0.338461538461538,-0.323076923076923,-0.307692307692308,
-0.292307692307692,-0.276923076923077,-0.261538461538462,-0.246153846153846,
-0.230769230769231,-0.215384615384615,-0.2,-0.184615384615385,-0.169230769230769,
-0.153846153846154,-0.138461538461538,-0.123076923076923,-0.107692307692308,
-0.0923076923076923,-0.0769230769230769,-0.0615384615384615,-0.0461538461538462,
-0.0307692307692308,-0.0153846153846154,0.),.UNSPECIFIED.)
CURVE()
GEOMETRIC_REPRESENTATION_ITEM()
RATIONAL_B_SPLINE_CURVE((1.,1.,1.,1.,1.,1.,1.,1.,1.,1.,1.,1.,1.,1.,1.,1.,
1.,1.,1.,1.,1.,1.,1.,1.,1.,1.,1.,1.,1.,1.,1.,1.,1.,1.,1.,1.,1.,1.,1.,1.,
1.,1.,1.,1.,1.,1.,1.,1.,1.,1.,1.,1.,1.,1.,1.,1.,1.,1.,1.,1.,1.,1.,1.,1.,
1.,1.,1.,1.,1.,1.))
REPRESENTATION_ITEM('')
);
#196=(
BOUNDED_CURVE()
B_SPLINE_CURVE(5,(#26684,#26685,#26686,#26687,#26688,#26689,#26690,#26691,
#26692,#26693,#26694,#26695,#26696,#26697,#26698,#26699,#26700,#26701,#26702,
#26703,#26704,#26705,#26706,#26707,#26708,#26709,#26710,#26711,#26712,#26713,
#26714,#26715,#26716,#26717,#26718,#26719,#26720,#26721,#26722,#26723,#26724,
#26725,#26726,#26727,#26728,#26729,#26730,#26731,#26732,#26733,#26734,#26735,
#26736,#26737,#26738,#26739,#26740,#26741,#26742,#26743,#26744,#26745,#26746,
#26747,#26748,#26749,#26750,#26751,#26752,#26753),.UNSPECIFIED.,.F.,.F.)
B_SPLINE_CURVE_WITH_KNOTS((6,1,1,1,1,1,1,1,1,1,1,1,1,1,1,1,1,1,1,1,1,1,
1,1,1,1,1,1,1,1,1,1,1,1,1,1,1,1,1,1,1,1,1,1,1,1,1,1,1,1,1,1,1,1,1,1,1,1,
1,1,1,1,1,1,1,6),(-1.,-0.984615384615383,-0.969230769230768,-0.953846153846152,
-0.938461538461537,-0.923076923076922,-0.907692307692306,-0.892307692307691,
-0.876923076923076,-0.86153846153846,-0.846153846153845,-0.83076923076923,
-0.815384615384614,-0.799999999999999,-0.784615384615384,-0.769230769230768,
-0.753846153846153,-0.738461538461538,-0.723076923076922,-0.707692307692307,
-0.692307692307692,-0.676923076923076,-0.661538461538461,-0.646153846153846,
-0.63076923076923,-0.615384615384615,-0.6,-0.584615384615384,-0.569230769230769,
-0.553846153846154,-0.538461538461538,-0.523076923076923,-0.507692307692308,
-0.492307692307692,-0.476923076923077,-0.461538461538462,-0.446153846153846,
-0.430769230769231,-0.415384615384615,-0.4,-0.384615384615385,-0.369230769230769,
-0.353846153846154,-0.338461538461538,-0.323076923076923,-0.307692307692308,
-0.292307692307692,-0.276923076923077,-0.261538461538462,-0.246153846153846,
-0.230769230769231,-0.215384615384615,-0.2,-0.184615384615385,-0.169230769230769,
-0.153846153846154,-0.138461538461538,-0.123076923076923,-0.107692307692308,
-0.0923076923076923,-0.0769230769230769,-0.0615384615384615,-0.0461538461538462,
-0.0307692307692308,-0.0153846153846154,0.),.UNSPECIFIED.)
CURVE()
GEOMETRIC_REPRESENTATION_ITEM()
RATIONAL_B_SPLINE_CURVE((1.,1.,1.,1.,1.,1.,1.,1.,1.,1.,1.,1.,1.,1.,1.,1.,
1.,1.,1.,1.,1.,1.,1.,1.,1.,1.,1.,1.,1.,1.,1.,1.,1.,1.,1.,1.,1.,1.,1.,1.,
1.,1.,1.,1.,1.,1.,1.,1.,1.,1.,1.,1.,1.,1.,1.,1.,1.,1.,1.,1.,1.,1.,1.,1.,
1.,1.,1.,1.,1.,1.))
REPRESENTATION_ITEM('')
);
#197=(
BOUNDED_CURVE()
B_SPLINE_CURVE(5,(#26900,#26901,#26902,#26903,#26904,#26905,#26906,#26907,
#26908,#26909,#26910,#26911,#26912,#26913,#26914,#26915,#26916,#26917,#26918,
#26919,#26920,#26921,#26922,#26923,#26924,#26925,#26926,#26927,#26928,#26929,
#26930,#26931,#26932,#26933,#26934,#26935,#26936,#26937,#26938,#26939,#26940,
#26941,#26942,#26943,#26944,#26945,#26946,#26947,#26948,#26949,#26950,#26951,
#26952,#26953,#26954,#26955,#26956,#26957,#26958,#26959,#26960,#26961,#26962,
#26963,#26964,#26965,#26966,#26967,#26968,#26969),.UNSPECIFIED.,.F.,.F.)
B_SPLINE_CURVE_WITH_KNOTS((6,1,1,1,1,1,1,1,1,1,1,1,1,1,1,1,1,1,1,1,1,1,
1,1,1,1,1,1,1,1,1,1,1,1,1,1,1,1,1,1,1,1,1,1,1,1,1,1,1,1,1,1,1,1,1,1,1,1,
1,1,1,1,1,1,1,6),(-1.,-0.984615384615383,-0.969230769230768,-0.953846153846152,
-0.938461538461537,-0.923076923076922,-0.907692307692306,-0.892307692307691,
-0.876923076923076,-0.86153846153846,-0.846153846153845,-0.83076923076923,
-0.815384615384614,-0.799999999999999,-0.784615384615384,-0.769230769230768,
-0.753846153846153,-0.738461538461538,-0.723076923076922,-0.707692307692307,
-0.692307692307692,-0.676923076923076,-0.661538461538461,-0.646153846153846,
-0.63076923076923,-0.615384615384615,-0.6,-0.584615384615384,-0.569230769230769,
-0.553846153846154,-0.538461538461538,-0.523076923076923,-0.507692307692308,
-0.492307692307692,-0.476923076923077,-0.461538461538462,-0.446153846153846,
-0.430769230769231,-0.415384615384615,-0.4,-0.384615384615385,-0.369230769230769,
-0.353846153846154,-0.338461538461538,-0.323076923076923,-0.307692307692308,
-0.292307692307692,-0.276923076923077,-0.261538461538462,-0.246153846153846,
-0.230769230769231,-0.215384615384615,-0.2,-0.184615384615385,-0.169230769230769,
-0.153846153846154,-0.138461538461538,-0.123076923076923,-0.107692307692308,
-0.0923076923076923,-0.0769230769230769,-0.0615384615384615,-0.0461538461538462,
-0.0307692307692308,-0.0153846153846154,0.),.UNSPECIFIED.)
CURVE()
GEOMETRIC_REPRESENTATION_ITEM()
RATIONAL_B_SPLINE_CURVE((1.,1.,1.,1.,1.,1.,1.,1.,1.,1.,1.,1.,1.,1.,1.,1.,
1.,1.,1.,1.,1.,1.,1.,1.,1.,1.,1.,1.,1.,1.,1.,1.,1.,1.,1.,1.,1.,1.,1.,1.,
1.,1.,1.,1.,1.,1.,1.,1.,1.,1.,1.,1.,1.,1.,1.,1.,1.,1.,1.,1.,1.,1.,1.,1.,
1.,1.,1.,1.,1.,1.))
REPRESENTATION_ITEM('')
);
#198=(
BOUNDED_CURVE()
B_SPLINE_CURVE(5,(#27116,#27117,#27118,#27119,#27120,#27121,#27122,#27123,
#27124,#27125,#27126,#27127,#27128,#27129,#27130,#27131,#27132,#27133,#27134,
#27135,#27136,#27137,#27138,#27139,#27140,#27141,#27142,#27143,#27144,#27145,
#27146,#27147,#27148,#27149,#27150,#27151,#27152,#27153,#27154,#27155,#27156,
#27157,#27158,#27159,#27160,#27161,#27162,#27163,#27164,#27165,#27166,#27167,
#27168,#27169,#27170,#27171,#27172,#27173,#27174,#27175,#27176,#27177,#27178,
#27179,#27180,#27181,#27182,#27183,#27184,#27185),.UNSPECIFIED.,.F.,.F.)
B_SPLINE_CURVE_WITH_KNOTS((6,1,1,1,1,1,1,1,1,1,1,1,1,1,1,1,1,1,1,1,1,1,
1,1,1,1,1,1,1,1,1,1,1,1,1,1,1,1,1,1,1,1,1,1,1,1,1,1,1,1,1,1,1,1,1,1,1,1,
1,1,1,1,1,1,1,6),(-1.,-0.984615384615383,-0.969230769230768,-0.953846153846152,
-0.938461538461537,-0.923076923076922,-0.907692307692306,-0.892307692307691,
-0.876923076923076,-0.86153846153846,-0.846153846153845,-0.83076923076923,
-0.815384615384614,-0.799999999999999,-0.784615384615384,-0.769230769230768,
-0.753846153846153,-0.738461538461538,-0.723076923076922,-0.707692307692307,
-0.692307692307692,-0.676923076923076,-0.661538461538461,-0.646153846153846,
-0.63076923076923,-0.615384615384615,-0.6,-0.584615384615384,-0.569230769230769,
-0.553846153846154,-0.538461538461538,-0.523076923076923,-0.507692307692308,
-0.492307692307692,-0.476923076923077,-0.461538461538462,-0.446153846153846,
-0.430769230769231,-0.415384615384615,-0.4,-0.384615384615385,-0.369230769230769,
-0.353846153846154,-0.338461538461538,-0.323076923076923,-0.307692307692308,
-0.292307692307692,-0.276923076923077,-0.261538461538462,-0.246153846153846,
-0.230769230769231,-0.215384615384615,-0.2,-0.184615384615385,-0.169230769230769,
-0.153846153846154,-0.138461538461538,-0.123076923076923,-0.107692307692308,
-0.0923076923076923,-0.0769230769230769,-0.0615384615384615,-0.0461538461538462,
-0.0307692307692308,-0.0153846153846154,0.),.UNSPECIFIED.)
CURVE()
GEOMETRIC_REPRESENTATION_ITEM()
RATIONAL_B_SPLINE_CURVE((1.,1.,1.,1.,1.,1.,1.,1.,1.,1.,1.,1.,1.,1.,1.,1.,
1.,1.,1.,1.,1.,1.,1.,1.,1.,1.,1.,1.,1.,1.,1.,1.,1.,1.,1.,1.,1.,1.,1.,1.,
1.,1.,1.,1.,1.,1.,1.,1.,1.,1.,1.,1.,1.,1.,1.,1.,1.,1.,1.,1.,1.,1.,1.,1.,
1.,1.,1.,1.,1.,1.))
REPRESENTATION_ITEM('')
);
#199=(
BOUNDED_CURVE()
B_SPLINE_CURVE(5,(#27332,#27333,#27334,#27335,#27336,#27337,#27338,#27339,
#27340,#27341,#27342,#27343,#27344,#27345,#27346,#27347,#27348,#27349,#27350,
#27351,#27352,#27353,#27354,#27355,#27356,#27357,#27358,#27359,#27360,#27361,
#27362,#27363,#27364,#27365,#27366,#27367,#27368,#27369,#27370,#27371,#27372,
#27373,#27374,#27375,#27376,#27377,#27378,#27379,#27380,#27381,#27382,#27383,
#27384,#27385,#27386,#27387,#27388,#27389,#27390,#27391,#27392,#27393,#27394,
#27395,#27396,#27397,#27398,#27399,#27400,#27401),.UNSPECIFIED.,.F.,.F.)
B_SPLINE_CURVE_WITH_KNOTS((6,1,1,1,1,1,1,1,1,1,1,1,1,1,1,1,1,1,1,1,1,1,
1,1,1,1,1,1,1,1,1,1,1,1,1,1,1,1,1,1,1,1,1,1,1,1,1,1,1,1,1,1,1,1,1,1,1,1,
1,1,1,1,1,1,1,6),(-1.,-0.984615384615383,-0.969230769230768,-0.953846153846152,
-0.938461538461537,-0.923076923076922,-0.907692307692306,-0.892307692307691,
-0.876923076923076,-0.86153846153846,-0.846153846153845,-0.83076923076923,
-0.815384615384614,-0.799999999999999,-0.784615384615384,-0.769230769230768,
-0.753846153846153,-0.738461538461538,-0.723076923076922,-0.707692307692307,
-0.692307692307692,-0.676923076923076,-0.661538461538461,-0.646153846153846,
-0.63076923076923,-0.615384615384615,-0.6,-0.584615384615384,-0.569230769230769,
-0.553846153846154,-0.538461538461538,-0.523076923076923,-0.507692307692308,
-0.492307692307692,-0.476923076923077,-0.461538461538462,-0.446153846153846,
-0.430769230769231,-0.415384615384615,-0.4,-0.384615384615385,-0.369230769230769,
-0.353846153846154,-0.338461538461538,-0.323076923076923,-0.307692307692308,
-0.292307692307692,-0.276923076923077,-0.261538461538462,-0.246153846153846,
-0.230769230769231,-0.215384615384615,-0.2,-0.184615384615385,-0.169230769230769,
-0.153846153846154,-0.138461538461538,-0.123076923076923,-0.107692307692308,
-0.0923076923076923,-0.0769230769230769,-0.0615384615384615,-0.0461538461538462,
-0.0307692307692308,-0.0153846153846154,0.),.UNSPECIFIED.)
CURVE()
GEOMETRIC_REPRESENTATION_ITEM()
RATIONAL_B_SPLINE_CURVE((1.,1.,1.,1.,1.,1.,1.,1.,1.,1.,1.,1.,1.,1.,1.,1.,
1.,1.,1.,1.,1.,1.,1.,1.,1.,1.,1.,1.,1.,1.,1.,1.,1.,1.,1.,1.,1.,1.,1.,1.,
1.,1.,1.,1.,1.,1.,1.,1.,1.,1.,1.,1.,1.,1.,1.,1.,1.,1.,1.,1.,1.,1.,1.,1.,
1.,1.,1.,1.,1.,1.))
REPRESENTATION_ITEM('')
);
#200=(
BOUNDED_CURVE()
B_SPLINE_CURVE(5,(#27548,#27549,#27550,#27551,#27552,#27553,#27554,#27555,
#27556,#27557,#27558,#27559,#27560,#27561,#27562,#27563,#27564,#27565,#27566,
#27567,#27568,#27569,#27570,#27571,#27572,#27573,#27574,#27575,#27576,#27577,
#27578,#27579,#27580,#27581,#27582,#27583,#27584,#27585,#27586,#27587,#27588,
#27589,#27590,#27591,#27592,#27593,#27594,#27595,#27596,#27597,#27598,#27599,
#27600,#27601,#27602,#27603,#27604,#27605,#27606,#27607,#27608,#27609,#27610,
#27611,#27612,#27613,#27614,#27615,#27616,#27617),.UNSPECIFIED.,.F.,.F.)
B_SPLINE_CURVE_WITH_KNOTS((6,1,1,1,1,1,1,1,1,1,1,1,1,1,1,1,1,1,1,1,1,1,
1,1,1,1,1,1,1,1,1,1,1,1,1,1,1,1,1,1,1,1,1,1,1,1,1,1,1,1,1,1,1,1,1,1,1,1,
1,1,1,1,1,1,1,6),(-1.,-0.984615384615383,-0.969230769230768,-0.953846153846152,
-0.938461538461537,-0.923076923076922,-0.907692307692306,-0.892307692307691,
-0.876923076923076,-0.86153846153846,-0.846153846153845,-0.83076923076923,
-0.815384615384614,-0.799999999999999,-0.784615384615384,-0.769230769230768,
-0.753846153846153,-0.738461538461538,-0.723076923076922,-0.707692307692307,
-0.692307692307692,-0.676923076923076,-0.661538461538461,-0.646153846153846,
-0.63076923076923,-0.615384615384615,-0.6,-0.584615384615384,-0.569230769230769,
-0.553846153846154,-0.538461538461538,-0.523076923076923,-0.507692307692308,
-0.492307692307692,-0.476923076923077,-0.461538461538462,-0.446153846153846,
-0.430769230769231,-0.415384615384615,-0.4,-0.384615384615385,-0.369230769230769,
-0.353846153846154,-0.338461538461538,-0.323076923076923,-0.307692307692308,
-0.292307692307692,-0.276923076923077,-0.261538461538462,-0.246153846153846,
-0.230769230769231,-0.215384615384615,-0.2,-0.184615384615385,-0.169230769230769,
-0.153846153846154,-0.138461538461538,-0.123076923076923,-0.107692307692308,
-0.0923076923076923,-0.0769230769230769,-0.0615384615384615,-0.0461538461538462,
-0.0307692307692308,-0.0153846153846154,0.),.UNSPECIFIED.)
CURVE()
GEOMETRIC_REPRESENTATION_ITEM()
RATIONAL_B_SPLINE_CURVE((1.,1.,1.,1.,1.,1.,1.,1.,1.,1.,1.,1.,1.,1.,1.,1.,
1.,1.,1.,1.,1.,1.,1.,1.,1.,1.,1.,1.,1.,1.,1.,1.,1.,1.,1.,1.,1.,1.,1.,1.,
1.,1.,1.,1.,1.,1.,1.,1.,1.,1.,1.,1.,1.,1.,1.,1.,1.,1.,1.,1.,1.,1.,1.,1.,
1.,1.,1.,1.,1.,1.))
REPRESENTATION_ITEM('')
);
#201=(
BOUNDED_CURVE()
B_SPLINE_CURVE(5,(#27764,#27765,#27766,#27767,#27768,#27769,#27770,#27771,
#27772,#27773,#27774,#27775,#27776,#27777,#27778,#27779,#27780,#27781,#27782,
#27783,#27784,#27785,#27786,#27787,#27788,#27789,#27790,#27791,#27792,#27793,
#27794,#27795,#27796,#27797,#27798,#27799,#27800,#27801,#27802,#27803,#27804,
#27805,#27806,#27807,#27808,#27809,#27810,#27811,#27812,#27813,#27814,#27815,
#27816,#27817,#27818,#27819,#27820,#27821,#27822,#27823,#27824,#27825,#27826,
#27827,#27828,#27829,#27830,#27831,#27832,#27833),.UNSPECIFIED.,.F.,.F.)
B_SPLINE_CURVE_WITH_KNOTS((6,1,1,1,1,1,1,1,1,1,1,1,1,1,1,1,1,1,1,1,1,1,
1,1,1,1,1,1,1,1,1,1,1,1,1,1,1,1,1,1,1,1,1,1,1,1,1,1,1,1,1,1,1,1,1,1,1,1,
1,1,1,1,1,1,1,6),(-1.,-0.984615384615383,-0.969230769230768,-0.953846153846152,
-0.938461538461537,-0.923076923076922,-0.907692307692306,-0.892307692307691,
-0.876923076923076,-0.86153846153846,-0.846153846153845,-0.83076923076923,
-0.815384615384614,-0.799999999999999,-0.784615384615384,-0.769230769230768,
-0.753846153846153,-0.738461538461538,-0.723076923076922,-0.707692307692307,
-0.692307692307692,-0.676923076923076,-0.661538461538461,-0.646153846153846,
-0.63076923076923,-0.615384615384615,-0.6,-0.584615384615384,-0.569230769230769,
-0.553846153846154,-0.538461538461538,-0.523076923076923,-0.507692307692308,
-0.492307692307692,-0.476923076923077,-0.461538461538462,-0.446153846153846,
-0.430769230769231,-0.415384615384615,-0.4,-0.384615384615385,-0.369230769230769,
-0.353846153846154,-0.338461538461538,-0.323076923076923,-0.307692307692308,
-0.292307692307692,-0.276923076923077,-0.261538461538462,-0.246153846153846,
-0.230769230769231,-0.215384615384615,-0.2,-0.184615384615385,-0.169230769230769,
-0.153846153846154,-0.138461538461538,-0.123076923076923,-0.107692307692308,
-0.0923076923076923,-0.0769230769230769,-0.0615384615384615,-0.0461538461538462,
-0.0307692307692308,-0.0153846153846154,0.),.UNSPECIFIED.)
CURVE()
GEOMETRIC_REPRESENTATION_ITEM()
RATIONAL_B_SPLINE_CURVE((1.,1.,1.,1.,1.,1.,1.,1.,1.,1.,1.,1.,1.,1.,1.,1.,
1.,1.,1.,1.,1.,1.,1.,1.,1.,1.,1.,1.,1.,1.,1.,1.,1.,1.,1.,1.,1.,1.,1.,1.,
1.,1.,1.,1.,1.,1.,1.,1.,1.,1.,1.,1.,1.,1.,1.,1.,1.,1.,1.,1.,1.,1.,1.,1.,
1.,1.,1.,1.,1.,1.))
REPRESENTATION_ITEM('')
);
#202=(
BOUNDED_CURVE()
B_SPLINE_CURVE(5,(#27980,#27981,#27982,#27983,#27984,#27985,#27986,#27987,
#27988,#27989,#27990,#27991,#27992,#27993,#27994,#27995,#27996,#27997,#27998,
#27999,#28000,#28001,#28002,#28003,#28004,#28005,#28006,#28007,#28008,#28009,
#28010,#28011,#28012,#28013,#28014,#28015,#28016,#28017,#28018,#28019,#28020,
#28021,#28022,#28023,#28024,#28025,#28026,#28027,#28028,#28029,#28030,#28031,
#28032,#28033,#28034,#28035,#28036,#28037,#28038,#28039,#28040,#28041,#28042,
#28043,#28044,#28045,#28046,#28047,#28048,#28049),.UNSPECIFIED.,.F.,.F.)
B_SPLINE_CURVE_WITH_KNOTS((6,1,1,1,1,1,1,1,1,1,1,1,1,1,1,1,1,1,1,1,1,1,
1,1,1,1,1,1,1,1,1,1,1,1,1,1,1,1,1,1,1,1,1,1,1,1,1,1,1,1,1,1,1,1,1,1,1,1,
1,1,1,1,1,1,1,6),(-1.,-0.984615384615383,-0.969230769230768,-0.953846153846152,
-0.938461538461537,-0.923076923076922,-0.907692307692306,-0.892307692307691,
-0.876923076923076,-0.86153846153846,-0.846153846153845,-0.83076923076923,
-0.815384615384614,-0.799999999999999,-0.784615384615384,-0.769230769230768,
-0.753846153846153,-0.738461538461538,-0.723076923076922,-0.707692307692307,
-0.692307692307692,-0.676923076923076,-0.661538461538461,-0.646153846153846,
-0.63076923076923,-0.615384615384615,-0.6,-0.584615384615384,-0.569230769230769,
-0.553846153846154,-0.538461538461538,-0.523076923076923,-0.507692307692308,
-0.492307692307692,-0.476923076923077,-0.461538461538462,-0.446153846153846,
-0.430769230769231,-0.415384615384615,-0.4,-0.384615384615385,-0.369230769230769,
-0.353846153846154,-0.338461538461538,-0.323076923076923,-0.307692307692308,
-0.292307692307692,-0.276923076923077,-0.261538461538462,-0.246153846153846,
-0.230769230769231,-0.215384615384615,-0.2,-0.184615384615385,-0.169230769230769,
-0.153846153846154,-0.138461538461538,-0.123076923076923,-0.107692307692308,
-0.0923076923076923,-0.0769230769230769,-0.0615384615384615,-0.0461538461538462,
-0.0307692307692308,-0.0153846153846154,0.),.UNSPECIFIED.)
CURVE()
GEOMETRIC_REPRESENTATION_ITEM()
RATIONAL_B_SPLINE_CURVE((1.,1.,1.,1.,1.,1.,1.,1.,1.,1.,1.,1.,1.,1.,1.,1.,
1.,1.,1.,1.,1.,1.,1.,1.,1.,1.,1.,1.,1.,1.,1.,1.,1.,1.,1.,1.,1.,1.,1.,1.,
1.,1.,1.,1.,1.,1.,1.,1.,1.,1.,1.,1.,1.,1.,1.,1.,1.,1.,1.,1.,1.,1.,1.,1.,
1.,1.,1.,1.,1.,1.))
REPRESENTATION_ITEM('')
);
#203=(
BOUNDED_CURVE()
B_SPLINE_CURVE(5,(#28196,#28197,#28198,#28199,#28200,#28201,#28202,#28203,
#28204,#28205,#28206,#28207,#28208,#28209,#28210,#28211,#28212,#28213,#28214,
#28215,#28216,#28217,#28218,#28219,#28220,#28221,#28222,#28223,#28224,#28225,
#28226,#28227,#28228,#28229,#28230,#28231,#28232,#28233,#28234,#28235,#28236,
#28237,#28238,#28239,#28240,#28241,#28242,#28243,#28244,#28245,#28246,#28247,
#28248,#28249,#28250,#28251,#28252,#28253,#28254,#28255,#28256,#28257,#28258,
#28259,#28260,#28261,#28262,#28263,#28264,#28265),.UNSPECIFIED.,.F.,.F.)
B_SPLINE_CURVE_WITH_KNOTS((6,1,1,1,1,1,1,1,1,1,1,1,1,1,1,1,1,1,1,1,1,1,
1,1,1,1,1,1,1,1,1,1,1,1,1,1,1,1,1,1,1,1,1,1,1,1,1,1,1,1,1,1,1,1,1,1,1,1,
1,1,1,1,1,1,1,6),(-1.,-0.984615384615383,-0.969230769230768,-0.953846153846152,
-0.938461538461537,-0.923076923076922,-0.907692307692306,-0.892307692307691,
-0.876923076923076,-0.86153846153846,-0.846153846153845,-0.83076923076923,
-0.815384615384614,-0.799999999999999,-0.784615384615384,-0.769230769230768,
-0.753846153846153,-0.738461538461538,-0.723076923076922,-0.707692307692307,
-0.692307692307692,-0.676923076923076,-0.661538461538461,-0.646153846153846,
-0.63076923076923,-0.615384615384615,-0.6,-0.584615384615384,-0.569230769230769,
-0.553846153846154,-0.538461538461538,-0.523076923076923,-0.507692307692308,
-0.492307692307692,-0.476923076923077,-0.461538461538462,-0.446153846153846,
-0.430769230769231,-0.415384615384615,-0.4,-0.384615384615385,-0.369230769230769,
-0.353846153846154,-0.338461538461538,-0.323076923076923,-0.307692307692308,
-0.292307692307692,-0.276923076923077,-0.261538461538462,-0.246153846153846,
-0.230769230769231,-0.215384615384615,-0.2,-0.184615384615385,-0.169230769230769,
-0.153846153846154,-0.138461538461538,-0.123076923076923,-0.107692307692308,
-0.0923076923076923,-0.0769230769230769,-0.0615384615384615,-0.0461538461538462,
-0.0307692307692308,-0.0153846153846154,0.),.UNSPECIFIED.)
CURVE()
GEOMETRIC_REPRESENTATION_ITEM()
RATIONAL_B_SPLINE_CURVE((1.,1.,1.,1.,1.,1.,1.,1.,1.,1.,1.,1.,1.,1.,1.,1.,
1.,1.,1.,1.,1.,1.,1.,1.,1.,1.,1.,1.,1.,1.,1.,1.,1.,1.,1.,1.,1.,1.,1.,1.,
1.,1.,1.,1.,1.,1.,1.,1.,1.,1.,1.,1.,1.,1.,1.,1.,1.,1.,1.,1.,1.,1.,1.,1.,
1.,1.,1.,1.,1.,1.))
REPRESENTATION_ITEM('')
);
#204=(
BOUNDED_CURVE()
B_SPLINE_CURVE(5,(#28412,#28413,#28414,#28415,#28416,#28417,#28418,#28419,
#28420,#28421,#28422,#28423,#28424,#28425,#28426,#28427,#28428,#28429,#28430,
#28431,#28432,#28433,#28434,#28435,#28436,#28437,#28438,#28439,#28440,#28441,
#28442,#28443,#28444,#28445,#28446,#28447,#28448,#28449,#28450,#28451,#28452,
#28453,#28454,#28455,#28456,#28457,#28458,#28459,#28460,#28461,#28462,#28463,
#28464,#28465,#28466,#28467,#28468,#28469,#28470,#28471,#28472,#28473,#28474,
#28475,#28476,#28477,#28478,#28479,#28480,#28481),.UNSPECIFIED.,.F.,.F.)
B_SPLINE_CURVE_WITH_KNOTS((6,1,1,1,1,1,1,1,1,1,1,1,1,1,1,1,1,1,1,1,1,1,
1,1,1,1,1,1,1,1,1,1,1,1,1,1,1,1,1,1,1,1,1,1,1,1,1,1,1,1,1,1,1,1,1,1,1,1,
1,1,1,1,1,1,1,6),(-1.,-0.984615384615383,-0.969230769230768,-0.953846153846152,
-0.938461538461537,-0.923076923076922,-0.907692307692306,-0.892307692307691,
-0.876923076923076,-0.86153846153846,-0.846153846153845,-0.83076923076923,
-0.815384615384614,-0.799999999999999,-0.784615384615384,-0.769230769230768,
-0.753846153846153,-0.738461538461538,-0.723076923076922,-0.707692307692307,
-0.692307692307692,-0.676923076923076,-0.661538461538461,-0.646153846153846,
-0.63076923076923,-0.615384615384615,-0.6,-0.584615384615384,-0.569230769230769,
-0.553846153846154,-0.538461538461538,-0.523076923076923,-0.507692307692308,
-0.492307692307692,-0.476923076923077,-0.461538461538462,-0.446153846153846,
-0.430769230769231,-0.415384615384615,-0.4,-0.384615384615385,-0.369230769230769,
-0.353846153846154,-0.338461538461538,-0.323076923076923,-0.307692307692308,
-0.292307692307692,-0.276923076923077,-0.261538461538462,-0.246153846153846,
-0.230769230769231,-0.215384615384615,-0.2,-0.184615384615385,-0.169230769230769,
-0.153846153846154,-0.138461538461538,-0.123076923076923,-0.107692307692308,
-0.0923076923076923,-0.0769230769230769,-0.0615384615384615,-0.0461538461538462,
-0.0307692307692308,-0.0153846153846154,0.),.UNSPECIFIED.)
CURVE()
GEOMETRIC_REPRESENTATION_ITEM()
RATIONAL_B_SPLINE_CURVE((1.,1.,1.,1.,1.,1.,1.,1.,1.,1.,1.,1.,1.,1.,1.,1.,
1.,1.,1.,1.,1.,1.,1.,1.,1.,1.,1.,1.,1.,1.,1.,1.,1.,1.,1.,1.,1.,1.,1.,1.,
1.,1.,1.,1.,1.,1.,1.,1.,1.,1.,1.,1.,1.,1.,1.,1.,1.,1.,1.,1.,1.,1.,1.,1.,
1.,1.,1.,1.,1.,1.))
REPRESENTATION_ITEM('')
);
#205=(
BOUNDED_CURVE()
B_SPLINE_CURVE(5,(#28628,#28629,#28630,#28631,#28632,#28633,#28634,#28635,
#28636,#28637,#28638,#28639,#28640,#28641,#28642,#28643,#28644,#28645,#28646,
#28647,#28648,#28649,#28650,#28651,#28652,#28653,#28654,#28655,#28656,#28657,
#28658,#28659,#28660,#28661,#28662,#28663,#28664,#28665,#28666,#28667,#28668,
#28669,#28670,#28671,#28672,#28673,#28674,#28675,#28676,#28677,#28678,#28679,
#28680,#28681,#28682,#28683,#28684,#28685,#28686,#28687,#28688,#28689,#28690,
#28691,#28692,#28693,#28694,#28695,#28696,#28697),.UNSPECIFIED.,.F.,.F.)
B_SPLINE_CURVE_WITH_KNOTS((6,1,1,1,1,1,1,1,1,1,1,1,1,1,1,1,1,1,1,1,1,1,
1,1,1,1,1,1,1,1,1,1,1,1,1,1,1,1,1,1,1,1,1,1,1,1,1,1,1,1,1,1,1,1,1,1,1,1,
1,1,1,1,1,1,1,6),(-1.,-0.984615384615383,-0.969230769230768,-0.953846153846152,
-0.938461538461537,-0.923076923076922,-0.907692307692306,-0.892307692307691,
-0.876923076923076,-0.86153846153846,-0.846153846153845,-0.83076923076923,
-0.815384615384614,-0.799999999999999,-0.784615384615384,-0.769230769230768,
-0.753846153846153,-0.738461538461538,-0.723076923076922,-0.707692307692307,
-0.692307692307692,-0.676923076923076,-0.661538461538461,-0.646153846153846,
-0.63076923076923,-0.615384615384615,-0.6,-0.584615384615384,-0.569230769230769,
-0.553846153846154,-0.538461538461538,-0.523076923076923,-0.507692307692308,
-0.492307692307692,-0.476923076923077,-0.461538461538462,-0.446153846153846,
-0.430769230769231,-0.415384615384615,-0.4,-0.384615384615385,-0.369230769230769,
-0.353846153846154,-0.338461538461538,-0.323076923076923,-0.307692307692308,
-0.292307692307692,-0.276923076923077,-0.261538461538462,-0.246153846153846,
-0.230769230769231,-0.215384615384615,-0.2,-0.184615384615385,-0.169230769230769,
-0.153846153846154,-0.138461538461538,-0.123076923076923,-0.107692307692308,
-0.0923076923076923,-0.0769230769230769,-0.0615384615384615,-0.0461538461538462,
-0.0307692307692308,-0.0153846153846154,0.),.UNSPECIFIED.)
CURVE()
GEOMETRIC_REPRESENTATION_ITEM()
RATIONAL_B_SPLINE_CURVE((1.,1.,1.,1.,1.,1.,1.,1.,1.,1.,1.,1.,1.,1.,1.,1.,
1.,1.,1.,1.,1.,1.,1.,1.,1.,1.,1.,1.,1.,1.,1.,1.,1.,1.,1.,1.,1.,1.,1.,1.,
1.,1.,1.,1.,1.,1.,1.,1.,1.,1.,1.,1.,1.,1.,1.,1.,1.,1.,1.,1.,1.,1.,1.,1.,
1.,1.,1.,1.,1.,1.))
REPRESENTATION_ITEM('')
);
#206=(
BOUNDED_CURVE()
B_SPLINE_CURVE(5,(#28844,#28845,#28846,#28847,#28848,#28849,#28850,#28851,
#28852,#28853,#28854,#28855,#28856,#28857,#28858,#28859,#28860,#28861,#28862,
#28863,#28864,#28865,#28866,#28867,#28868,#28869,#28870,#28871,#28872,#28873,
#28874,#28875,#28876,#28877,#28878,#28879,#28880,#28881,#28882,#28883,#28884,
#28885,#28886,#28887,#28888,#28889,#28890,#28891,#28892,#28893,#28894,#28895,
#28896,#28897,#28898,#28899,#28900,#28901,#28902,#28903,#28904,#28905,#28906,
#28907,#28908,#28909,#28910,#28911,#28912,#28913),.UNSPECIFIED.,.F.,.F.)
B_SPLINE_CURVE_WITH_KNOTS((6,1,1,1,1,1,1,1,1,1,1,1,1,1,1,1,1,1,1,1,1,1,
1,1,1,1,1,1,1,1,1,1,1,1,1,1,1,1,1,1,1,1,1,1,1,1,1,1,1,1,1,1,1,1,1,1,1,1,
1,1,1,1,1,1,1,6),(-1.,-0.984615384615383,-0.969230769230768,-0.953846153846152,
-0.938461538461537,-0.923076923076922,-0.907692307692306,-0.892307692307691,
-0.876923076923076,-0.86153846153846,-0.846153846153845,-0.83076923076923,
-0.815384615384614,-0.799999999999999,-0.784615384615384,-0.769230769230768,
-0.753846153846153,-0.738461538461538,-0.723076923076922,-0.707692307692307,
-0.692307692307692,-0.676923076923076,-0.661538461538461,-0.646153846153846,
-0.63076923076923,-0.615384615384615,-0.6,-0.584615384615384,-0.569230769230769,
-0.553846153846154,-0.538461538461538,-0.523076923076923,-0.507692307692308,
-0.492307692307692,-0.476923076923077,-0.461538461538462,-0.446153846153846,
-0.430769230769231,-0.415384615384615,-0.4,-0.384615384615385,-0.369230769230769,
-0.353846153846154,-0.338461538461538,-0.323076923076923,-0.307692307692308,
-0.292307692307692,-0.276923076923077,-0.261538461538462,-0.246153846153846,
-0.230769230769231,-0.215384615384615,-0.2,-0.184615384615385,-0.169230769230769,
-0.153846153846154,-0.138461538461538,-0.123076923076923,-0.107692307692308,
-0.0923076923076923,-0.0769230769230769,-0.0615384615384615,-0.0461538461538462,
-0.0307692307692308,-0.0153846153846154,0.),.UNSPECIFIED.)
CURVE()
GEOMETRIC_REPRESENTATION_ITEM()
RATIONAL_B_SPLINE_CURVE((1.,1.,1.,1.,1.,1.,1.,1.,1.,1.,1.,1.,1.,1.,1.,1.,
1.,1.,1.,1.,1.,1.,1.,1.,1.,1.,1.,1.,1.,1.,1.,1.,1.,1.,1.,1.,1.,1.,1.,1.,
1.,1.,1.,1.,1.,1.,1.,1.,1.,1.,1.,1.,1.,1.,1.,1.,1.,1.,1.,1.,1.,1.,1.,1.,
1.,1.,1.,1.,1.,1.))
REPRESENTATION_ITEM('')
);
#207=(
BOUNDED_CURVE()
B_SPLINE_CURVE(5,(#29060,#29061,#29062,#29063,#29064,#29065,#29066,#29067,
#29068,#29069,#29070,#29071,#29072,#29073,#29074,#29075,#29076,#29077,#29078,
#29079,#29080,#29081,#29082,#29083,#29084,#29085,#29086,#29087,#29088,#29089,
#29090,#29091,#29092,#29093,#29094,#29095,#29096,#29097,#29098,#29099,#29100,
#29101,#29102,#29103,#29104,#29105,#29106,#29107,#29108,#29109,#29110,#29111,
#29112,#29113,#29114,#29115,#29116,#29117,#29118,#29119,#29120,#29121,#29122,
#29123,#29124,#29125,#29126,#29127,#29128,#29129),.UNSPECIFIED.,.F.,.F.)
B_SPLINE_CURVE_WITH_KNOTS((6,1,1,1,1,1,1,1,1,1,1,1,1,1,1,1,1,1,1,1,1,1,
1,1,1,1,1,1,1,1,1,1,1,1,1,1,1,1,1,1,1,1,1,1,1,1,1,1,1,1,1,1,1,1,1,1,1,1,
1,1,1,1,1,1,1,6),(-1.,-0.984615384615383,-0.969230769230768,-0.953846153846152,
-0.938461538461537,-0.923076923076922,-0.907692307692306,-0.892307692307691,
-0.876923076923076,-0.86153846153846,-0.846153846153845,-0.83076923076923,
-0.815384615384614,-0.799999999999999,-0.784615384615384,-0.769230769230768,
-0.753846153846153,-0.738461538461538,-0.723076923076922,-0.707692307692307,
-0.692307692307692,-0.676923076923076,-0.661538461538461,-0.646153846153846,
-0.63076923076923,-0.615384615384615,-0.6,-0.584615384615384,-0.569230769230769,
-0.553846153846154,-0.538461538461538,-0.523076923076923,-0.507692307692308,
-0.492307692307692,-0.476923076923077,-0.461538461538462,-0.446153846153846,
-0.430769230769231,-0.415384615384615,-0.4,-0.384615384615385,-0.369230769230769,
-0.353846153846154,-0.338461538461538,-0.323076923076923,-0.307692307692308,
-0.292307692307692,-0.276923076923077,-0.261538461538462,-0.246153846153846,
-0.230769230769231,-0.215384615384615,-0.2,-0.184615384615385,-0.169230769230769,
-0.153846153846154,-0.138461538461538,-0.123076923076923,-0.107692307692308,
-0.0923076923076923,-0.0769230769230769,-0.0615384615384615,-0.0461538461538462,
-0.0307692307692308,-0.0153846153846154,0.),.UNSPECIFIED.)
CURVE()
GEOMETRIC_REPRESENTATION_ITEM()
RATIONAL_B_SPLINE_CURVE((1.,1.,1.,1.,1.,1.,1.,1.,1.,1.,1.,1.,1.,1.,1.,1.,
1.,1.,1.,1.,1.,1.,1.,1.,1.,1.,1.,1.,1.,1.,1.,1.,1.,1.,1.,1.,1.,1.,1.,1.,
1.,1.,1.,1.,1.,1.,1.,1.,1.,1.,1.,1.,1.,1.,1.,1.,1.,1.,1.,1.,1.,1.,1.,1.,
1.,1.,1.,1.,1.,1.))
REPRESENTATION_ITEM('')
);
#208=(
BOUNDED_CURVE()
B_SPLINE_CURVE(5,(#29276,#29277,#29278,#29279,#29280,#29281,#29282,#29283,
#29284,#29285,#29286,#29287,#29288,#29289,#29290,#29291,#29292,#29293,#29294,
#29295,#29296,#29297,#29298,#29299,#29300,#29301,#29302,#29303,#29304,#29305,
#29306,#29307,#29308,#29309,#29310,#29311,#29312,#29313,#29314,#29315,#29316,
#29317,#29318,#29319,#29320,#29321,#29322,#29323,#29324,#29325,#29326,#29327,
#29328,#29329,#29330,#29331,#29332,#29333,#29334,#29335,#29336,#29337,#29338,
#29339,#29340,#29341,#29342,#29343,#29344,#29345),.UNSPECIFIED.,.F.,.F.)
B_SPLINE_CURVE_WITH_KNOTS((6,1,1,1,1,1,1,1,1,1,1,1,1,1,1,1,1,1,1,1,1,1,
1,1,1,1,1,1,1,1,1,1,1,1,1,1,1,1,1,1,1,1,1,1,1,1,1,1,1,1,1,1,1,1,1,1,1,1,
1,1,1,1,1,1,1,6),(-1.,-0.984615384615383,-0.969230769230768,-0.953846153846152,
-0.938461538461537,-0.923076923076922,-0.907692307692306,-0.892307692307691,
-0.876923076923076,-0.86153846153846,-0.846153846153845,-0.83076923076923,
-0.815384615384614,-0.799999999999999,-0.784615384615384,-0.769230769230768,
-0.753846153846153,-0.738461538461538,-0.723076923076922,-0.707692307692307,
-0.692307692307692,-0.676923076923076,-0.661538461538461,-0.646153846153846,
-0.63076923076923,-0.615384615384615,-0.6,-0.584615384615384,-0.569230769230769,
-0.553846153846154,-0.538461538461538,-0.523076923076923,-0.507692307692308,
-0.492307692307692,-0.476923076923077,-0.461538461538462,-0.446153846153846,
-0.430769230769231,-0.415384615384615,-0.4,-0.384615384615385,-0.369230769230769,
-0.353846153846154,-0.338461538461538,-0.323076923076923,-0.307692307692308,
-0.292307692307692,-0.276923076923077,-0.261538461538462,-0.246153846153846,
-0.230769230769231,-0.215384615384615,-0.2,-0.184615384615385,-0.169230769230769,
-0.153846153846154,-0.138461538461538,-0.123076923076923,-0.107692307692308,
-0.0923076923076923,-0.0769230769230769,-0.0615384615384615,-0.0461538461538462,
-0.0307692307692308,-0.0153846153846154,0.),.UNSPECIFIED.)
CURVE()
GEOMETRIC_REPRESENTATION_ITEM()
RATIONAL_B_SPLINE_CURVE((1.,1.,1.,1.,1.,1.,1.,1.,1.,1.,1.,1.,1.,1.,1.,1.,
1.,1.,1.,1.,1.,1.,1.,1.,1.,1.,1.,1.,1.,1.,1.,1.,1.,1.,1.,1.,1.,1.,1.,1.,
1.,1.,1.,1.,1.,1.,1.,1.,1.,1.,1.,1.,1.,1.,1.,1.,1.,1.,1.,1.,1.,1.,1.,1.,
1.,1.,1.,1.,1.,1.))
REPRESENTATION_ITEM('')
);
#209=(
BOUNDED_CURVE()
B_SPLINE_CURVE(5,(#29492,#29493,#29494,#29495,#29496,#29497,#29498,#29499,
#29500,#29501,#29502,#29503,#29504,#29505,#29506,#29507,#29508,#29509,#29510,
#29511,#29512,#29513,#29514,#29515,#29516,#29517,#29518,#29519,#29520,#29521,
#29522,#29523,#29524,#29525,#29526,#29527,#29528,#29529,#29530,#29531,#29532,
#29533,#29534,#29535,#29536,#29537,#29538,#29539,#29540,#29541,#29542,#29543,
#29544,#29545,#29546,#29547,#29548,#29549,#29550,#29551,#29552,#29553,#29554,
#29555,#29556,#29557,#29558,#29559,#29560,#29561),.UNSPECIFIED.,.F.,.F.)
B_SPLINE_CURVE_WITH_KNOTS((6,1,1,1,1,1,1,1,1,1,1,1,1,1,1,1,1,1,1,1,1,1,
1,1,1,1,1,1,1,1,1,1,1,1,1,1,1,1,1,1,1,1,1,1,1,1,1,1,1,1,1,1,1,1,1,1,1,1,
1,1,1,1,1,1,1,6),(-1.,-0.984615384615383,-0.969230769230768,-0.953846153846152,
-0.938461538461537,-0.923076923076922,-0.907692307692306,-0.892307692307691,
-0.876923076923076,-0.86153846153846,-0.846153846153845,-0.83076923076923,
-0.815384615384614,-0.799999999999999,-0.784615384615384,-0.769230769230768,
-0.753846153846153,-0.738461538461538,-0.723076923076922,-0.707692307692307,
-0.692307692307692,-0.676923076923076,-0.661538461538461,-0.646153846153846,
-0.63076923076923,-0.615384615384615,-0.6,-0.584615384615384,-0.569230769230769,
-0.553846153846154,-0.538461538461538,-0.523076923076923,-0.507692307692308,
-0.492307692307692,-0.476923076923077,-0.461538461538462,-0.446153846153846,
-0.430769230769231,-0.415384615384615,-0.4,-0.384615384615385,-0.369230769230769,
-0.353846153846154,-0.338461538461538,-0.323076923076923,-0.307692307692308,
-0.292307692307692,-0.276923076923077,-0.261538461538462,-0.246153846153846,
-0.230769230769231,-0.215384615384615,-0.2,-0.184615384615385,-0.169230769230769,
-0.153846153846154,-0.138461538461538,-0.123076923076923,-0.107692307692308,
-0.0923076923076923,-0.0769230769230769,-0.0615384615384615,-0.0461538461538462,
-0.0307692307692308,-0.0153846153846154,0.),.UNSPECIFIED.)
CURVE()
GEOMETRIC_REPRESENTATION_ITEM()
RATIONAL_B_SPLINE_CURVE((1.,1.,1.,1.,1.,1.,1.,1.,1.,1.,1.,1.,1.,1.,1.,1.,
1.,1.,1.,1.,1.,1.,1.,1.,1.,1.,1.,1.,1.,1.,1.,1.,1.,1.,1.,1.,1.,1.,1.,1.,
1.,1.,1.,1.,1.,1.,1.,1.,1.,1.,1.,1.,1.,1.,1.,1.,1.,1.,1.,1.,1.,1.,1.,1.,
1.,1.,1.,1.,1.,1.))
REPRESENTATION_ITEM('')
);
#210=(
BOUNDED_CURVE()
B_SPLINE_CURVE(5,(#29708,#29709,#29710,#29711,#29712,#29713,#29714,#29715,
#29716,#29717,#29718,#29719,#29720,#29721,#29722,#29723,#29724,#29725,#29726,
#29727,#29728,#29729,#29730,#29731,#29732,#29733,#29734,#29735,#29736,#29737,
#29738,#29739,#29740,#29741,#29742,#29743,#29744,#29745,#29746,#29747,#29748,
#29749,#29750,#29751,#29752,#29753,#29754,#29755,#29756,#29757,#29758,#29759,
#29760,#29761,#29762,#29763,#29764,#29765,#29766,#29767,#29768,#29769,#29770,
#29771,#29772,#29773,#29774,#29775,#29776,#29777),.UNSPECIFIED.,.F.,.F.)
B_SPLINE_CURVE_WITH_KNOTS((6,1,1,1,1,1,1,1,1,1,1,1,1,1,1,1,1,1,1,1,1,1,
1,1,1,1,1,1,1,1,1,1,1,1,1,1,1,1,1,1,1,1,1,1,1,1,1,1,1,1,1,1,1,1,1,1,1,1,
1,1,1,1,1,1,1,6),(-1.,-0.984615384615383,-0.969230769230768,-0.953846153846152,
-0.938461538461537,-0.923076923076922,-0.907692307692306,-0.892307692307691,
-0.876923076923076,-0.86153846153846,-0.846153846153845,-0.83076923076923,
-0.815384615384614,-0.799999999999999,-0.784615384615384,-0.769230769230768,
-0.753846153846153,-0.738461538461538,-0.723076923076922,-0.707692307692307,
-0.692307692307692,-0.676923076923076,-0.661538461538461,-0.646153846153846,
-0.63076923076923,-0.615384615384615,-0.6,-0.584615384615384,-0.569230769230769,
-0.553846153846154,-0.538461538461538,-0.523076923076923,-0.507692307692308,
-0.492307692307692,-0.476923076923077,-0.461538461538462,-0.446153846153846,
-0.430769230769231,-0.415384615384615,-0.4,-0.384615384615385,-0.369230769230769,
-0.353846153846154,-0.338461538461538,-0.323076923076923,-0.307692307692308,
-0.292307692307692,-0.276923076923077,-0.261538461538462,-0.246153846153846,
-0.230769230769231,-0.215384615384615,-0.2,-0.184615384615385,-0.169230769230769,
-0.153846153846154,-0.138461538461538,-0.123076923076923,-0.107692307692308,
-0.0923076923076923,-0.0769230769230769,-0.0615384615384615,-0.0461538461538462,
-0.0307692307692308,-0.0153846153846154,0.),.UNSPECIFIED.)
CURVE()
GEOMETRIC_REPRESENTATION_ITEM()
RATIONAL_B_SPLINE_CURVE((1.,1.,1.,1.,1.,1.,1.,1.,1.,1.,1.,1.,1.,1.,1.,1.,
1.,1.,1.,1.,1.,1.,1.,1.,1.,1.,1.,1.,1.,1.,1.,1.,1.,1.,1.,1.,1.,1.,1.,1.,
1.,1.,1.,1.,1.,1.,1.,1.,1.,1.,1.,1.,1.,1.,1.,1.,1.,1.,1.,1.,1.,1.,1.,1.,
1.,1.,1.,1.,1.,1.))
REPRESENTATION_ITEM('')
);
#211=(
BOUNDED_CURVE()
B_SPLINE_CURVE(5,(#30153,#30154,#30155,#30156,#30157,#30158,#30159,#30160,
#30161,#30162,#30163,#30164,#30165,#30166,#30167,#30168,#30169,#30170,#30171,
#30172,#30173,#30174,#30175,#30176,#30177,#30178,#30179,#30180,#30181,#30182,
#30183,#30184,#30185,#30186,#30187,#30188,#30189,#30190,#30191,#30192,#30193,
#30194,#30195,#30196,#30197,#30198,#30199,#30200,#30201,#30202,#30203,#30204,
#30205,#30206,#30207,#30208,#30209,#30210,#30211,#30212,#30213,#30214,#30215,
#30216,#30217,#30218,#30219,#30220,#30221,#30222),.UNSPECIFIED.,.F.,.F.)
B_SPLINE_CURVE_WITH_KNOTS((6,1,1,1,1,1,1,1,1,1,1,1,1,1,1,1,1,1,1,1,1,1,
1,1,1,1,1,1,1,1,1,1,1,1,1,1,1,1,1,1,1,1,1,1,1,1,1,1,1,1,1,1,1,1,1,1,1,1,
1,1,1,1,1,1,1,6),(0.00577184337450058,0.0153846153846154,0.0307692307692308,
0.0461538461538462,0.0615384615384615,0.0769230769230769,0.0923076923076923,
0.107692307692308,0.123076923076923,0.138461538461538,0.153846153846154,
0.169230769230769,0.184615384615385,0.2,0.215384615384615,0.230769230769231,
0.246153846153846,0.261538461538462,0.276923076923077,0.292307692307692,
0.307692307692308,0.323076923076923,0.338461538461538,0.353846153846154,
0.369230769230769,0.384615384615385,0.4,0.415384615384615,0.430769230769231,
0.446153846153846,0.461538461538462,0.476923076923077,0.492307692307692,
0.507692307692308,0.523076923076923,0.538461538461538,0.553846153846154,
0.569230769230769,0.584615384615384,0.6,0.615384615384615,0.63076923076923,
0.646153846153846,0.661538461538461,0.676923076923076,0.692307692307692,
0.707692307692307,0.723076923076922,0.738461538461538,0.753846153846153,
0.769230769230768,0.784615384615384,0.799999999999999,0.815384615384614,
0.83076923076923,0.846153846153845,0.86153846153846,0.876923076923076,0.892307692307691,
0.907692307692306,0.923076923076922,0.938461538461537,0.953846153846152,
0.969230769230768,0.984615384615383,1.),.UNSPECIFIED.)
CURVE()
GEOMETRIC_REPRESENTATION_ITEM()
RATIONAL_B_SPLINE_CURVE((1.,1.,1.,1.,1.,1.,1.,1.,1.,1.,1.,1.,1.,1.,1.,1.,
1.,1.,1.,1.,1.,1.,1.,1.,1.,1.,1.,1.,1.,1.,1.,1.,1.,1.,1.,1.,1.,1.,1.,1.,
1.,1.,1.,1.,1.,1.,1.,1.,1.,1.,1.,1.,1.,1.,1.,1.,1.,1.,1.,1.,1.,1.,1.,1.,
1.,1.,1.,1.,1.,1.))
REPRESENTATION_ITEM('')
);
#212=(
BOUNDED_CURVE()
B_SPLINE_CURVE(5,(#30226,#30227,#30228,#30229,#30230,#30231,#30232,#30233,
#30234,#30235,#30236,#30237,#30238,#30239,#30240,#30241,#30242,#30243,#30244,
#30245,#30246,#30247,#30248,#30249,#30250,#30251,#30252,#30253,#30254,#30255,
#30256,#30257,#30258,#30259,#30260,#30261,#30262,#30263,#30264,#30265,#30266,
#30267,#30268,#30269,#30270,#30271,#30272,#30273,#30274,#30275,#30276,#30277,
#30278,#30279,#30280,#30281,#30282,#30283,#30284,#30285,#30286,#30287,#30288,
#30289,#30290,#30291,#30292,#30293,#30294,#30295),.UNSPECIFIED.,.F.,.F.)
B_SPLINE_CURVE_WITH_KNOTS((6,1,1,1,1,1,1,1,1,1,1,1,1,1,1,1,1,1,1,1,1,1,
1,1,1,1,1,1,1,1,1,1,1,1,1,1,1,1,1,1,1,1,1,1,1,1,1,1,1,1,1,1,1,1,1,1,1,1,
1,1,1,1,1,1,1,6),(0.,0.0153846153846154,0.0307692307692308,0.0461538461538462,
0.0615384615384615,0.0769230769230769,0.0923076923076923,0.107692307692308,
0.123076923076923,0.138461538461538,0.153846153846154,0.169230769230769,
0.184615384615385,0.2,0.215384615384615,0.230769230769231,0.246153846153846,
0.261538461538462,0.276923076923077,0.292307692307692,0.307692307692308,
0.323076923076923,0.338461538461538,0.353846153846154,0.369230769230769,
0.384615384615385,0.4,0.415384615384615,0.430769230769231,0.446153846153846,
0.461538461538462,0.476923076923077,0.492307692307692,0.507692307692308,
0.523076923076923,0.538461538461538,0.553846153846154,0.569230769230769,
0.584615384615384,0.6,0.615384615384615,0.63076923076923,0.646153846153846,
0.661538461538461,0.676923076923076,0.692307692307692,0.707692307692307,
0.723076923076922,0.738461538461538,0.753846153846153,0.769230769230768,
0.784615384615384,0.799999999999999,0.815384615384614,0.83076923076923,
0.846153846153845,0.86153846153846,0.876923076923076,0.892307692307691,
0.907692307692306,0.923076923076922,0.938461538461537,0.953846153846152,
0.969230769230768,0.984615384615383,0.994228156739708),.UNSPECIFIED.)
CURVE()
GEOMETRIC_REPRESENTATION_ITEM()
RATIONAL_B_SPLINE_CURVE((1.,1.,1.,1.,1.,1.,1.,1.,1.,1.,1.,1.,1.,1.,1.,1.,
1.,1.,1.,1.,1.,1.,1.,1.,1.,1.,1.,1.,1.,1.,1.,1.,1.,1.,1.,1.,1.,1.,1.,1.,
1.,1.,1.,1.,1.,1.,1.,1.,1.,1.,1.,1.,1.,1.,1.,1.,1.,1.,1.,1.,1.,1.,1.,1.,
1.,1.,1.,1.,1.,1.))
REPRESENTATION_ITEM('')
);
#213=(
BOUNDED_CURVE()
B_SPLINE_CURVE(5,(#30299,#30300,#30301,#30302,#30303,#30304,#30305,#30306,
#30307,#30308,#30309,#30310,#30311,#30312,#30313,#30314,#30315,#30316,#30317,
#30318,#30319,#30320,#30321,#30322,#30323,#30324,#30325,#30326,#30327,#30328,
#30329,#30330,#30331,#30332,#30333,#30334,#30335,#30336,#30337,#30338,#30339,
#30340,#30341,#30342,#30343,#30344,#30345,#30346,#30347,#30348,#30349,#30350,
#30351,#30352,#30353,#30354,#30355,#30356,#30357,#30358,#30359,#30360,#30361,
#30362,#30363,#30364,#30365,#30366,#30367,#30368),.UNSPECIFIED.,.F.,.F.)
B_SPLINE_CURVE_WITH_KNOTS((6,1,1,1,1,1,1,1,1,1,1,1,1,1,1,1,1,1,1,1,1,1,
1,1,1,1,1,1,1,1,1,1,1,1,1,1,1,1,1,1,1,1,1,1,1,1,1,1,1,1,1,1,1,1,1,1,1,1,
1,1,1,1,1,1,1,6),(0.0057718433745091,0.0153846153846154,0.0307692307692308,
0.0461538461538462,0.0615384615384615,0.0769230769230769,0.0923076923076923,
0.107692307692308,0.123076923076923,0.138461538461538,0.153846153846154,
0.169230769230769,0.184615384615385,0.2,0.215384615384615,0.230769230769231,
0.246153846153846,0.261538461538462,0.276923076923077,0.292307692307692,
0.307692307692308,0.323076923076923,0.338461538461538,0.353846153846154,
0.369230769230769,0.384615384615385,0.4,0.415384615384615,0.430769230769231,
0.446153846153846,0.461538461538462,0.476923076923077,0.492307692307692,
0.507692307692308,0.523076923076923,0.538461538461538,0.553846153846154,
0.569230769230769,0.584615384615384,0.6,0.615384615384615,0.63076923076923,
0.646153846153846,0.661538461538461,0.676923076923076,0.692307692307692,
0.707692307692307,0.723076923076922,0.738461538461538,0.753846153846153,
0.769230769230768,0.784615384615384,0.799999999999999,0.815384615384614,
0.83076923076923,0.846153846153845,0.86153846153846,0.876923076923076,0.892307692307691,
0.907692307692306,0.923076923076922,0.938461538461537,0.953846153846152,
0.969230769230768,0.984615384615383,1.),.UNSPECIFIED.)
CURVE()
GEOMETRIC_REPRESENTATION_ITEM()
RATIONAL_B_SPLINE_CURVE((1.,1.,1.,1.,1.,1.,1.,1.,1.,1.,1.,1.,1.,1.,1.,1.,
1.,1.,1.,1.,1.,1.,1.,1.,1.,1.,1.,1.,1.,1.,1.,1.,1.,1.,1.,1.,1.,1.,1.,1.,
1.,1.,1.,1.,1.,1.,1.,1.,1.,1.,1.,1.,1.,1.,1.,1.,1.,1.,1.,1.,1.,1.,1.,1.,
1.,1.,1.,1.,1.,1.))
REPRESENTATION_ITEM('')
);
#214=(
BOUNDED_CURVE()
B_SPLINE_CURVE(5,(#30372,#30373,#30374,#30375,#30376,#30377,#30378,#30379,
#30380,#30381,#30382,#30383,#30384,#30385,#30386,#30387,#30388,#30389,#30390,
#30391,#30392,#30393,#30394,#30395,#30396,#30397,#30398,#30399,#30400,#30401,
#30402,#30403,#30404,#30405,#30406,#30407,#30408,#30409,#30410,#30411,#30412,
#30413,#30414,#30415,#30416,#30417,#30418,#30419,#30420,#30421,#30422,#30423,
#30424,#30425,#30426,#30427,#30428,#30429,#30430,#30431,#30432,#30433,#30434,
#30435,#30436,#30437,#30438,#30439,#30440,#30441),.UNSPECIFIED.,.F.,.F.)
B_SPLINE_CURVE_WITH_KNOTS((6,1,1,1,1,1,1,1,1,1,1,1,1,1,1,1,1,1,1,1,1,1,
1,1,1,1,1,1,1,1,1,1,1,1,1,1,1,1,1,1,1,1,1,1,1,1,1,1,1,1,1,1,1,1,1,1,1,1,
1,1,1,1,1,1,1,6),(0.,0.0153846153846154,0.0307692307692308,0.0461538461538462,
0.0615384615384615,0.0769230769230769,0.0923076923076923,0.107692307692308,
0.123076923076923,0.138461538461538,0.153846153846154,0.169230769230769,
0.184615384615385,0.2,0.215384615384615,0.230769230769231,0.246153846153846,
0.261538461538462,0.276923076923077,0.292307692307692,0.307692307692308,
0.323076923076923,0.338461538461538,0.353846153846154,0.369230769230769,
0.384615384615385,0.4,0.415384615384615,0.430769230769231,0.446153846153846,
0.461538461538462,0.476923076923077,0.492307692307692,0.507692307692308,
0.523076923076923,0.538461538461538,0.553846153846154,0.569230769230769,
0.584615384615384,0.6,0.615384615384615,0.63076923076923,0.646153846153846,
0.661538461538461,0.676923076923076,0.692307692307692,0.707692307692307,
0.723076923076922,0.738461538461538,0.753846153846153,0.769230769230768,
0.784615384615384,0.799999999999999,0.815384615384614,0.83076923076923,
0.846153846153845,0.86153846153846,0.876923076923076,0.892307692307691,
0.907692307692306,0.923076923076922,0.938461538461537,0.953846153846152,
0.969230769230768,0.984615384615383,0.994228156739689),.UNSPECIFIED.)
CURVE()
GEOMETRIC_REPRESENTATION_ITEM()
RATIONAL_B_SPLINE_CURVE((1.,1.,1.,1.,1.,1.,1.,1.,1.,1.,1.,1.,1.,1.,1.,1.,
1.,1.,1.,1.,1.,1.,1.,1.,1.,1.,1.,1.,1.,1.,1.,1.,1.,1.,1.,1.,1.,1.,1.,1.,
1.,1.,1.,1.,1.,1.,1.,1.,1.,1.,1.,1.,1.,1.,1.,1.,1.,1.,1.,1.,1.,1.,1.,1.,
1.,1.,1.,1.,1.,1.))
REPRESENTATION_ITEM('')
);
#215=(
BOUNDED_CURVE()
B_SPLINE_CURVE(5,(#30445,#30446,#30447,#30448,#30449,#30450,#30451,#30452,
#30453,#30454,#30455,#30456,#30457,#30458,#30459,#30460,#30461,#30462,#30463,
#30464,#30465,#30466,#30467,#30468,#30469,#30470,#30471,#30472,#30473,#30474,
#30475,#30476,#30477,#30478,#30479,#30480,#30481,#30482,#30483,#30484,#30485,
#30486,#30487,#30488,#30489,#30490,#30491,#30492,#30493,#30494,#30495,#30496,
#30497,#30498,#30499,#30500,#30501,#30502,#30503,#30504,#30505,#30506,#30507,
#30508,#30509,#30510,#30511,#30512,#30513,#30514),.UNSPECIFIED.,.F.,.F.)
B_SPLINE_CURVE_WITH_KNOTS((6,1,1,1,1,1,1,1,1,1,1,1,1,1,1,1,1,1,1,1,1,1,
1,1,1,1,1,1,1,1,1,1,1,1,1,1,1,1,1,1,1,1,1,1,1,1,1,1,1,1,1,1,1,1,1,1,1,1,
1,1,1,1,1,1,1,6),(0.00577184337448946,0.0153846153846154,0.0307692307692308,
0.0461538461538462,0.0615384615384615,0.0769230769230769,0.0923076923076923,
0.107692307692308,0.123076923076923,0.138461538461538,0.153846153846154,
0.169230769230769,0.184615384615385,0.2,0.215384615384615,0.230769230769231,
0.246153846153846,0.261538461538462,0.276923076923077,0.292307692307692,
0.307692307692308,0.323076923076923,0.338461538461538,0.353846153846154,
0.369230769230769,0.384615384615385,0.4,0.415384615384615,0.430769230769231,
0.446153846153846,0.461538461538462,0.476923076923077,0.492307692307692,
0.507692307692308,0.523076923076923,0.538461538461538,0.553846153846154,
0.569230769230769,0.584615384615384,0.6,0.615384615384615,0.63076923076923,
0.646153846153846,0.661538461538461,0.676923076923076,0.692307692307692,
0.707692307692307,0.723076923076922,0.738461538461538,0.753846153846153,
0.769230769230768,0.784615384615384,0.799999999999999,0.815384615384614,
0.83076923076923,0.846153846153845,0.86153846153846,0.876923076923076,0.892307692307691,
0.907692307692306,0.923076923076922,0.938461538461537,0.953846153846152,
0.969230769230768,0.984615384615383,1.),.UNSPECIFIED.)
CURVE()
GEOMETRIC_REPRESENTATION_ITEM()
RATIONAL_B_SPLINE_CURVE((1.,1.,1.,1.,1.,1.,1.,1.,1.,1.,1.,1.,1.,1.,1.,1.,
1.,1.,1.,1.,1.,1.,1.,1.,1.,1.,1.,1.,1.,1.,1.,1.,1.,1.,1.,1.,1.,1.,1.,1.,
1.,1.,1.,1.,1.,1.,1.,1.,1.,1.,1.,1.,1.,1.,1.,1.,1.,1.,1.,1.,1.,1.,1.,1.,
1.,1.,1.,1.,1.,1.))
REPRESENTATION_ITEM('')
);
#216=(
BOUNDED_CURVE()
B_SPLINE_CURVE(5,(#30518,#30519,#30520,#30521,#30522,#30523,#30524,#30525,
#30526,#30527,#30528,#30529,#30530,#30531,#30532,#30533,#30534,#30535,#30536,
#30537,#30538,#30539,#30540,#30541,#30542,#30543,#30544,#30545,#30546,#30547,
#30548,#30549,#30550,#30551,#30552,#30553,#30554,#30555,#30556,#30557,#30558,
#30559,#30560,#30561,#30562,#30563,#30564,#30565,#30566,#30567,#30568,#30569,
#30570,#30571,#30572,#30573,#30574,#30575,#30576,#30577,#30578,#30579,#30580,
#30581,#30582,#30583,#30584,#30585,#30586,#30587),.UNSPECIFIED.,.F.,.F.)
B_SPLINE_CURVE_WITH_KNOTS((6,1,1,1,1,1,1,1,1,1,1,1,1,1,1,1,1,1,1,1,1,1,
1,1,1,1,1,1,1,1,1,1,1,1,1,1,1,1,1,1,1,1,1,1,1,1,1,1,1,1,1,1,1,1,1,1,1,1,
1,1,1,1,1,1,1,6),(0.,0.0153846153846154,0.0307692307692308,0.0461538461538462,
0.0615384615384615,0.0769230769230769,0.0923076923076923,0.107692307692308,
0.123076923076923,0.138461538461538,0.153846153846154,0.169230769230769,
0.184615384615385,0.2,0.215384615384615,0.230769230769231,0.246153846153846,
0.261538461538462,0.276923076923077,0.292307692307692,0.307692307692308,
0.323076923076923,0.338461538461538,0.353846153846154,0.369230769230769,
0.384615384615385,0.4,0.415384615384615,0.430769230769231,0.446153846153846,
0.461538461538462,0.476923076923077,0.492307692307692,0.507692307692308,
0.523076923076923,0.538461538461538,0.553846153846154,0.569230769230769,
0.584615384615384,0.6,0.615384615384615,0.63076923076923,0.646153846153846,
0.661538461538461,0.676923076923076,0.692307692307692,0.707692307692307,
0.723076923076922,0.738461538461538,0.753846153846153,0.769230769230768,
0.784615384615384,0.799999999999999,0.815384615384614,0.83076923076923,
0.846153846153845,0.86153846153846,0.876923076923076,0.892307692307691,
0.907692307692306,0.923076923076922,0.938461538461537,0.953846153846152,
0.969230769230768,0.984615384615383,0.994228156739718),.UNSPECIFIED.)
CURVE()
GEOMETRIC_REPRESENTATION_ITEM()
RATIONAL_B_SPLINE_CURVE((1.,1.,1.,1.,1.,1.,1.,1.,1.,1.,1.,1.,1.,1.,1.,1.,
1.,1.,1.,1.,1.,1.,1.,1.,1.,1.,1.,1.,1.,1.,1.,1.,1.,1.,1.,1.,1.,1.,1.,1.,
1.,1.,1.,1.,1.,1.,1.,1.,1.,1.,1.,1.,1.,1.,1.,1.,1.,1.,1.,1.,1.,1.,1.,1.,
1.,1.,1.,1.,1.,1.))
REPRESENTATION_ITEM('')
);
#217=(
BOUNDED_CURVE()
B_SPLINE_CURVE(5,(#30591,#30592,#30593,#30594,#30595,#30596,#30597,#30598,
#30599,#30600,#30601,#30602,#30603,#30604,#30605,#30606,#30607,#30608,#30609,
#30610,#30611,#30612,#30613,#30614,#30615,#30616,#30617,#30618,#30619,#30620,
#30621,#30622,#30623,#30624,#30625,#30626,#30627,#30628,#30629,#30630,#30631,
#30632,#30633,#30634,#30635,#30636,#30637,#30638,#30639,#30640,#30641,#30642,
#30643,#30644,#30645,#30646,#30647,#30648,#30649,#30650,#30651,#30652,#30653,
#30654,#30655,#30656,#30657,#30658,#30659,#30660),.UNSPECIFIED.,.F.,.F.)
B_SPLINE_CURVE_WITH_KNOTS((6,1,1,1,1,1,1,1,1,1,1,1,1,1,1,1,1,1,1,1,1,1,
1,1,1,1,1,1,1,1,1,1,1,1,1,1,1,1,1,1,1,1,1,1,1,1,1,1,1,1,1,1,1,1,1,1,1,1,
1,1,1,1,1,1,1,6),(0.00577184337450897,0.0153846153846154,0.0307692307692308,
0.0461538461538462,0.0615384615384615,0.0769230769230769,0.0923076923076923,
0.107692307692308,0.123076923076923,0.138461538461538,0.153846153846154,
0.169230769230769,0.184615384615385,0.2,0.215384615384615,0.230769230769231,
0.246153846153846,0.261538461538462,0.276923076923077,0.292307692307692,
0.307692307692308,0.323076923076923,0.338461538461538,0.353846153846154,
0.369230769230769,0.384615384615385,0.4,0.415384615384615,0.430769230769231,
0.446153846153846,0.461538461538462,0.476923076923077,0.492307692307692,
0.507692307692308,0.523076923076923,0.538461538461538,0.553846153846154,
0.569230769230769,0.584615384615384,0.6,0.615384615384615,0.63076923076923,
0.646153846153846,0.661538461538461,0.676923076923076,0.692307692307692,
0.707692307692307,0.723076923076922,0.738461538461538,0.753846153846153,
0.769230769230768,0.784615384615384,0.799999999999999,0.815384615384614,
0.83076923076923,0.846153846153845,0.86153846153846,0.876923076923076,0.892307692307691,
0.907692307692306,0.923076923076922,0.938461538461537,0.953846153846152,
0.969230769230768,0.984615384615383,1.),.UNSPECIFIED.)
CURVE()
GEOMETRIC_REPRESENTATION_ITEM()
RATIONAL_B_SPLINE_CURVE((1.,1.,1.,1.,1.,1.,1.,1.,1.,1.,1.,1.,1.,1.,1.,1.,
1.,1.,1.,1.,1.,1.,1.,1.,1.,1.,1.,1.,1.,1.,1.,1.,1.,1.,1.,1.,1.,1.,1.,1.,
1.,1.,1.,1.,1.,1.,1.,1.,1.,1.,1.,1.,1.,1.,1.,1.,1.,1.,1.,1.,1.,1.,1.,1.,
1.,1.,1.,1.,1.,1.))
REPRESENTATION_ITEM('')
);
#218=(
BOUNDED_CURVE()
B_SPLINE_CURVE(5,(#30664,#30665,#30666,#30667,#30668,#30669,#30670,#30671,
#30672,#30673,#30674,#30675,#30676,#30677,#30678,#30679,#30680,#30681,#30682,
#30683,#30684,#30685,#30686,#30687,#30688,#30689,#30690,#30691,#30692,#30693,
#30694,#30695,#30696,#30697,#30698,#30699,#30700,#30701,#30702,#30703,#30704,
#30705,#30706,#30707,#30708,#30709,#30710,#30711,#30712,#30713,#30714,#30715,
#30716,#30717,#30718,#30719,#30720,#30721,#30722,#30723,#30724,#30725,#30726,
#30727,#30728,#30729,#30730,#30731,#30732,#30733),.UNSPECIFIED.,.F.,.F.)
B_SPLINE_CURVE_WITH_KNOTS((6,1,1,1,1,1,1,1,1,1,1,1,1,1,1,1,1,1,1,1,1,1,
1,1,1,1,1,1,1,1,1,1,1,1,1,1,1,1,1,1,1,1,1,1,1,1,1,1,1,1,1,1,1,1,1,1,1,1,
1,1,1,1,1,1,1,6),(0.,0.0153846153846154,0.0307692307692308,0.0461538461538462,
0.0615384615384615,0.0769230769230769,0.0923076923076923,0.107692307692308,
0.123076923076923,0.138461538461538,0.153846153846154,0.169230769230769,
0.184615384615385,0.2,0.215384615384615,0.230769230769231,0.246153846153846,
0.261538461538462,0.276923076923077,0.292307692307692,0.307692307692308,
0.323076923076923,0.338461538461538,0.353846153846154,0.369230769230769,
0.384615384615385,0.4,0.415384615384615,0.430769230769231,0.446153846153846,
0.461538461538462,0.476923076923077,0.492307692307692,0.507692307692308,
0.523076923076923,0.538461538461538,0.553846153846154,0.569230769230769,
0.584615384615384,0.6,0.615384615384615,0.63076923076923,0.646153846153846,
0.661538461538461,0.676923076923076,0.692307692307692,0.707692307692307,
0.723076923076922,0.738461538461538,0.753846153846153,0.769230769230768,
0.784615384615384,0.799999999999999,0.815384615384614,0.83076923076923,
0.846153846153845,0.86153846153846,0.876923076923076,0.892307692307691,
0.907692307692306,0.923076923076922,0.938461538461537,0.953846153846152,
0.969230769230768,0.984615384615383,0.994228156739701),.UNSPECIFIED.)
CURVE()
GEOMETRIC_REPRESENTATION_ITEM()
RATIONAL_B_SPLINE_CURVE((1.,1.,1.,1.,1.,1.,1.,1.,1.,1.,1.,1.,1.,1.,1.,1.,
1.,1.,1.,1.,1.,1.,1.,1.,1.,1.,1.,1.,1.,1.,1.,1.,1.,1.,1.,1.,1.,1.,1.,1.,
1.,1.,1.,1.,1.,1.,1.,1.,1.,1.,1.,1.,1.,1.,1.,1.,1.,1.,1.,1.,1.,1.,1.,1.,
1.,1.,1.,1.,1.,1.))
REPRESENTATION_ITEM('')
);
#219=(
BOUNDED_CURVE()
B_SPLINE_CURVE(5,(#30737,#30738,#30739,#30740,#30741,#30742,#30743,#30744,
#30745,#30746,#30747,#30748,#30749,#30750,#30751,#30752,#30753,#30754,#30755,
#30756,#30757,#30758,#30759,#30760,#30761,#30762,#30763,#30764,#30765,#30766,
#30767,#30768,#30769,#30770,#30771,#30772,#30773,#30774,#30775,#30776,#30777,
#30778,#30779,#30780,#30781,#30782,#30783,#30784,#30785,#30786,#30787,#30788,
#30789,#30790,#30791,#30792,#30793,#30794,#30795,#30796,#30797,#30798,#30799,
#30800,#30801,#30802,#30803,#30804,#30805,#30806),.UNSPECIFIED.,.F.,.F.)
B_SPLINE_CURVE_WITH_KNOTS((6,1,1,1,1,1,1,1,1,1,1,1,1,1,1,1,1,1,1,1,1,1,
1,1,1,1,1,1,1,1,1,1,1,1,1,1,1,1,1,1,1,1,1,1,1,1,1,1,1,1,1,1,1,1,1,1,1,1,
1,1,1,1,1,1,1,6),(0.00577184337451001,0.0153846153846154,0.0307692307692308,
0.0461538461538462,0.0615384615384615,0.0769230769230769,0.0923076923076923,
0.107692307692308,0.123076923076923,0.138461538461538,0.153846153846154,
0.169230769230769,0.184615384615385,0.2,0.215384615384615,0.230769230769231,
0.246153846153846,0.261538461538462,0.276923076923077,0.292307692307692,
0.307692307692308,0.323076923076923,0.338461538461538,0.353846153846154,
0.369230769230769,0.384615384615385,0.4,0.415384615384615,0.430769230769231,
0.446153846153846,0.461538461538462,0.476923076923077,0.492307692307692,
0.507692307692308,0.523076923076923,0.538461538461538,0.553846153846154,
0.569230769230769,0.584615384615384,0.6,0.615384615384615,0.63076923076923,
0.646153846153846,0.661538461538461,0.676923076923076,0.692307692307692,
0.707692307692307,0.723076923076922,0.738461538461538,0.753846153846153,
0.769230769230768,0.784615384615384,0.799999999999999,0.815384615384614,
0.83076923076923,0.846153846153845,0.86153846153846,0.876923076923076,0.892307692307691,
0.907692307692306,0.923076923076922,0.938461538461537,0.953846153846152,
0.969230769230768,0.984615384615383,1.),.UNSPECIFIED.)
CURVE()
GEOMETRIC_REPRESENTATION_ITEM()
RATIONAL_B_SPLINE_CURVE((1.,1.,1.,1.,1.,1.,1.,1.,1.,1.,1.,1.,1.,1.,1.,1.,
1.,1.,1.,1.,1.,1.,1.,1.,1.,1.,1.,1.,1.,1.,1.,1.,1.,1.,1.,1.,1.,1.,1.,1.,
1.,1.,1.,1.,1.,1.,1.,1.,1.,1.,1.,1.,1.,1.,1.,1.,1.,1.,1.,1.,1.,1.,1.,1.,
1.,1.,1.,1.,1.,1.))
REPRESENTATION_ITEM('')
);
#220=(
BOUNDED_CURVE()
B_SPLINE_CURVE(5,(#30810,#30811,#30812,#30813,#30814,#30815,#30816,#30817,
#30818,#30819,#30820,#30821,#30822,#30823,#30824,#30825,#30826,#30827,#30828,
#30829,#30830,#30831,#30832,#30833,#30834,#30835,#30836,#30837,#30838,#30839,
#30840,#30841,#30842,#30843,#30844,#30845,#30846,#30847,#30848,#30849,#30850,
#30851,#30852,#30853,#30854,#30855,#30856,#30857,#30858,#30859,#30860,#30861,
#30862,#30863,#30864,#30865,#30866,#30867,#30868,#30869,#30870,#30871,#30872,
#30873,#30874,#30875,#30876,#30877,#30878,#30879),.UNSPECIFIED.,.F.,.F.)
B_SPLINE_CURVE_WITH_KNOTS((6,1,1,1,1,1,1,1,1,1,1,1,1,1,1,1,1,1,1,1,1,1,
1,1,1,1,1,1,1,1,1,1,1,1,1,1,1,1,1,1,1,1,1,1,1,1,1,1,1,1,1,1,1,1,1,1,1,1,
1,1,1,1,1,1,1,6),(0.,0.0153846153846154,0.0307692307692308,0.0461538461538462,
0.0615384615384615,0.0769230769230769,0.0923076923076923,0.107692307692308,
0.123076923076923,0.138461538461538,0.153846153846154,0.169230769230769,
0.184615384615385,0.2,0.215384615384615,0.230769230769231,0.246153846153846,
0.261538461538462,0.276923076923077,0.292307692307692,0.307692307692308,
0.323076923076923,0.338461538461538,0.353846153846154,0.369230769230769,
0.384615384615385,0.4,0.415384615384615,0.430769230769231,0.446153846153846,
0.461538461538462,0.476923076923077,0.492307692307692,0.507692307692308,
0.523076923076923,0.538461538461538,0.553846153846154,0.569230769230769,
0.584615384615384,0.6,0.615384615384615,0.63076923076923,0.646153846153846,
0.661538461538461,0.676923076923076,0.692307692307692,0.707692307692307,
0.723076923076922,0.738461538461538,0.753846153846153,0.769230769230768,
0.784615384615384,0.799999999999999,0.815384615384614,0.83076923076923,
0.846153846153845,0.86153846153846,0.876923076923076,0.892307692307691,
0.907692307692306,0.923076923076922,0.938461538461537,0.953846153846152,
0.969230769230768,0.984615384615383,0.994228156739697),.UNSPECIFIED.)
CURVE()
GEOMETRIC_REPRESENTATION_ITEM()
RATIONAL_B_SPLINE_CURVE((1.,1.,1.,1.,1.,1.,1.,1.,1.,1.,1.,1.,1.,1.,1.,1.,
1.,1.,1.,1.,1.,1.,1.,1.,1.,1.,1.,1.,1.,1.,1.,1.,1.,1.,1.,1.,1.,1.,1.,1.,
1.,1.,1.,1.,1.,1.,1.,1.,1.,1.,1.,1.,1.,1.,1.,1.,1.,1.,1.,1.,1.,1.,1.,1.,
1.,1.,1.,1.,1.,1.))
REPRESENTATION_ITEM('')
);
#221=(
BOUNDED_CURVE()
B_SPLINE_CURVE(5,(#30883,#30884,#30885,#30886,#30887,#30888,#30889,#30890,
#30891,#30892,#30893,#30894,#30895,#30896,#30897,#30898,#30899,#30900,#30901,
#30902,#30903,#30904,#30905,#30906,#30907,#30908,#30909,#30910,#30911,#30912,
#30913,#30914,#30915,#30916,#30917,#30918,#30919,#30920,#30921,#30922,#30923,
#30924,#30925,#30926,#30927,#30928,#30929,#30930,#30931,#30932,#30933,#30934,
#30935,#30936,#30937,#30938,#30939,#30940,#30941,#30942,#30943,#30944,#30945,
#30946,#30947,#30948,#30949,#30950,#30951,#30952),.UNSPECIFIED.,.F.,.F.)
B_SPLINE_CURVE_WITH_KNOTS((6,1,1,1,1,1,1,1,1,1,1,1,1,1,1,1,1,1,1,1,1,1,
1,1,1,1,1,1,1,1,1,1,1,1,1,1,1,1,1,1,1,1,1,1,1,1,1,1,1,1,1,1,1,1,1,1,1,1,
1,1,1,1,1,1,1,6),(0.00577184337452306,0.0153846153846154,0.0307692307692308,
0.0461538461538462,0.0615384615384615,0.0769230769230769,0.0923076923076923,
0.107692307692308,0.123076923076923,0.138461538461538,0.153846153846154,
0.169230769230769,0.184615384615385,0.2,0.215384615384615,0.230769230769231,
0.246153846153846,0.261538461538462,0.276923076923077,0.292307692307692,
0.307692307692308,0.323076923076923,0.338461538461538,0.353846153846154,
0.369230769230769,0.384615384615385,0.4,0.415384615384615,0.430769230769231,
0.446153846153846,0.461538461538462,0.476923076923077,0.492307692307692,
0.507692307692308,0.523076923076923,0.538461538461538,0.553846153846154,
0.569230769230769,0.584615384615384,0.6,0.615384615384615,0.63076923076923,
0.646153846153846,0.661538461538461,0.676923076923076,0.692307692307692,
0.707692307692307,0.723076923076922,0.738461538461538,0.753846153846153,
0.769230769230768,0.784615384615384,0.799999999999999,0.815384615384614,
0.83076923076923,0.846153846153845,0.86153846153846,0.876923076923076,0.892307692307691,
0.907692307692306,0.923076923076922,0.938461538461537,0.953846153846152,
0.969230769230768,0.984615384615383,1.),.UNSPECIFIED.)
CURVE()
GEOMETRIC_REPRESENTATION_ITEM()
RATIONAL_B_SPLINE_CURVE((1.,1.,1.,1.,1.,1.,1.,1.,1.,1.,1.,1.,1.,1.,1.,1.,
1.,1.,1.,1.,1.,1.,1.,1.,1.,1.,1.,1.,1.,1.,1.,1.,1.,1.,1.,1.,1.,1.,1.,1.,
1.,1.,1.,1.,1.,1.,1.,1.,1.,1.,1.,1.,1.,1.,1.,1.,1.,1.,1.,1.,1.,1.,1.,1.,
1.,1.,1.,1.,1.,1.))
REPRESENTATION_ITEM('')
);
#222=(
BOUNDED_CURVE()
B_SPLINE_CURVE(5,(#30956,#30957,#30958,#30959,#30960,#30961,#30962,#30963,
#30964,#30965,#30966,#30967,#30968,#30969,#30970,#30971,#30972,#30973,#30974,
#30975,#30976,#30977,#30978,#30979,#30980,#30981,#30982,#30983,#30984,#30985,
#30986,#30987,#30988,#30989,#30990,#30991,#30992,#30993,#30994,#30995,#30996,
#30997,#30998,#30999,#31000,#31001,#31002,#31003,#31004,#31005,#31006,#31007,
#31008,#31009,#31010,#31011,#31012,#31013,#31014,#31015,#31016,#31017,#31018,
#31019,#31020,#31021,#31022,#31023,#31024,#31025),.UNSPECIFIED.,.F.,.F.)
B_SPLINE_CURVE_WITH_KNOTS((6,1,1,1,1,1,1,1,1,1,1,1,1,1,1,1,1,1,1,1,1,1,
1,1,1,1,1,1,1,1,1,1,1,1,1,1,1,1,1,1,1,1,1,1,1,1,1,1,1,1,1,1,1,1,1,1,1,1,
1,1,1,1,1,1,1,6),(0.,0.0153846153846154,0.0307692307692308,0.0461538461538462,
0.0615384615384615,0.0769230769230769,0.0923076923076923,0.107692307692308,
0.123076923076923,0.138461538461538,0.153846153846154,0.169230769230769,
0.184615384615385,0.2,0.215384615384615,0.230769230769231,0.246153846153846,
0.261538461538462,0.276923076923077,0.292307692307692,0.307692307692308,
0.323076923076923,0.338461538461538,0.353846153846154,0.369230769230769,
0.384615384615385,0.4,0.415384615384615,0.430769230769231,0.446153846153846,
0.461538461538462,0.476923076923077,0.492307692307692,0.507692307692308,
0.523076923076923,0.538461538461538,0.553846153846154,0.569230769230769,
0.584615384615384,0.6,0.615384615384615,0.63076923076923,0.646153846153846,
0.661538461538461,0.676923076923076,0.692307692307692,0.707692307692307,
0.723076923076922,0.738461538461538,0.753846153846153,0.769230769230768,
0.784615384615384,0.799999999999999,0.815384615384614,0.83076923076923,
0.846153846153845,0.86153846153846,0.876923076923076,0.892307692307691,
0.907692307692306,0.923076923076922,0.938461538461537,0.953846153846152,
0.969230769230768,0.984615384615383,0.994228156739688),.UNSPECIFIED.)
CURVE()
GEOMETRIC_REPRESENTATION_ITEM()
RATIONAL_B_SPLINE_CURVE((1.,1.,1.,1.,1.,1.,1.,1.,1.,1.,1.,1.,1.,1.,1.,1.,
1.,1.,1.,1.,1.,1.,1.,1.,1.,1.,1.,1.,1.,1.,1.,1.,1.,1.,1.,1.,1.,1.,1.,1.,
1.,1.,1.,1.,1.,1.,1.,1.,1.,1.,1.,1.,1.,1.,1.,1.,1.,1.,1.,1.,1.,1.,1.,1.,
1.,1.,1.,1.,1.,1.))
REPRESENTATION_ITEM('')
);
#223=(
BOUNDED_CURVE()
B_SPLINE_CURVE(5,(#31029,#31030,#31031,#31032,#31033,#31034,#31035,#31036,
#31037,#31038,#31039,#31040,#31041,#31042,#31043,#31044,#31045,#31046,#31047,
#31048,#31049,#31050,#31051,#31052,#31053,#31054,#31055,#31056,#31057,#31058,
#31059,#31060,#31061,#31062,#31063,#31064,#31065,#31066,#31067,#31068,#31069,
#31070,#31071,#31072,#31073,#31074,#31075,#31076,#31077,#31078,#31079,#31080,
#31081,#31082,#31083,#31084,#31085,#31086,#31087,#31088,#31089,#31090,#31091,
#31092,#31093,#31094,#31095,#31096,#31097,#31098),.UNSPECIFIED.,.F.,.F.)
B_SPLINE_CURVE_WITH_KNOTS((6,1,1,1,1,1,1,1,1,1,1,1,1,1,1,1,1,1,1,1,1,1,
1,1,1,1,1,1,1,1,1,1,1,1,1,1,1,1,1,1,1,1,1,1,1,1,1,1,1,1,1,1,1,1,1,1,1,1,
1,1,1,1,1,1,1,6),(0.00577184337449862,0.0153846153846154,0.0307692307692308,
0.0461538461538462,0.0615384615384615,0.0769230769230769,0.0923076923076923,
0.107692307692308,0.123076923076923,0.138461538461538,0.153846153846154,
0.169230769230769,0.184615384615385,0.2,0.215384615384615,0.230769230769231,
0.246153846153846,0.261538461538462,0.276923076923077,0.292307692307692,
0.307692307692308,0.323076923076923,0.338461538461538,0.353846153846154,
0.369230769230769,0.384615384615385,0.4,0.415384615384615,0.430769230769231,
0.446153846153846,0.461538461538462,0.476923076923077,0.492307692307692,
0.507692307692308,0.523076923076923,0.538461538461538,0.553846153846154,
0.569230769230769,0.584615384615384,0.6,0.615384615384615,0.63076923076923,
0.646153846153846,0.661538461538461,0.676923076923076,0.692307692307692,
0.707692307692307,0.723076923076922,0.738461538461538,0.753846153846153,
0.769230769230768,0.784615384615384,0.799999999999999,0.815384615384614,
0.83076923076923,0.846153846153845,0.86153846153846,0.876923076923076,0.892307692307691,
0.907692307692306,0.923076923076922,0.938461538461537,0.953846153846152,
0.969230769230768,0.984615384615383,1.),.UNSPECIFIED.)
CURVE()
GEOMETRIC_REPRESENTATION_ITEM()
RATIONAL_B_SPLINE_CURVE((1.,1.,1.,1.,1.,1.,1.,1.,1.,1.,1.,1.,1.,1.,1.,1.,
1.,1.,1.,1.,1.,1.,1.,1.,1.,1.,1.,1.,1.,1.,1.,1.,1.,1.,1.,1.,1.,1.,1.,1.,
1.,1.,1.,1.,1.,1.,1.,1.,1.,1.,1.,1.,1.,1.,1.,1.,1.,1.,1.,1.,1.,1.,1.,1.,
1.,1.,1.,1.,1.,1.))
REPRESENTATION_ITEM('')
);
#224=(
BOUNDED_CURVE()
B_SPLINE_CURVE(5,(#31102,#31103,#31104,#31105,#31106,#31107,#31108,#31109,
#31110,#31111,#31112,#31113,#31114,#31115,#31116,#31117,#31118,#31119,#31120,
#31121,#31122,#31123,#31124,#31125,#31126,#31127,#31128,#31129,#31130,#31131,
#31132,#31133,#31134,#31135,#31136,#31137,#31138,#31139,#31140,#31141,#31142,
#31143,#31144,#31145,#31146,#31147,#31148,#31149,#31150,#31151,#31152,#31153,
#31154,#31155,#31156,#31157,#31158,#31159,#31160,#31161,#31162,#31163,#31164,
#31165,#31166,#31167,#31168,#31169,#31170,#31171),.UNSPECIFIED.,.F.,.F.)
B_SPLINE_CURVE_WITH_KNOTS((6,1,1,1,1,1,1,1,1,1,1,1,1,1,1,1,1,1,1,1,1,1,
1,1,1,1,1,1,1,1,1,1,1,1,1,1,1,1,1,1,1,1,1,1,1,1,1,1,1,1,1,1,1,1,1,1,1,1,
1,1,1,1,1,1,1,6),(0.,0.0153846153846154,0.0307692307692308,0.0461538461538462,
0.0615384615384615,0.0769230769230769,0.0923076923076923,0.107692307692308,
0.123076923076923,0.138461538461538,0.153846153846154,0.169230769230769,
0.184615384615385,0.2,0.215384615384615,0.230769230769231,0.246153846153846,
0.261538461538462,0.276923076923077,0.292307692307692,0.307692307692308,
0.323076923076923,0.338461538461538,0.353846153846154,0.369230769230769,
0.384615384615385,0.4,0.415384615384615,0.430769230769231,0.446153846153846,
0.461538461538462,0.476923076923077,0.492307692307692,0.507692307692308,
0.523076923076923,0.538461538461538,0.553846153846154,0.569230769230769,
0.584615384615384,0.6,0.615384615384615,0.63076923076923,0.646153846153846,
0.661538461538461,0.676923076923076,0.692307692307692,0.707692307692307,
0.723076923076922,0.738461538461538,0.753846153846153,0.769230769230768,
0.784615384615384,0.799999999999999,0.815384615384614,0.83076923076923,
0.846153846153845,0.86153846153846,0.876923076923076,0.892307692307691,
0.907692307692306,0.923076923076922,0.938461538461537,0.953846153846152,
0.969230769230768,0.984615384615383,0.994228156739696),.UNSPECIFIED.)
CURVE()
GEOMETRIC_REPRESENTATION_ITEM()
RATIONAL_B_SPLINE_CURVE((1.,1.,1.,1.,1.,1.,1.,1.,1.,1.,1.,1.,1.,1.,1.,1.,
1.,1.,1.,1.,1.,1.,1.,1.,1.,1.,1.,1.,1.,1.,1.,1.,1.,1.,1.,1.,1.,1.,1.,1.,
1.,1.,1.,1.,1.,1.,1.,1.,1.,1.,1.,1.,1.,1.,1.,1.,1.,1.,1.,1.,1.,1.,1.,1.,
1.,1.,1.,1.,1.,1.))
REPRESENTATION_ITEM('')
);
#225=(
BOUNDED_CURVE()
B_SPLINE_CURVE(5,(#31175,#31176,#31177,#31178,#31179,#31180,#31181,#31182,
#31183,#31184,#31185,#31186,#31187,#31188,#31189,#31190,#31191,#31192,#31193,
#31194,#31195,#31196,#31197,#31198,#31199,#31200,#31201,#31202,#31203,#31204,
#31205,#31206,#31207,#31208,#31209,#31210,#31211,#31212,#31213,#31214,#31215,
#31216,#31217,#31218,#31219,#31220,#31221,#31222,#31223,#31224,#31225,#31226,
#31227,#31228,#31229,#31230,#31231,#31232,#31233,#31234,#31235,#31236,#31237,
#31238,#31239,#31240,#31241,#31242,#31243,#31244),.UNSPECIFIED.,.F.,.F.)
B_SPLINE_CURVE_WITH_KNOTS((6,1,1,1,1,1,1,1,1,1,1,1,1,1,1,1,1,1,1,1,1,1,
1,1,1,1,1,1,1,1,1,1,1,1,1,1,1,1,1,1,1,1,1,1,1,1,1,1,1,1,1,1,1,1,1,1,1,1,
1,1,1,1,1,1,1,6),(0.00577184337452068,0.0153846153846154,0.0307692307692308,
0.0461538461538462,0.0615384615384615,0.0769230769230769,0.0923076923076923,
0.107692307692308,0.123076923076923,0.138461538461538,0.153846153846154,
0.169230769230769,0.184615384615385,0.2,0.215384615384615,0.230769230769231,
0.246153846153846,0.261538461538462,0.276923076923077,0.292307692307692,
0.307692307692308,0.323076923076923,0.338461538461538,0.353846153846154,
0.369230769230769,0.384615384615385,0.4,0.415384615384615,0.430769230769231,
0.446153846153846,0.461538461538462,0.476923076923077,0.492307692307692,
0.507692307692308,0.523076923076923,0.538461538461538,0.553846153846154,
0.569230769230769,0.584615384615384,0.6,0.615384615384615,0.63076923076923,
0.646153846153846,0.661538461538461,0.676923076923076,0.692307692307692,
0.707692307692307,0.723076923076922,0.738461538461538,0.753846153846153,
0.769230769230768,0.784615384615384,0.799999999999999,0.815384615384614,
0.83076923076923,0.846153846153845,0.86153846153846,0.876923076923076,0.892307692307691,
0.907692307692306,0.923076923076922,0.938461538461537,0.953846153846152,
0.969230769230768,0.984615384615383,1.),.UNSPECIFIED.)
CURVE()
GEOMETRIC_REPRESENTATION_ITEM()
RATIONAL_B_SPLINE_CURVE((1.,1.,1.,1.,1.,1.,1.,1.,1.,1.,1.,1.,1.,1.,1.,1.,
1.,1.,1.,1.,1.,1.,1.,1.,1.,1.,1.,1.,1.,1.,1.,1.,1.,1.,1.,1.,1.,1.,1.,1.,
1.,1.,1.,1.,1.,1.,1.,1.,1.,1.,1.,1.,1.,1.,1.,1.,1.,1.,1.,1.,1.,1.,1.,1.,
1.,1.,1.,1.,1.,1.))
REPRESENTATION_ITEM('')
);
#226=(
BOUNDED_CURVE()
B_SPLINE_CURVE(5,(#31248,#31249,#31250,#31251,#31252,#31253,#31254,#31255,
#31256,#31257,#31258,#31259,#31260,#31261,#31262,#31263,#31264,#31265,#31266,
#31267,#31268,#31269,#31270,#31271,#31272,#31273,#31274,#31275,#31276,#31277,
#31278,#31279,#31280,#31281,#31282,#31283,#31284,#31285,#31286,#31287,#31288,
#31289,#31290,#31291,#31292,#31293,#31294,#31295,#31296,#31297,#31298,#31299,
#31300,#31301,#31302,#31303,#31304,#31305,#31306,#31307,#31308,#31309,#31310,
#31311,#31312,#31313,#31314,#31315,#31316,#31317),.UNSPECIFIED.,.F.,.F.)
B_SPLINE_CURVE_WITH_KNOTS((6,1,1,1,1,1,1,1,1,1,1,1,1,1,1,1,1,1,1,1,1,1,
1,1,1,1,1,1,1,1,1,1,1,1,1,1,1,1,1,1,1,1,1,1,1,1,1,1,1,1,1,1,1,1,1,1,1,1,
1,1,1,1,1,1,1,6),(0.,0.0153846153846154,0.0307692307692308,0.0461538461538462,
0.0615384615384615,0.0769230769230769,0.0923076923076923,0.107692307692308,
0.123076923076923,0.138461538461538,0.153846153846154,0.169230769230769,
0.184615384615385,0.2,0.215384615384615,0.230769230769231,0.246153846153846,
0.261538461538462,0.276923076923077,0.292307692307692,0.307692307692308,
0.323076923076923,0.338461538461538,0.353846153846154,0.369230769230769,
0.384615384615385,0.4,0.415384615384615,0.430769230769231,0.446153846153846,
0.461538461538462,0.476923076923077,0.492307692307692,0.507692307692308,
0.523076923076923,0.538461538461538,0.553846153846154,0.569230769230769,
0.584615384615384,0.6,0.615384615384615,0.63076923076923,0.646153846153846,
0.661538461538461,0.676923076923076,0.692307692307692,0.707692307692307,
0.723076923076922,0.738461538461538,0.753846153846153,0.769230769230768,
0.784615384615384,0.799999999999999,0.815384615384614,0.83076923076923,
0.846153846153845,0.86153846153846,0.876923076923076,0.892307692307691,
0.907692307692306,0.923076923076922,0.938461538461537,0.953846153846152,
0.969230769230768,0.984615384615383,0.994228156739698),.UNSPECIFIED.)
CURVE()
GEOMETRIC_REPRESENTATION_ITEM()
RATIONAL_B_SPLINE_CURVE((1.,1.,1.,1.,1.,1.,1.,1.,1.,1.,1.,1.,1.,1.,1.,1.,
1.,1.,1.,1.,1.,1.,1.,1.,1.,1.,1.,1.,1.,1.,1.,1.,1.,1.,1.,1.,1.,1.,1.,1.,
1.,1.,1.,1.,1.,1.,1.,1.,1.,1.,1.,1.,1.,1.,1.,1.,1.,1.,1.,1.,1.,1.,1.,1.,
1.,1.,1.,1.,1.,1.))
REPRESENTATION_ITEM('')
);
#227=(
BOUNDED_CURVE()
B_SPLINE_CURVE(5,(#31321,#31322,#31323,#31324,#31325,#31326,#31327,#31328,
#31329,#31330,#31331,#31332,#31333,#31334,#31335,#31336,#31337,#31338,#31339,
#31340,#31341,#31342,#31343,#31344,#31345,#31346,#31347,#31348,#31349,#31350,
#31351,#31352,#31353,#31354,#31355,#31356,#31357,#31358,#31359,#31360,#31361,
#31362,#31363,#31364,#31365,#31366,#31367,#31368,#31369,#31370,#31371,#31372,
#31373,#31374,#31375,#31376,#31377,#31378,#31379,#31380,#31381,#31382,#31383,
#31384,#31385,#31386,#31387,#31388,#31389,#31390),.UNSPECIFIED.,.F.,.F.)
B_SPLINE_CURVE_WITH_KNOTS((6,1,1,1,1,1,1,1,1,1,1,1,1,1,1,1,1,1,1,1,1,1,
1,1,1,1,1,1,1,1,1,1,1,1,1,1,1,1,1,1,1,1,1,1,1,1,1,1,1,1,1,1,1,1,1,1,1,1,
1,1,1,1,1,1,1,6),(0.00577184337451607,0.0153846153846154,0.0307692307692308,
0.0461538461538462,0.0615384615384615,0.0769230769230769,0.0923076923076923,
0.107692307692308,0.123076923076923,0.138461538461538,0.153846153846154,
0.169230769230769,0.184615384615385,0.2,0.215384615384615,0.230769230769231,
0.246153846153846,0.261538461538462,0.276923076923077,0.292307692307692,
0.307692307692308,0.323076923076923,0.338461538461538,0.353846153846154,
0.369230769230769,0.384615384615385,0.4,0.415384615384615,0.430769230769231,
0.446153846153846,0.461538461538462,0.476923076923077,0.492307692307692,
0.507692307692308,0.523076923076923,0.538461538461538,0.553846153846154,
0.569230769230769,0.584615384615384,0.6,0.615384615384615,0.63076923076923,
0.646153846153846,0.661538461538461,0.676923076923076,0.692307692307692,
0.707692307692307,0.723076923076922,0.738461538461538,0.753846153846153,
0.769230769230768,0.784615384615384,0.799999999999999,0.815384615384614,
0.83076923076923,0.846153846153845,0.86153846153846,0.876923076923076,0.892307692307691,
0.907692307692306,0.923076923076922,0.938461538461537,0.953846153846152,
0.969230769230768,0.984615384615383,1.),.UNSPECIFIED.)
CURVE()
GEOMETRIC_REPRESENTATION_ITEM()
RATIONAL_B_SPLINE_CURVE((1.,1.,1.,1.,1.,1.,1.,1.,1.,1.,1.,1.,1.,1.,1.,1.,
1.,1.,1.,1.,1.,1.,1.,1.,1.,1.,1.,1.,1.,1.,1.,1.,1.,1.,1.,1.,1.,1.,1.,1.,
1.,1.,1.,1.,1.,1.,1.,1.,1.,1.,1.,1.,1.,1.,1.,1.,1.,1.,1.,1.,1.,1.,1.,1.,
1.,1.,1.,1.,1.,1.))
REPRESENTATION_ITEM('')
);
#228=(
BOUNDED_CURVE()
B_SPLINE_CURVE(5,(#31394,#31395,#31396,#31397,#31398,#31399,#31400,#31401,
#31402,#31403,#31404,#31405,#31406,#31407,#31408,#31409,#31410,#31411,#31412,
#31413,#31414,#31415,#31416,#31417,#31418,#31419,#31420,#31421,#31422,#31423,
#31424,#31425,#31426,#31427,#31428,#31429,#31430,#31431,#31432,#31433,#31434,
#31435,#31436,#31437,#31438,#31439,#31440,#31441,#31442,#31443,#31444,#31445,
#31446,#31447,#31448,#31449,#31450,#31451,#31452,#31453,#31454,#31455,#31456,
#31457,#31458,#31459,#31460,#31461,#31462,#31463),.UNSPECIFIED.,.F.,.F.)
B_SPLINE_CURVE_WITH_KNOTS((6,1,1,1,1,1,1,1,1,1,1,1,1,1,1,1,1,1,1,1,1,1,
1,1,1,1,1,1,1,1,1,1,1,1,1,1,1,1,1,1,1,1,1,1,1,1,1,1,1,1,1,1,1,1,1,1,1,1,
1,1,1,1,1,1,1,6),(0.,0.0153846153846154,0.0307692307692308,0.0461538461538462,
0.0615384615384615,0.0769230769230769,0.0923076923076923,0.107692307692308,
0.123076923076923,0.138461538461538,0.153846153846154,0.169230769230769,
0.184615384615385,0.2,0.215384615384615,0.230769230769231,0.246153846153846,
0.261538461538462,0.276923076923077,0.292307692307692,0.307692307692308,
0.323076923076923,0.338461538461538,0.353846153846154,0.369230769230769,
0.384615384615385,0.4,0.415384615384615,0.430769230769231,0.446153846153846,
0.461538461538462,0.476923076923077,0.492307692307692,0.507692307692308,
0.523076923076923,0.538461538461538,0.553846153846154,0.569230769230769,
0.584615384615384,0.6,0.615384615384615,0.63076923076923,0.646153846153846,
0.661538461538461,0.676923076923076,0.692307692307692,0.707692307692307,
0.723076923076922,0.738461538461538,0.753846153846153,0.769230769230768,
0.784615384615384,0.799999999999999,0.815384615384614,0.83076923076923,
0.846153846153845,0.86153846153846,0.876923076923076,0.892307692307691,
0.907692307692306,0.923076923076922,0.938461538461537,0.953846153846152,
0.969230769230768,0.984615384615383,0.994228156739704),.UNSPECIFIED.)
CURVE()
GEOMETRIC_REPRESENTATION_ITEM()
RATIONAL_B_SPLINE_CURVE((1.,1.,1.,1.,1.,1.,1.,1.,1.,1.,1.,1.,1.,1.,1.,1.,
1.,1.,1.,1.,1.,1.,1.,1.,1.,1.,1.,1.,1.,1.,1.,1.,1.,1.,1.,1.,1.,1.,1.,1.,
1.,1.,1.,1.,1.,1.,1.,1.,1.,1.,1.,1.,1.,1.,1.,1.,1.,1.,1.,1.,1.,1.,1.,1.,
1.,1.,1.,1.,1.,1.))
REPRESENTATION_ITEM('')
);
#229=(
BOUNDED_CURVE()
B_SPLINE_CURVE(5,(#31467,#31468,#31469,#31470,#31471,#31472,#31473,#31474,
#31475,#31476,#31477,#31478,#31479,#31480,#31481,#31482,#31483,#31484,#31485,
#31486,#31487,#31488,#31489,#31490,#31491,#31492,#31493,#31494,#31495,#31496,
#31497,#31498,#31499,#31500,#31501,#31502,#31503,#31504,#31505,#31506,#31507,
#31508,#31509,#31510,#31511,#31512,#31513,#31514,#31515,#31516,#31517,#31518,
#31519,#31520,#31521,#31522,#31523,#31524,#31525,#31526,#31527,#31528,#31529,
#31530,#31531,#31532,#31533,#31534,#31535,#31536),.UNSPECIFIED.,.F.,.F.)
B_SPLINE_CURVE_WITH_KNOTS((6,1,1,1,1,1,1,1,1,1,1,1,1,1,1,1,1,1,1,1,1,1,
1,1,1,1,1,1,1,1,1,1,1,1,1,1,1,1,1,1,1,1,1,1,1,1,1,1,1,1,1,1,1,1,1,1,1,1,
1,1,1,1,1,1,1,6),(0.00577184337449692,0.0153846153846154,0.0307692307692308,
0.0461538461538462,0.0615384615384615,0.0769230769230769,0.0923076923076923,
0.107692307692308,0.123076923076923,0.138461538461538,0.153846153846154,
0.169230769230769,0.184615384615385,0.2,0.215384615384615,0.230769230769231,
0.246153846153846,0.261538461538462,0.276923076923077,0.292307692307692,
0.307692307692308,0.323076923076923,0.338461538461538,0.353846153846154,
0.369230769230769,0.384615384615385,0.4,0.415384615384615,0.430769230769231,
0.446153846153846,0.461538461538462,0.476923076923077,0.492307692307692,
0.507692307692308,0.523076923076923,0.538461538461538,0.553846153846154,
0.569230769230769,0.584615384615384,0.6,0.615384615384615,0.63076923076923,
0.646153846153846,0.661538461538461,0.676923076923076,0.692307692307692,
0.707692307692307,0.723076923076922,0.738461538461538,0.753846153846153,
0.769230769230768,0.784615384615384,0.799999999999999,0.815384615384614,
0.83076923076923,0.846153846153845,0.86153846153846,0.876923076923076,0.892307692307691,
0.907692307692306,0.923076923076922,0.938461538461537,0.953846153846152,
0.969230769230768,0.984615384615383,1.),.UNSPECIFIED.)
CURVE()
GEOMETRIC_REPRESENTATION_ITEM()
RATIONAL_B_SPLINE_CURVE((1.,1.,1.,1.,1.,1.,1.,1.,1.,1.,1.,1.,1.,1.,1.,1.,
1.,1.,1.,1.,1.,1.,1.,1.,1.,1.,1.,1.,1.,1.,1.,1.,1.,1.,1.,1.,1.,1.,1.,1.,
1.,1.,1.,1.,1.,1.,1.,1.,1.,1.,1.,1.,1.,1.,1.,1.,1.,1.,1.,1.,1.,1.,1.,1.,
1.,1.,1.,1.,1.,1.))
REPRESENTATION_ITEM('')
);
#230=(
BOUNDED_CURVE()
B_SPLINE_CURVE(5,(#31540,#31541,#31542,#31543,#31544,#31545,#31546,#31547,
#31548,#31549,#31550,#31551,#31552,#31553,#31554,#31555,#31556,#31557,#31558,
#31559,#31560,#31561,#31562,#31563,#31564,#31565,#31566,#31567,#31568,#31569,
#31570,#31571,#31572,#31573,#31574,#31575,#31576,#31577,#31578,#31579,#31580,
#31581,#31582,#31583,#31584,#31585,#31586,#31587,#31588,#31589,#31590,#31591,
#31592,#31593,#31594,#31595,#31596,#31597,#31598,#31599,#31600,#31601,#31602,
#31603,#31604,#31605,#31606,#31607,#31608,#31609),.UNSPECIFIED.,.F.,.F.)
B_SPLINE_CURVE_WITH_KNOTS((6,1,1,1,1,1,1,1,1,1,1,1,1,1,1,1,1,1,1,1,1,1,
1,1,1,1,1,1,1,1,1,1,1,1,1,1,1,1,1,1,1,1,1,1,1,1,1,1,1,1,1,1,1,1,1,1,1,1,
1,1,1,1,1,1,1,6),(0.,0.0153846153846154,0.0307692307692308,0.0461538461538462,
0.0615384615384615,0.0769230769230769,0.0923076923076923,0.107692307692308,
0.123076923076923,0.138461538461538,0.153846153846154,0.169230769230769,
0.184615384615385,0.2,0.215384615384615,0.230769230769231,0.246153846153846,
0.261538461538462,0.276923076923077,0.292307692307692,0.307692307692308,
0.323076923076923,0.338461538461538,0.353846153846154,0.369230769230769,
0.384615384615385,0.4,0.415384615384615,0.430769230769231,0.446153846153846,
0.461538461538462,0.476923076923077,0.492307692307692,0.507692307692308,
0.523076923076923,0.538461538461538,0.553846153846154,0.569230769230769,
0.584615384615384,0.6,0.615384615384615,0.63076923076923,0.646153846153846,
0.661538461538461,0.676923076923076,0.692307692307692,0.707692307692307,
0.723076923076922,0.738461538461538,0.753846153846153,0.769230769230768,
0.784615384615384,0.799999999999999,0.815384615384614,0.83076923076923,
0.846153846153845,0.86153846153846,0.876923076923076,0.892307692307691,
0.907692307692306,0.923076923076922,0.938461538461537,0.953846153846152,
0.969230769230768,0.984615384615383,0.994228156739711),.UNSPECIFIED.)
CURVE()
GEOMETRIC_REPRESENTATION_ITEM()
RATIONAL_B_SPLINE_CURVE((1.,1.,1.,1.,1.,1.,1.,1.,1.,1.,1.,1.,1.,1.,1.,1.,
1.,1.,1.,1.,1.,1.,1.,1.,1.,1.,1.,1.,1.,1.,1.,1.,1.,1.,1.,1.,1.,1.,1.,1.,
1.,1.,1.,1.,1.,1.,1.,1.,1.,1.,1.,1.,1.,1.,1.,1.,1.,1.,1.,1.,1.,1.,1.,1.,
1.,1.,1.,1.,1.,1.))
REPRESENTATION_ITEM('')
);
#231=(
BOUNDED_CURVE()
B_SPLINE_CURVE(5,(#31613,#31614,#31615,#31616,#31617,#31618,#31619,#31620,
#31621,#31622,#31623,#31624,#31625,#31626,#31627,#31628,#31629,#31630,#31631,
#31632,#31633,#31634,#31635,#31636,#31637,#31638,#31639,#31640,#31641,#31642,
#31643,#31644,#31645,#31646,#31647,#31648,#31649,#31650,#31651,#31652,#31653,
#31654,#31655,#31656,#31657,#31658,#31659,#31660,#31661,#31662,#31663,#31664,
#31665,#31666,#31667,#31668,#31669,#31670,#31671,#31672,#31673,#31674,#31675,
#31676,#31677,#31678,#31679,#31680,#31681,#31682),.UNSPECIFIED.,.F.,.F.)
B_SPLINE_CURVE_WITH_KNOTS((6,1,1,1,1,1,1,1,1,1,1,1,1,1,1,1,1,1,1,1,1,1,
1,1,1,1,1,1,1,1,1,1,1,1,1,1,1,1,1,1,1,1,1,1,1,1,1,1,1,1,1,1,1,1,1,1,1,1,
1,1,1,1,1,1,1,6),(0.00577184337450058,0.0153846153846154,0.0307692307692308,
0.0461538461538462,0.0615384615384615,0.0769230769230769,0.0923076923076923,
0.107692307692308,0.123076923076923,0.138461538461538,0.153846153846154,
0.169230769230769,0.184615384615385,0.2,0.215384615384615,0.230769230769231,
0.246153846153846,0.261538461538462,0.276923076923077,0.292307692307692,
0.307692307692308,0.323076923076923,0.338461538461538,0.353846153846154,
0.369230769230769,0.384615384615385,0.4,0.415384615384615,0.430769230769231,
0.446153846153846,0.461538461538462,0.476923076923077,0.492307692307692,
0.507692307692308,0.523076923076923,0.538461538461538,0.553846153846154,
0.569230769230769,0.584615384615384,0.6,0.615384615384615,0.63076923076923,
0.646153846153846,0.661538461538461,0.676923076923076,0.692307692307692,
0.707692307692307,0.723076923076922,0.738461538461538,0.753846153846153,
0.769230769230768,0.784615384615384,0.799999999999999,0.815384615384614,
0.83076923076923,0.846153846153845,0.86153846153846,0.876923076923076,0.892307692307691,
0.907692307692306,0.923076923076922,0.938461538461537,0.953846153846152,
0.969230769230768,0.984615384615383,1.),.UNSPECIFIED.)
CURVE()
GEOMETRIC_REPRESENTATION_ITEM()
RATIONAL_B_SPLINE_CURVE((1.,1.,1.,1.,1.,1.,1.,1.,1.,1.,1.,1.,1.,1.,1.,1.,
1.,1.,1.,1.,1.,1.,1.,1.,1.,1.,1.,1.,1.,1.,1.,1.,1.,1.,1.,1.,1.,1.,1.,1.,
1.,1.,1.,1.,1.,1.,1.,1.,1.,1.,1.,1.,1.,1.,1.,1.,1.,1.,1.,1.,1.,1.,1.,1.,
1.,1.,1.,1.,1.,1.))
REPRESENTATION_ITEM('')
);
#232=(
BOUNDED_CURVE()
B_SPLINE_CURVE(5,(#31686,#31687,#31688,#31689,#31690,#31691,#31692,#31693,
#31694,#31695,#31696,#31697,#31698,#31699,#31700,#31701,#31702,#31703,#31704,
#31705,#31706,#31707,#31708,#31709,#31710,#31711,#31712,#31713,#31714,#31715,
#31716,#31717,#31718,#31719,#31720,#31721,#31722,#31723,#31724,#31725,#31726,
#31727,#31728,#31729,#31730,#31731,#31732,#31733,#31734,#31735,#31736,#31737,
#31738,#31739,#31740,#31741,#31742,#31743,#31744,#31745,#31746,#31747,#31748,
#31749,#31750,#31751,#31752,#31753,#31754,#31755),.UNSPECIFIED.,.F.,.F.)
B_SPLINE_CURVE_WITH_KNOTS((6,1,1,1,1,1,1,1,1,1,1,1,1,1,1,1,1,1,1,1,1,1,
1,1,1,1,1,1,1,1,1,1,1,1,1,1,1,1,1,1,1,1,1,1,1,1,1,1,1,1,1,1,1,1,1,1,1,1,
1,1,1,1,1,1,1,6),(0.,0.0153846153846154,0.0307692307692308,0.0461538461538462,
0.0615384615384615,0.0769230769230769,0.0923076923076923,0.107692307692308,
0.123076923076923,0.138461538461538,0.153846153846154,0.169230769230769,
0.184615384615385,0.2,0.215384615384615,0.230769230769231,0.246153846153846,
0.261538461538462,0.276923076923077,0.292307692307692,0.307692307692308,
0.323076923076923,0.338461538461538,0.353846153846154,0.369230769230769,
0.384615384615385,0.4,0.415384615384615,0.430769230769231,0.446153846153846,
0.461538461538462,0.476923076923077,0.492307692307692,0.507692307692308,
0.523076923076923,0.538461538461538,0.553846153846154,0.569230769230769,
0.584615384615384,0.6,0.615384615384615,0.63076923076923,0.646153846153846,
0.661538461538461,0.676923076923076,0.692307692307692,0.707692307692307,
0.723076923076922,0.738461538461538,0.753846153846153,0.769230769230768,
0.784615384615384,0.799999999999999,0.815384615384614,0.83076923076923,
0.846153846153845,0.86153846153846,0.876923076923076,0.892307692307691,
0.907692307692306,0.923076923076922,0.938461538461537,0.953846153846152,
0.969230769230768,0.984615384615383,0.994228156739701),.UNSPECIFIED.)
CURVE()
GEOMETRIC_REPRESENTATION_ITEM()
RATIONAL_B_SPLINE_CURVE((1.,1.,1.,1.,1.,1.,1.,1.,1.,1.,1.,1.,1.,1.,1.,1.,
1.,1.,1.,1.,1.,1.,1.,1.,1.,1.,1.,1.,1.,1.,1.,1.,1.,1.,1.,1.,1.,1.,1.,1.,
1.,1.,1.,1.,1.,1.,1.,1.,1.,1.,1.,1.,1.,1.,1.,1.,1.,1.,1.,1.,1.,1.,1.,1.,
1.,1.,1.,1.,1.,1.))
REPRESENTATION_ITEM('')
);
#233=(
BOUNDED_CURVE()
B_SPLINE_CURVE(5,(#31759,#31760,#31761,#31762,#31763,#31764,#31765,#31766,
#31767,#31768,#31769,#31770,#31771,#31772,#31773,#31774,#31775,#31776,#31777,
#31778,#31779,#31780,#31781,#31782,#31783,#31784,#31785,#31786,#31787,#31788,
#31789,#31790,#31791,#31792,#31793,#31794,#31795,#31796,#31797,#31798,#31799,
#31800,#31801,#31802,#31803,#31804,#31805,#31806,#31807,#31808,#31809,#31810,
#31811,#31812,#31813,#31814,#31815,#31816,#31817,#31818,#31819,#31820,#31821,
#31822,#31823,#31824,#31825,#31826,#31827,#31828),.UNSPECIFIED.,.F.,.F.)
B_SPLINE_CURVE_WITH_KNOTS((6,1,1,1,1,1,1,1,1,1,1,1,1,1,1,1,1,1,1,1,1,1,
1,1,1,1,1,1,1,1,1,1,1,1,1,1,1,1,1,1,1,1,1,1,1,1,1,1,1,1,1,1,1,1,1,1,1,1,
1,1,1,1,1,1,1,6),(0.0057718433745091,0.0153846153846154,0.0307692307692308,
0.0461538461538462,0.0615384615384615,0.0769230769230769,0.0923076923076923,
0.107692307692308,0.123076923076923,0.138461538461538,0.153846153846154,
0.169230769230769,0.184615384615385,0.2,0.215384615384615,0.230769230769231,
0.246153846153846,0.261538461538462,0.276923076923077,0.292307692307692,
0.307692307692308,0.323076923076923,0.338461538461538,0.353846153846154,
0.369230769230769,0.384615384615385,0.4,0.415384615384615,0.430769230769231,
0.446153846153846,0.461538461538462,0.476923076923077,0.492307692307692,
0.507692307692308,0.523076923076923,0.538461538461538,0.553846153846154,
0.569230769230769,0.584615384615384,0.6,0.615384615384615,0.63076923076923,
0.646153846153846,0.661538461538461,0.676923076923076,0.692307692307692,
0.707692307692307,0.723076923076922,0.738461538461538,0.753846153846153,
0.769230769230768,0.784615384615384,0.799999999999999,0.815384615384614,
0.83076923076923,0.846153846153845,0.86153846153846,0.876923076923076,0.892307692307691,
0.907692307692306,0.923076923076922,0.938461538461537,0.953846153846152,
0.969230769230768,0.984615384615383,1.),.UNSPECIFIED.)
CURVE()
GEOMETRIC_REPRESENTATION_ITEM()
RATIONAL_B_SPLINE_CURVE((1.,1.,1.,1.,1.,1.,1.,1.,1.,1.,1.,1.,1.,1.,1.,1.,
1.,1.,1.,1.,1.,1.,1.,1.,1.,1.,1.,1.,1.,1.,1.,1.,1.,1.,1.,1.,1.,1.,1.,1.,
1.,1.,1.,1.,1.,1.,1.,1.,1.,1.,1.,1.,1.,1.,1.,1.,1.,1.,1.,1.,1.,1.,1.,1.,
1.,1.,1.,1.,1.,1.))
REPRESENTATION_ITEM('')
);
#234=(
BOUNDED_CURVE()
B_SPLINE_CURVE(5,(#31832,#31833,#31834,#31835,#31836,#31837,#31838,#31839,
#31840,#31841,#31842,#31843,#31844,#31845,#31846,#31847,#31848,#31849,#31850,
#31851,#31852,#31853,#31854,#31855,#31856,#31857,#31858,#31859,#31860,#31861,
#31862,#31863,#31864,#31865,#31866,#31867,#31868,#31869,#31870,#31871,#31872,
#31873,#31874,#31875,#31876,#31877,#31878,#31879,#31880,#31881,#31882,#31883,
#31884,#31885,#31886,#31887,#31888,#31889,#31890,#31891,#31892,#31893,#31894,
#31895,#31896,#31897,#31898,#31899,#31900,#31901),.UNSPECIFIED.,.F.,.F.)
B_SPLINE_CURVE_WITH_KNOTS((6,1,1,1,1,1,1,1,1,1,1,1,1,1,1,1,1,1,1,1,1,1,
1,1,1,1,1,1,1,1,1,1,1,1,1,1,1,1,1,1,1,1,1,1,1,1,1,1,1,1,1,1,1,1,1,1,1,1,
1,1,1,1,1,1,1,6),(0.,0.0153846153846154,0.0307692307692308,0.0461538461538462,
0.0615384615384615,0.0769230769230769,0.0923076923076923,0.107692307692308,
0.123076923076923,0.138461538461538,0.153846153846154,0.169230769230769,
0.184615384615385,0.2,0.215384615384615,0.230769230769231,0.246153846153846,
0.261538461538462,0.276923076923077,0.292307692307692,0.307692307692308,
0.323076923076923,0.338461538461538,0.353846153846154,0.369230769230769,
0.384615384615385,0.4,0.415384615384615,0.430769230769231,0.446153846153846,
0.461538461538462,0.476923076923077,0.492307692307692,0.507692307692308,
0.523076923076923,0.538461538461538,0.553846153846154,0.569230769230769,
0.584615384615384,0.6,0.615384615384615,0.63076923076923,0.646153846153846,
0.661538461538461,0.676923076923076,0.692307692307692,0.707692307692307,
0.723076923076922,0.738461538461538,0.753846153846153,0.769230769230768,
0.784615384615384,0.799999999999999,0.815384615384614,0.83076923076923,
0.846153846153845,0.86153846153846,0.876923076923076,0.892307692307691,
0.907692307692306,0.923076923076922,0.938461538461537,0.953846153846152,
0.969230769230768,0.984615384615383,0.994228156739689),.UNSPECIFIED.)
CURVE()
GEOMETRIC_REPRESENTATION_ITEM()
RATIONAL_B_SPLINE_CURVE((1.,1.,1.,1.,1.,1.,1.,1.,1.,1.,1.,1.,1.,1.,1.,1.,
1.,1.,1.,1.,1.,1.,1.,1.,1.,1.,1.,1.,1.,1.,1.,1.,1.,1.,1.,1.,1.,1.,1.,1.,
1.,1.,1.,1.,1.,1.,1.,1.,1.,1.,1.,1.,1.,1.,1.,1.,1.,1.,1.,1.,1.,1.,1.,1.,
1.,1.,1.,1.,1.,1.))
REPRESENTATION_ITEM('')
);
#235=(
BOUNDED_CURVE()
B_SPLINE_CURVE(5,(#31905,#31906,#31907,#31908,#31909,#31910,#31911,#31912,
#31913,#31914,#31915,#31916,#31917,#31918,#31919,#31920,#31921,#31922,#31923,
#31924,#31925,#31926,#31927,#31928,#31929,#31930,#31931,#31932,#31933,#31934,
#31935,#31936,#31937,#31938,#31939,#31940,#31941,#31942,#31943,#31944,#31945,
#31946,#31947,#31948,#31949,#31950,#31951,#31952,#31953,#31954,#31955,#31956,
#31957,#31958,#31959,#31960,#31961,#31962,#31963,#31964,#31965,#31966,#31967,
#31968,#31969,#31970,#31971,#31972,#31973,#31974),.UNSPECIFIED.,.F.,.F.)
B_SPLINE_CURVE_WITH_KNOTS((6,1,1,1,1,1,1,1,1,1,1,1,1,1,1,1,1,1,1,1,1,1,
1,1,1,1,1,1,1,1,1,1,1,1,1,1,1,1,1,1,1,1,1,1,1,1,1,1,1,1,1,1,1,1,1,1,1,1,
1,1,1,1,1,1,1,6),(0.00577184337450777,0.0153846153846154,0.0307692307692308,
0.0461538461538462,0.0615384615384615,0.0769230769230769,0.0923076923076923,
0.107692307692308,0.123076923076923,0.138461538461538,0.153846153846154,
0.169230769230769,0.184615384615385,0.2,0.215384615384615,0.230769230769231,
0.246153846153846,0.261538461538462,0.276923076923077,0.292307692307692,
0.307692307692308,0.323076923076923,0.338461538461538,0.353846153846154,
0.369230769230769,0.384615384615385,0.4,0.415384615384615,0.430769230769231,
0.446153846153846,0.461538461538462,0.476923076923077,0.492307692307692,
0.507692307692308,0.523076923076923,0.538461538461538,0.553846153846154,
0.569230769230769,0.584615384615384,0.6,0.615384615384615,0.63076923076923,
0.646153846153846,0.661538461538461,0.676923076923076,0.692307692307692,
0.707692307692307,0.723076923076922,0.738461538461538,0.753846153846153,
0.769230769230768,0.784615384615384,0.799999999999999,0.815384615384614,
0.83076923076923,0.846153846153845,0.86153846153846,0.876923076923076,0.892307692307691,
0.907692307692306,0.923076923076922,0.938461538461537,0.953846153846152,
0.969230769230768,0.984615384615383,1.),.UNSPECIFIED.)
CURVE()
GEOMETRIC_REPRESENTATION_ITEM()
RATIONAL_B_SPLINE_CURVE((1.,1.,1.,1.,1.,1.,1.,1.,1.,1.,1.,1.,1.,1.,1.,1.,
1.,1.,1.,1.,1.,1.,1.,1.,1.,1.,1.,1.,1.,1.,1.,1.,1.,1.,1.,1.,1.,1.,1.,1.,
1.,1.,1.,1.,1.,1.,1.,1.,1.,1.,1.,1.,1.,1.,1.,1.,1.,1.,1.,1.,1.,1.,1.,1.,
1.,1.,1.,1.,1.,1.))
REPRESENTATION_ITEM('')
);
#236=(
BOUNDED_CURVE()
B_SPLINE_CURVE(5,(#31978,#31979,#31980,#31981,#31982,#31983,#31984,#31985,
#31986,#31987,#31988,#31989,#31990,#31991,#31992,#31993,#31994,#31995,#31996,
#31997,#31998,#31999,#32000,#32001,#32002,#32003,#32004,#32005,#32006,#32007,
#32008,#32009,#32010,#32011,#32012,#32013,#32014,#32015,#32016,#32017,#32018,
#32019,#32020,#32021,#32022,#32023,#32024,#32025,#32026,#32027,#32028,#32029,
#32030,#32031,#32032,#32033,#32034,#32035,#32036,#32037,#32038,#32039,#32040,
#32041,#32042,#32043,#32044,#32045,#32046,#32047),.UNSPECIFIED.,.F.,.F.)
B_SPLINE_CURVE_WITH_KNOTS((6,1,1,1,1,1,1,1,1,1,1,1,1,1,1,1,1,1,1,1,1,1,
1,1,1,1,1,1,1,1,1,1,1,1,1,1,1,1,1,1,1,1,1,1,1,1,1,1,1,1,1,1,1,1,1,1,1,1,
1,1,1,1,1,1,1,6),(0.,0.0153846153846154,0.0307692307692308,0.0461538461538462,
0.0615384615384615,0.0769230769230769,0.0923076923076923,0.107692307692308,
0.123076923076923,0.138461538461538,0.153846153846154,0.169230769230769,
0.184615384615385,0.2,0.215384615384615,0.230769230769231,0.246153846153846,
0.261538461538462,0.276923076923077,0.292307692307692,0.307692307692308,
0.323076923076923,0.338461538461538,0.353846153846154,0.369230769230769,
0.384615384615385,0.4,0.415384615384615,0.430769230769231,0.446153846153846,
0.461538461538462,0.476923076923077,0.492307692307692,0.507692307692308,
0.523076923076923,0.538461538461538,0.553846153846154,0.569230769230769,
0.584615384615384,0.6,0.615384615384615,0.63076923076923,0.646153846153846,
0.661538461538461,0.676923076923076,0.692307692307692,0.707692307692307,
0.723076923076922,0.738461538461538,0.753846153846153,0.769230769230768,
0.784615384615384,0.799999999999999,0.815384615384614,0.83076923076923,
0.846153846153845,0.86153846153846,0.876923076923076,0.892307692307691,
0.907692307692306,0.923076923076922,0.938461538461537,0.953846153846152,
0.969230769230768,0.984615384615383,0.994228156739701),.UNSPECIFIED.)
CURVE()
GEOMETRIC_REPRESENTATION_ITEM()
RATIONAL_B_SPLINE_CURVE((1.,1.,1.,1.,1.,1.,1.,1.,1.,1.,1.,1.,1.,1.,1.,1.,
1.,1.,1.,1.,1.,1.,1.,1.,1.,1.,1.,1.,1.,1.,1.,1.,1.,1.,1.,1.,1.,1.,1.,1.,
1.,1.,1.,1.,1.,1.,1.,1.,1.,1.,1.,1.,1.,1.,1.,1.,1.,1.,1.,1.,1.,1.,1.,1.,
1.,1.,1.,1.,1.,1.))
REPRESENTATION_ITEM('')
);
#237=(
BOUNDED_CURVE()
B_SPLINE_CURVE(5,(#32051,#32052,#32053,#32054,#32055,#32056,#32057,#32058,
#32059,#32060,#32061,#32062,#32063,#32064,#32065,#32066,#32067,#32068,#32069,
#32070,#32071,#32072,#32073,#32074,#32075,#32076,#32077,#32078,#32079,#32080,
#32081,#32082,#32083,#32084,#32085,#32086,#32087,#32088,#32089,#32090,#32091,
#32092,#32093,#32094,#32095,#32096,#32097,#32098,#32099,#32100,#32101,#32102,
#32103,#32104,#32105,#32106,#32107,#32108,#32109,#32110,#32111,#32112,#32113,
#32114,#32115,#32116,#32117,#32118,#32119,#32120),.UNSPECIFIED.,.F.,.F.)
B_SPLINE_CURVE_WITH_KNOTS((6,1,1,1,1,1,1,1,1,1,1,1,1,1,1,1,1,1,1,1,1,1,
1,1,1,1,1,1,1,1,1,1,1,1,1,1,1,1,1,1,1,1,1,1,1,1,1,1,1,1,1,1,1,1,1,1,1,1,
1,1,1,1,1,1,1,6),(0.00577184337450172,0.0153846153846154,0.0307692307692308,
0.0461538461538462,0.0615384615384615,0.0769230769230769,0.0923076923076923,
0.107692307692308,0.123076923076923,0.138461538461538,0.153846153846154,
0.169230769230769,0.184615384615385,0.2,0.215384615384615,0.230769230769231,
0.246153846153846,0.261538461538462,0.276923076923077,0.292307692307692,
0.307692307692308,0.323076923076923,0.338461538461538,0.353846153846154,
0.369230769230769,0.384615384615385,0.4,0.415384615384615,0.430769230769231,
0.446153846153846,0.461538461538462,0.476923076923077,0.492307692307692,
0.507692307692308,0.523076923076923,0.538461538461538,0.553846153846154,
0.569230769230769,0.584615384615384,0.6,0.615384615384615,0.63076923076923,
0.646153846153846,0.661538461538461,0.676923076923076,0.692307692307692,
0.707692307692307,0.723076923076922,0.738461538461538,0.753846153846153,
0.769230769230768,0.784615384615384,0.799999999999999,0.815384615384614,
0.83076923076923,0.846153846153845,0.86153846153846,0.876923076923076,0.892307692307691,
0.907692307692306,0.923076923076922,0.938461538461537,0.953846153846152,
0.969230769230768,0.984615384615383,1.),.UNSPECIFIED.)
CURVE()
GEOMETRIC_REPRESENTATION_ITEM()
RATIONAL_B_SPLINE_CURVE((1.,1.,1.,1.,1.,1.,1.,1.,1.,1.,1.,1.,1.,1.,1.,1.,
1.,1.,1.,1.,1.,1.,1.,1.,1.,1.,1.,1.,1.,1.,1.,1.,1.,1.,1.,1.,1.,1.,1.,1.,
1.,1.,1.,1.,1.,1.,1.,1.,1.,1.,1.,1.,1.,1.,1.,1.,1.,1.,1.,1.,1.,1.,1.,1.,
1.,1.,1.,1.,1.,1.))
REPRESENTATION_ITEM('')
);
#238=(
BOUNDED_CURVE()
B_SPLINE_CURVE(5,(#32124,#32125,#32126,#32127,#32128,#32129,#32130,#32131,
#32132,#32133,#32134,#32135,#32136,#32137,#32138,#32139,#32140,#32141,#32142,
#32143,#32144,#32145,#32146,#32147,#32148,#32149,#32150,#32151,#32152,#32153,
#32154,#32155,#32156,#32157,#32158,#32159,#32160,#32161,#32162,#32163,#32164,
#32165,#32166,#32167,#32168,#32169,#32170,#32171,#32172,#32173,#32174,#32175,
#32176,#32177,#32178,#32179,#32180,#32181,#32182,#32183,#32184,#32185,#32186,
#32187,#32188,#32189,#32190,#32191,#32192,#32193),.UNSPECIFIED.,.F.,.F.)
B_SPLINE_CURVE_WITH_KNOTS((6,1,1,1,1,1,1,1,1,1,1,1,1,1,1,1,1,1,1,1,1,1,
1,1,1,1,1,1,1,1,1,1,1,1,1,1,1,1,1,1,1,1,1,1,1,1,1,1,1,1,1,1,1,1,1,1,1,1,
1,1,1,1,1,1,1,6),(0.,0.0153846153846154,0.0307692307692308,0.0461538461538462,
0.0615384615384615,0.0769230769230769,0.0923076923076923,0.107692307692308,
0.123076923076923,0.138461538461538,0.153846153846154,0.169230769230769,
0.184615384615385,0.2,0.215384615384615,0.230769230769231,0.246153846153846,
0.261538461538462,0.276923076923077,0.292307692307692,0.307692307692308,
0.323076923076923,0.338461538461538,0.353846153846154,0.369230769230769,
0.384615384615385,0.4,0.415384615384615,0.430769230769231,0.446153846153846,
0.461538461538462,0.476923076923077,0.492307692307692,0.507692307692308,
0.523076923076923,0.538461538461538,0.553846153846154,0.569230769230769,
0.584615384615384,0.6,0.615384615384615,0.63076923076923,0.646153846153846,
0.661538461538461,0.676923076923076,0.692307692307692,0.707692307692307,
0.723076923076922,0.738461538461538,0.753846153846153,0.769230769230768,
0.784615384615384,0.799999999999999,0.815384615384614,0.83076923076923,
0.846153846153845,0.86153846153846,0.876923076923076,0.892307692307691,
0.907692307692306,0.923076923076922,0.938461538461537,0.953846153846152,
0.969230769230768,0.984615384615383,0.99422815673971),.UNSPECIFIED.)
CURVE()
GEOMETRIC_REPRESENTATION_ITEM()
RATIONAL_B_SPLINE_CURVE((1.,1.,1.,1.,1.,1.,1.,1.,1.,1.,1.,1.,1.,1.,1.,1.,
1.,1.,1.,1.,1.,1.,1.,1.,1.,1.,1.,1.,1.,1.,1.,1.,1.,1.,1.,1.,1.,1.,1.,1.,
1.,1.,1.,1.,1.,1.,1.,1.,1.,1.,1.,1.,1.,1.,1.,1.,1.,1.,1.,1.,1.,1.,1.,1.,
1.,1.,1.,1.,1.,1.))
REPRESENTATION_ITEM('')
);
#239=(
BOUNDED_CURVE()
B_SPLINE_CURVE(5,(#32197,#32198,#32199,#32200,#32201,#32202,#32203,#32204,
#32205,#32206,#32207,#32208,#32209,#32210,#32211,#32212,#32213,#32214,#32215,
#32216,#32217,#32218,#32219,#32220,#32221,#32222,#32223,#32224,#32225,#32226,
#32227,#32228,#32229,#32230,#32231,#32232,#32233,#32234,#32235,#32236,#32237,
#32238,#32239,#32240,#32241,#32242,#32243,#32244,#32245,#32246,#32247,#32248,
#32249,#32250,#32251,#32252,#32253,#32254,#32255,#32256,#32257,#32258,#32259,
#32260,#32261,#32262,#32263,#32264,#32265,#32266),.UNSPECIFIED.,.F.,.F.)
B_SPLINE_CURVE_WITH_KNOTS((6,1,1,1,1,1,1,1,1,1,1,1,1,1,1,1,1,1,1,1,1,1,
1,1,1,1,1,1,1,1,1,1,1,1,1,1,1,1,1,1,1,1,1,1,1,1,1,1,1,1,1,1,1,1,1,1,1,1,
1,1,1,1,1,1,1,6),(0.00577184337448657,0.0153846153846154,0.0307692307692308,
0.0461538461538462,0.0615384615384615,0.0769230769230769,0.0923076923076923,
0.107692307692308,0.123076923076923,0.138461538461538,0.153846153846154,
0.169230769230769,0.184615384615385,0.2,0.215384615384615,0.230769230769231,
0.246153846153846,0.261538461538462,0.276923076923077,0.292307692307692,
0.307692307692308,0.323076923076923,0.338461538461538,0.353846153846154,
0.369230769230769,0.384615384615385,0.4,0.415384615384615,0.430769230769231,
0.446153846153846,0.461538461538462,0.476923076923077,0.492307692307692,
0.507692307692308,0.523076923076923,0.538461538461538,0.553846153846154,
0.569230769230769,0.584615384615384,0.6,0.615384615384615,0.63076923076923,
0.646153846153846,0.661538461538461,0.676923076923076,0.692307692307692,
0.707692307692307,0.723076923076922,0.738461538461538,0.753846153846153,
0.769230769230768,0.784615384615384,0.799999999999999,0.815384615384614,
0.83076923076923,0.846153846153845,0.86153846153846,0.876923076923076,0.892307692307691,
0.907692307692306,0.923076923076922,0.938461538461537,0.953846153846152,
0.969230769230768,0.984615384615383,1.),.UNSPECIFIED.)
CURVE()
GEOMETRIC_REPRESENTATION_ITEM()
RATIONAL_B_SPLINE_CURVE((1.,1.,1.,1.,1.,1.,1.,1.,1.,1.,1.,1.,1.,1.,1.,1.,
1.,1.,1.,1.,1.,1.,1.,1.,1.,1.,1.,1.,1.,1.,1.,1.,1.,1.,1.,1.,1.,1.,1.,1.,
1.,1.,1.,1.,1.,1.,1.,1.,1.,1.,1.,1.,1.,1.,1.,1.,1.,1.,1.,1.,1.,1.,1.,1.,
1.,1.,1.,1.,1.,1.))
REPRESENTATION_ITEM('')
);
#240=(
BOUNDED_CURVE()
B_SPLINE_CURVE(5,(#32270,#32271,#32272,#32273,#32274,#32275,#32276,#32277,
#32278,#32279,#32280,#32281,#32282,#32283,#32284,#32285,#32286,#32287,#32288,
#32289,#32290,#32291,#32292,#32293,#32294,#32295,#32296,#32297,#32298,#32299,
#32300,#32301,#32302,#32303,#32304,#32305,#32306,#32307,#32308,#32309,#32310,
#32311,#32312,#32313,#32314,#32315,#32316,#32317,#32318,#32319,#32320,#32321,
#32322,#32323,#32324,#32325,#32326,#32327,#32328,#32329,#32330,#32331,#32332,
#32333,#32334,#32335,#32336,#32337,#32338,#32339),.UNSPECIFIED.,.F.,.F.)
B_SPLINE_CURVE_WITH_KNOTS((6,1,1,1,1,1,1,1,1,1,1,1,1,1,1,1,1,1,1,1,1,1,
1,1,1,1,1,1,1,1,1,1,1,1,1,1,1,1,1,1,1,1,1,1,1,1,1,1,1,1,1,1,1,1,1,1,1,1,
1,1,1,1,1,1,1,6),(0.,0.0153846153846154,0.0307692307692308,0.0461538461538462,
0.0615384615384615,0.0769230769230769,0.0923076923076923,0.107692307692308,
0.123076923076923,0.138461538461538,0.153846153846154,0.169230769230769,
0.184615384615385,0.2,0.215384615384615,0.230769230769231,0.246153846153846,
0.261538461538462,0.276923076923077,0.292307692307692,0.307692307692308,
0.323076923076923,0.338461538461538,0.353846153846154,0.369230769230769,
0.384615384615385,0.4,0.415384615384615,0.430769230769231,0.446153846153846,
0.461538461538462,0.476923076923077,0.492307692307692,0.507692307692308,
0.523076923076923,0.538461538461538,0.553846153846154,0.569230769230769,
0.584615384615384,0.6,0.615384615384615,0.63076923076923,0.646153846153846,
0.661538461538461,0.676923076923076,0.692307692307692,0.707692307692307,
0.723076923076922,0.738461538461538,0.753846153846153,0.769230769230768,
0.784615384615384,0.799999999999999,0.815384615384614,0.83076923076923,
0.846153846153845,0.86153846153846,0.876923076923076,0.892307692307691,
0.907692307692306,0.923076923076922,0.938461538461537,0.953846153846152,
0.969230769230768,0.984615384615383,0.994228156739709),.UNSPECIFIED.)
CURVE()
GEOMETRIC_REPRESENTATION_ITEM()
RATIONAL_B_SPLINE_CURVE((1.,1.,1.,1.,1.,1.,1.,1.,1.,1.,1.,1.,1.,1.,1.,1.,
1.,1.,1.,1.,1.,1.,1.,1.,1.,1.,1.,1.,1.,1.,1.,1.,1.,1.,1.,1.,1.,1.,1.,1.,
1.,1.,1.,1.,1.,1.,1.,1.,1.,1.,1.,1.,1.,1.,1.,1.,1.,1.,1.,1.,1.,1.,1.,1.,
1.,1.,1.,1.,1.,1.))
REPRESENTATION_ITEM('')
);
#241=(
BOUNDED_CURVE()
B_SPLINE_CURVE(5,(#32343,#32344,#32345,#32346,#32347,#32348,#32349,#32350,
#32351,#32352,#32353,#32354,#32355,#32356,#32357,#32358,#32359,#32360,#32361,
#32362,#32363,#32364,#32365,#32366,#32367,#32368,#32369,#32370,#32371,#32372,
#32373,#32374,#32375,#32376,#32377,#32378,#32379,#32380,#32381,#32382,#32383,
#32384,#32385,#32386,#32387,#32388,#32389,#32390,#32391,#32392,#32393,#32394,
#32395,#32396,#32397,#32398,#32399,#32400,#32401,#32402,#32403,#32404,#32405,
#32406,#32407,#32408,#32409,#32410,#32411,#32412),.UNSPECIFIED.,.F.,.F.)
B_SPLINE_CURVE_WITH_KNOTS((6,1,1,1,1,1,1,1,1,1,1,1,1,1,1,1,1,1,1,1,1,1,
1,1,1,1,1,1,1,1,1,1,1,1,1,1,1,1,1,1,1,1,1,1,1,1,1,1,1,1,1,1,1,1,1,1,1,1,
1,1,1,1,1,1,1,6),(0.00577184337451094,0.0153846153846154,0.0307692307692308,
0.0461538461538462,0.0615384615384615,0.0769230769230769,0.0923076923076923,
0.107692307692308,0.123076923076923,0.138461538461538,0.153846153846154,
0.169230769230769,0.184615384615385,0.2,0.215384615384615,0.230769230769231,
0.246153846153846,0.261538461538462,0.276923076923077,0.292307692307692,
0.307692307692308,0.323076923076923,0.338461538461538,0.353846153846154,
0.369230769230769,0.384615384615385,0.4,0.415384615384615,0.430769230769231,
0.446153846153846,0.461538461538462,0.476923076923077,0.492307692307692,
0.507692307692308,0.523076923076923,0.538461538461538,0.553846153846154,
0.569230769230769,0.584615384615384,0.6,0.615384615384615,0.63076923076923,
0.646153846153846,0.661538461538461,0.676923076923076,0.692307692307692,
0.707692307692307,0.723076923076922,0.738461538461538,0.753846153846153,
0.769230769230768,0.784615384615384,0.799999999999999,0.815384615384614,
0.83076923076923,0.846153846153845,0.86153846153846,0.876923076923076,0.892307692307691,
0.907692307692306,0.923076923076922,0.938461538461537,0.953846153846152,
0.969230769230768,0.984615384615383,1.),.UNSPECIFIED.)
CURVE()
GEOMETRIC_REPRESENTATION_ITEM()
RATIONAL_B_SPLINE_CURVE((1.,1.,1.,1.,1.,1.,1.,1.,1.,1.,1.,1.,1.,1.,1.,1.,
1.,1.,1.,1.,1.,1.,1.,1.,1.,1.,1.,1.,1.,1.,1.,1.,1.,1.,1.,1.,1.,1.,1.,1.,
1.,1.,1.,1.,1.,1.,1.,1.,1.,1.,1.,1.,1.,1.,1.,1.,1.,1.,1.,1.,1.,1.,1.,1.,
1.,1.,1.,1.,1.,1.))
REPRESENTATION_ITEM('')
);
#242=(
BOUNDED_CURVE()
B_SPLINE_CURVE(5,(#32416,#32417,#32418,#32419,#32420,#32421,#32422,#32423,
#32424,#32425,#32426,#32427,#32428,#32429,#32430,#32431,#32432,#32433,#32434,
#32435,#32436,#32437,#32438,#32439,#32440,#32441,#32442,#32443,#32444,#32445,
#32446,#32447,#32448,#32449,#32450,#32451,#32452,#32453,#32454,#32455,#32456,
#32457,#32458,#32459,#32460,#32461,#32462,#32463,#32464,#32465,#32466,#32467,
#32468,#32469,#32470,#32471,#32472,#32473,#32474,#32475,#32476,#32477,#32478,
#32479,#32480,#32481,#32482,#32483,#32484,#32485),.UNSPECIFIED.,.F.,.F.)
B_SPLINE_CURVE_WITH_KNOTS((6,1,1,1,1,1,1,1,1,1,1,1,1,1,1,1,1,1,1,1,1,1,
1,1,1,1,1,1,1,1,1,1,1,1,1,1,1,1,1,1,1,1,1,1,1,1,1,1,1,1,1,1,1,1,1,1,1,1,
1,1,1,1,1,1,1,6),(0.,0.0153846153846154,0.0307692307692308,0.0461538461538462,
0.0615384615384615,0.0769230769230769,0.0923076923076923,0.107692307692308,
0.123076923076923,0.138461538461538,0.153846153846154,0.169230769230769,
0.184615384615385,0.2,0.215384615384615,0.230769230769231,0.246153846153846,
0.261538461538462,0.276923076923077,0.292307692307692,0.307692307692308,
0.323076923076923,0.338461538461538,0.353846153846154,0.369230769230769,
0.384615384615385,0.4,0.415384615384615,0.430769230769231,0.446153846153846,
0.461538461538462,0.476923076923077,0.492307692307692,0.507692307692308,
0.523076923076923,0.538461538461538,0.553846153846154,0.569230769230769,
0.584615384615384,0.6,0.615384615384615,0.63076923076923,0.646153846153846,
0.661538461538461,0.676923076923076,0.692307692307692,0.707692307692307,
0.723076923076922,0.738461538461538,0.753846153846153,0.769230769230768,
0.784615384615384,0.799999999999999,0.815384615384614,0.83076923076923,
0.846153846153845,0.86153846153846,0.876923076923076,0.892307692307691,
0.907692307692306,0.923076923076922,0.938461538461537,0.953846153846152,
0.969230769230768,0.984615384615383,0.994228156739701),.UNSPECIFIED.)
CURVE()
GEOMETRIC_REPRESENTATION_ITEM()
RATIONAL_B_SPLINE_CURVE((1.,1.,1.,1.,1.,1.,1.,1.,1.,1.,1.,1.,1.,1.,1.,1.,
1.,1.,1.,1.,1.,1.,1.,1.,1.,1.,1.,1.,1.,1.,1.,1.,1.,1.,1.,1.,1.,1.,1.,1.,
1.,1.,1.,1.,1.,1.,1.,1.,1.,1.,1.,1.,1.,1.,1.,1.,1.,1.,1.,1.,1.,1.,1.,1.,
1.,1.,1.,1.,1.,1.))
REPRESENTATION_ITEM('')
);
#243=(
BOUNDED_CURVE()
B_SPLINE_CURVE(5,(#32489,#32490,#32491,#32492,#32493,#32494,#32495,#32496,
#32497,#32498,#32499,#32500,#32501,#32502,#32503,#32504,#32505,#32506,#32507,
#32508,#32509,#32510,#32511,#32512,#32513,#32514,#32515,#32516,#32517,#32518,
#32519,#32520,#32521,#32522,#32523,#32524,#32525,#32526,#32527,#32528,#32529,
#32530,#32531,#32532,#32533,#32534,#32535,#32536,#32537,#32538,#32539,#32540,
#32541,#32542,#32543,#32544,#32545,#32546,#32547,#32548,#32549,#32550,#32551,
#32552,#32553,#32554,#32555,#32556,#32557,#32558),.UNSPECIFIED.,.F.,.F.)
B_SPLINE_CURVE_WITH_KNOTS((6,1,1,1,1,1,1,1,1,1,1,1,1,1,1,1,1,1,1,1,1,1,
1,1,1,1,1,1,1,1,1,1,1,1,1,1,1,1,1,1,1,1,1,1,1,1,1,1,1,1,1,1,1,1,1,1,1,1,
1,1,1,1,1,1,1,6),(0.0057718433745102,0.0153846153846154,0.0307692307692308,
0.0461538461538462,0.0615384615384615,0.0769230769230769,0.0923076923076923,
0.107692307692308,0.123076923076923,0.138461538461538,0.153846153846154,
0.169230769230769,0.184615384615385,0.2,0.215384615384615,0.230769230769231,
0.246153846153846,0.261538461538462,0.276923076923077,0.292307692307692,
0.307692307692308,0.323076923076923,0.338461538461538,0.353846153846154,
0.369230769230769,0.384615384615385,0.4,0.415384615384615,0.430769230769231,
0.446153846153846,0.461538461538462,0.476923076923077,0.492307692307692,
0.507692307692308,0.523076923076923,0.538461538461538,0.553846153846154,
0.569230769230769,0.584615384615384,0.6,0.615384615384615,0.63076923076923,
0.646153846153846,0.661538461538461,0.676923076923076,0.692307692307692,
0.707692307692307,0.723076923076922,0.738461538461538,0.753846153846153,
0.769230769230768,0.784615384615384,0.799999999999999,0.815384615384614,
0.83076923076923,0.846153846153845,0.86153846153846,0.876923076923076,0.892307692307691,
0.907692307692306,0.923076923076922,0.938461538461537,0.953846153846152,
0.969230769230768,0.984615384615383,1.),.UNSPECIFIED.)
CURVE()
GEOMETRIC_REPRESENTATION_ITEM()
RATIONAL_B_SPLINE_CURVE((1.,1.,1.,1.,1.,1.,1.,1.,1.,1.,1.,1.,1.,1.,1.,1.,
1.,1.,1.,1.,1.,1.,1.,1.,1.,1.,1.,1.,1.,1.,1.,1.,1.,1.,1.,1.,1.,1.,1.,1.,
1.,1.,1.,1.,1.,1.,1.,1.,1.,1.,1.,1.,1.,1.,1.,1.,1.,1.,1.,1.,1.,1.,1.,1.,
1.,1.,1.,1.,1.,1.))
REPRESENTATION_ITEM('')
);
#244=(
BOUNDED_CURVE()
B_SPLINE_CURVE(5,(#32562,#32563,#32564,#32565,#32566,#32567,#32568,#32569,
#32570,#32571,#32572,#32573,#32574,#32575,#32576,#32577,#32578,#32579,#32580,
#32581,#32582,#32583,#32584,#32585,#32586,#32587,#32588,#32589,#32590,#32591,
#32592,#32593,#32594,#32595,#32596,#32597,#32598,#32599,#32600,#32601,#32602,
#32603,#32604,#32605,#32606,#32607,#32608,#32609,#32610,#32611,#32612,#32613,
#32614,#32615,#32616,#32617,#32618,#32619,#32620,#32621,#32622,#32623,#32624,
#32625,#32626,#32627,#32628,#32629,#32630,#32631),.UNSPECIFIED.,.F.,.F.)
B_SPLINE_CURVE_WITH_KNOTS((6,1,1,1,1,1,1,1,1,1,1,1,1,1,1,1,1,1,1,1,1,1,
1,1,1,1,1,1,1,1,1,1,1,1,1,1,1,1,1,1,1,1,1,1,1,1,1,1,1,1,1,1,1,1,1,1,1,1,
1,1,1,1,1,1,1,6),(0.,0.0153846153846154,0.0307692307692308,0.0461538461538462,
0.0615384615384615,0.0769230769230769,0.0923076923076923,0.107692307692308,
0.123076923076923,0.138461538461538,0.153846153846154,0.169230769230769,
0.184615384615385,0.2,0.215384615384615,0.230769230769231,0.246153846153846,
0.261538461538462,0.276923076923077,0.292307692307692,0.307692307692308,
0.323076923076923,0.338461538461538,0.353846153846154,0.369230769230769,
0.384615384615385,0.4,0.415384615384615,0.430769230769231,0.446153846153846,
0.461538461538462,0.476923076923077,0.492307692307692,0.507692307692308,
0.523076923076923,0.538461538461538,0.553846153846154,0.569230769230769,
0.584615384615384,0.6,0.615384615384615,0.63076923076923,0.646153846153846,
0.661538461538461,0.676923076923076,0.692307692307692,0.707692307692307,
0.723076923076922,0.738461538461538,0.753846153846153,0.769230769230768,
0.784615384615384,0.799999999999999,0.815384615384614,0.83076923076923,
0.846153846153845,0.86153846153846,0.876923076923076,0.892307692307691,
0.907692307692306,0.923076923076922,0.938461538461537,0.953846153846152,
0.969230769230768,0.984615384615383,0.994228156739694),.UNSPECIFIED.)
CURVE()
GEOMETRIC_REPRESENTATION_ITEM()
RATIONAL_B_SPLINE_CURVE((1.,1.,1.,1.,1.,1.,1.,1.,1.,1.,1.,1.,1.,1.,1.,1.,
1.,1.,1.,1.,1.,1.,1.,1.,1.,1.,1.,1.,1.,1.,1.,1.,1.,1.,1.,1.,1.,1.,1.,1.,
1.,1.,1.,1.,1.,1.,1.,1.,1.,1.,1.,1.,1.,1.,1.,1.,1.,1.,1.,1.,1.,1.,1.,1.,
1.,1.,1.,1.,1.,1.))
REPRESENTATION_ITEM('')
);
#245=(
BOUNDED_CURVE()
B_SPLINE_CURVE(5,(#32635,#32636,#32637,#32638,#32639,#32640,#32641,#32642,
#32643,#32644,#32645,#32646,#32647,#32648,#32649,#32650,#32651,#32652,#32653,
#32654,#32655,#32656,#32657,#32658,#32659,#32660,#32661,#32662,#32663,#32664,
#32665,#32666,#32667,#32668,#32669,#32670,#32671,#32672,#32673,#32674,#32675,
#32676,#32677,#32678,#32679,#32680,#32681,#32682,#32683,#32684,#32685,#32686,
#32687,#32688,#32689,#32690,#32691,#32692,#32693,#32694,#32695,#32696,#32697,
#32698,#32699,#32700,#32701,#32702,#32703,#32704),.UNSPECIFIED.,.F.,.F.)
B_SPLINE_CURVE_WITH_KNOTS((6,1,1,1,1,1,1,1,1,1,1,1,1,1,1,1,1,1,1,1,1,1,
1,1,1,1,1,1,1,1,1,1,1,1,1,1,1,1,1,1,1,1,1,1,1,1,1,1,1,1,1,1,1,1,1,1,1,1,
1,1,1,1,1,1,1,6),(0.00577184337452044,0.0153846153846154,0.0307692307692308,
0.0461538461538462,0.0615384615384615,0.0769230769230769,0.0923076923076923,
0.107692307692308,0.123076923076923,0.138461538461538,0.153846153846154,
0.169230769230769,0.184615384615385,0.2,0.215384615384615,0.230769230769231,
0.246153846153846,0.261538461538462,0.276923076923077,0.292307692307692,
0.307692307692308,0.323076923076923,0.338461538461538,0.353846153846154,
0.369230769230769,0.384615384615385,0.4,0.415384615384615,0.430769230769231,
0.446153846153846,0.461538461538462,0.476923076923077,0.492307692307692,
0.507692307692308,0.523076923076923,0.538461538461538,0.553846153846154,
0.569230769230769,0.584615384615384,0.6,0.615384615384615,0.63076923076923,
0.646153846153846,0.661538461538461,0.676923076923076,0.692307692307692,
0.707692307692307,0.723076923076922,0.738461538461538,0.753846153846153,
0.769230769230768,0.784615384615384,0.799999999999999,0.815384615384614,
0.83076923076923,0.846153846153845,0.86153846153846,0.876923076923076,0.892307692307691,
0.907692307692306,0.923076923076922,0.938461538461537,0.953846153846152,
0.969230769230768,0.984615384615383,1.),.UNSPECIFIED.)
CURVE()
GEOMETRIC_REPRESENTATION_ITEM()
RATIONAL_B_SPLINE_CURVE((1.,1.,1.,1.,1.,1.,1.,1.,1.,1.,1.,1.,1.,1.,1.,1.,
1.,1.,1.,1.,1.,1.,1.,1.,1.,1.,1.,1.,1.,1.,1.,1.,1.,1.,1.,1.,1.,1.,1.,1.,
1.,1.,1.,1.,1.,1.,1.,1.,1.,1.,1.,1.,1.,1.,1.,1.,1.,1.,1.,1.,1.,1.,1.,1.,
1.,1.,1.,1.,1.,1.))
REPRESENTATION_ITEM('')
);
#246=(
BOUNDED_CURVE()
B_SPLINE_CURVE(5,(#32708,#32709,#32710,#32711,#32712,#32713,#32714,#32715,
#32716,#32717,#32718,#32719,#32720,#32721,#32722,#32723,#32724,#32725,#32726,
#32727,#32728,#32729,#32730,#32731,#32732,#32733,#32734,#32735,#32736,#32737,
#32738,#32739,#32740,#32741,#32742,#32743,#32744,#32745,#32746,#32747,#32748,
#32749,#32750,#32751,#32752,#32753,#32754,#32755,#32756,#32757,#32758,#32759,
#32760,#32761,#32762,#32763,#32764,#32765,#32766,#32767,#32768,#32769,#32770,
#32771,#32772,#32773,#32774,#32775,#32776,#32777),.UNSPECIFIED.,.F.,.F.)
B_SPLINE_CURVE_WITH_KNOTS((6,1,1,1,1,1,1,1,1,1,1,1,1,1,1,1,1,1,1,1,1,1,
1,1,1,1,1,1,1,1,1,1,1,1,1,1,1,1,1,1,1,1,1,1,1,1,1,1,1,1,1,1,1,1,1,1,1,1,
1,1,1,1,1,1,1,6),(0.,0.0153846153846154,0.0307692307692308,0.0461538461538462,
0.0615384615384615,0.0769230769230769,0.0923076923076923,0.107692307692308,
0.123076923076923,0.138461538461538,0.153846153846154,0.169230769230769,
0.184615384615385,0.2,0.215384615384615,0.230769230769231,0.246153846153846,
0.261538461538462,0.276923076923077,0.292307692307692,0.307692307692308,
0.323076923076923,0.338461538461538,0.353846153846154,0.369230769230769,
0.384615384615385,0.4,0.415384615384615,0.430769230769231,0.446153846153846,
0.461538461538462,0.476923076923077,0.492307692307692,0.507692307692308,
0.523076923076923,0.538461538461538,0.553846153846154,0.569230769230769,
0.584615384615384,0.6,0.615384615384615,0.63076923076923,0.646153846153846,
0.661538461538461,0.676923076923076,0.692307692307692,0.707692307692307,
0.723076923076922,0.738461538461538,0.753846153846153,0.769230769230768,
0.784615384615384,0.799999999999999,0.815384615384614,0.83076923076923,
0.846153846153845,0.86153846153846,0.876923076923076,0.892307692307691,
0.907692307692306,0.923076923076922,0.938461538461537,0.953846153846152,
0.969230769230768,0.984615384615383,0.994228156739698),.UNSPECIFIED.)
CURVE()
GEOMETRIC_REPRESENTATION_ITEM()
RATIONAL_B_SPLINE_CURVE((1.,1.,1.,1.,1.,1.,1.,1.,1.,1.,1.,1.,1.,1.,1.,1.,
1.,1.,1.,1.,1.,1.,1.,1.,1.,1.,1.,1.,1.,1.,1.,1.,1.,1.,1.,1.,1.,1.,1.,1.,
1.,1.,1.,1.,1.,1.,1.,1.,1.,1.,1.,1.,1.,1.,1.,1.,1.,1.,1.,1.,1.,1.,1.,1.,
1.,1.,1.,1.,1.,1.))
REPRESENTATION_ITEM('')
);
#247=(
BOUNDED_CURVE()
B_SPLINE_CURVE(5,(#32781,#32782,#32783,#32784,#32785,#32786,#32787,#32788,
#32789,#32790,#32791,#32792,#32793,#32794,#32795,#32796,#32797,#32798,#32799,
#32800,#32801,#32802,#32803,#32804,#32805,#32806,#32807,#32808,#32809,#32810,
#32811,#32812,#32813,#32814,#32815,#32816,#32817,#32818,#32819,#32820,#32821,
#32822,#32823,#32824,#32825,#32826,#32827,#32828,#32829,#32830,#32831,#32832,
#32833,#32834,#32835,#32836,#32837,#32838,#32839,#32840,#32841,#32842,#32843,
#32844,#32845,#32846,#32847,#32848,#32849,#32850),.UNSPECIFIED.,.F.,.F.)
B_SPLINE_CURVE_WITH_KNOTS((6,1,1,1,1,1,1,1,1,1,1,1,1,1,1,1,1,1,1,1,1,1,
1,1,1,1,1,1,1,1,1,1,1,1,1,1,1,1,1,1,1,1,1,1,1,1,1,1,1,1,1,1,1,1,1,1,1,1,
1,1,1,1,1,1,1,6),(0.00577184337451607,0.0153846153846154,0.0307692307692308,
0.0461538461538462,0.0615384615384615,0.0769230769230769,0.0923076923076923,
0.107692307692308,0.123076923076923,0.138461538461538,0.153846153846154,
0.169230769230769,0.184615384615385,0.2,0.215384615384615,0.230769230769231,
0.246153846153846,0.261538461538462,0.276923076923077,0.292307692307692,
0.307692307692308,0.323076923076923,0.338461538461538,0.353846153846154,
0.369230769230769,0.384615384615385,0.4,0.415384615384615,0.430769230769231,
0.446153846153846,0.461538461538462,0.476923076923077,0.492307692307692,
0.507692307692308,0.523076923076923,0.538461538461538,0.553846153846154,
0.569230769230769,0.584615384615384,0.6,0.615384615384615,0.63076923076923,
0.646153846153846,0.661538461538461,0.676923076923076,0.692307692307692,
0.707692307692307,0.723076923076922,0.738461538461538,0.753846153846153,
0.769230769230768,0.784615384615384,0.799999999999999,0.815384615384614,
0.83076923076923,0.846153846153845,0.86153846153846,0.876923076923076,0.892307692307691,
0.907692307692306,0.923076923076922,0.938461538461537,0.953846153846152,
0.969230769230768,0.984615384615383,1.),.UNSPECIFIED.)
CURVE()
GEOMETRIC_REPRESENTATION_ITEM()
RATIONAL_B_SPLINE_CURVE((1.,1.,1.,1.,1.,1.,1.,1.,1.,1.,1.,1.,1.,1.,1.,1.,
1.,1.,1.,1.,1.,1.,1.,1.,1.,1.,1.,1.,1.,1.,1.,1.,1.,1.,1.,1.,1.,1.,1.,1.,
1.,1.,1.,1.,1.,1.,1.,1.,1.,1.,1.,1.,1.,1.,1.,1.,1.,1.,1.,1.,1.,1.,1.,1.,
1.,1.,1.,1.,1.,1.))
REPRESENTATION_ITEM('')
);
#248=(
BOUNDED_CURVE()
B_SPLINE_CURVE(5,(#32854,#32855,#32856,#32857,#32858,#32859,#32860,#32861,
#32862,#32863,#32864,#32865,#32866,#32867,#32868,#32869,#32870,#32871,#32872,
#32873,#32874,#32875,#32876,#32877,#32878,#32879,#32880,#32881,#32882,#32883,
#32884,#32885,#32886,#32887,#32888,#32889,#32890,#32891,#32892,#32893,#32894,
#32895,#32896,#32897,#32898,#32899,#32900,#32901,#32902,#32903,#32904,#32905,
#32906,#32907,#32908,#32909,#32910,#32911,#32912,#32913,#32914,#32915,#32916,
#32917,#32918,#32919,#32920,#32921,#32922,#32923),.UNSPECIFIED.,.F.,.F.)
B_SPLINE_CURVE_WITH_KNOTS((6,1,1,1,1,1,1,1,1,1,1,1,1,1,1,1,1,1,1,1,1,1,
1,1,1,1,1,1,1,1,1,1,1,1,1,1,1,1,1,1,1,1,1,1,1,1,1,1,1,1,1,1,1,1,1,1,1,1,
1,1,1,1,1,1,1,6),(0.,0.0153846153846154,0.0307692307692308,0.0461538461538462,
0.0615384615384615,0.0769230769230769,0.0923076923076923,0.107692307692308,
0.123076923076923,0.138461538461538,0.153846153846154,0.169230769230769,
0.184615384615385,0.2,0.215384615384615,0.230769230769231,0.246153846153846,
0.261538461538462,0.276923076923077,0.292307692307692,0.307692307692308,
0.323076923076923,0.338461538461538,0.353846153846154,0.369230769230769,
0.384615384615385,0.4,0.415384615384615,0.430769230769231,0.446153846153846,
0.461538461538462,0.476923076923077,0.492307692307692,0.507692307692308,
0.523076923076923,0.538461538461538,0.553846153846154,0.569230769230769,
0.584615384615384,0.6,0.615384615384615,0.63076923076923,0.646153846153846,
0.661538461538461,0.676923076923076,0.692307692307692,0.707692307692307,
0.723076923076922,0.738461538461538,0.753846153846153,0.769230769230768,
0.784615384615384,0.799999999999999,0.815384615384614,0.83076923076923,
0.846153846153845,0.86153846153846,0.876923076923076,0.892307692307691,
0.907692307692306,0.923076923076922,0.938461538461537,0.953846153846152,
0.969230769230768,0.984615384615383,0.994228156739704),.UNSPECIFIED.)
CURVE()
GEOMETRIC_REPRESENTATION_ITEM()
RATIONAL_B_SPLINE_CURVE((1.,1.,1.,1.,1.,1.,1.,1.,1.,1.,1.,1.,1.,1.,1.,1.,
1.,1.,1.,1.,1.,1.,1.,1.,1.,1.,1.,1.,1.,1.,1.,1.,1.,1.,1.,1.,1.,1.,1.,1.,
1.,1.,1.,1.,1.,1.,1.,1.,1.,1.,1.,1.,1.,1.,1.,1.,1.,1.,1.,1.,1.,1.,1.,1.,
1.,1.,1.,1.,1.,1.))
REPRESENTATION_ITEM('')
);
#249=(
BOUNDED_CURVE()
B_SPLINE_CURVE(5,(#32927,#32928,#32929,#32930,#32931,#32932,#32933,#32934,
#32935,#32936,#32937,#32938,#32939,#32940,#32941,#32942,#32943,#32944,#32945,
#32946,#32947,#32948,#32949,#32950,#32951,#32952,#32953,#32954,#32955,#32956,
#32957,#32958,#32959,#32960,#32961,#32962,#32963,#32964,#32965,#32966,#32967,
#32968,#32969,#32970,#32971,#32972,#32973,#32974,#32975,#32976,#32977,#32978,
#32979,#32980,#32981,#32982,#32983,#32984,#32985,#32986,#32987,#32988,#32989,
#32990,#32991,#32992,#32993,#32994,#32995,#32996),.UNSPECIFIED.,.F.,.F.)
B_SPLINE_CURVE_WITH_KNOTS((6,1,1,1,1,1,1,1,1,1,1,1,1,1,1,1,1,1,1,1,1,1,
1,1,1,1,1,1,1,1,1,1,1,1,1,1,1,1,1,1,1,1,1,1,1,1,1,1,1,1,1,1,1,1,1,1,1,1,
1,1,1,1,1,1,1,6),(0.00577184337449682,0.0153846153846154,0.0307692307692308,
0.0461538461538462,0.0615384615384615,0.0769230769230769,0.0923076923076923,
0.107692307692308,0.123076923076923,0.138461538461538,0.153846153846154,
0.169230769230769,0.184615384615385,0.2,0.215384615384615,0.230769230769231,
0.246153846153846,0.261538461538462,0.276923076923077,0.292307692307692,
0.307692307692308,0.323076923076923,0.338461538461538,0.353846153846154,
0.369230769230769,0.384615384615385,0.4,0.415384615384615,0.430769230769231,
0.446153846153846,0.461538461538462,0.476923076923077,0.492307692307692,
0.507692307692308,0.523076923076923,0.538461538461538,0.553846153846154,
0.569230769230769,0.584615384615384,0.6,0.615384615384615,0.63076923076923,
0.646153846153846,0.661538461538461,0.676923076923076,0.692307692307692,
0.707692307692307,0.723076923076922,0.738461538461538,0.753846153846153,
0.769230769230768,0.784615384615384,0.799999999999999,0.815384615384614,
0.83076923076923,0.846153846153845,0.86153846153846,0.876923076923076,0.892307692307691,
0.907692307692306,0.923076923076922,0.938461538461537,0.953846153846152,
0.969230769230768,0.984615384615383,1.),.UNSPECIFIED.)
CURVE()
GEOMETRIC_REPRESENTATION_ITEM()
RATIONAL_B_SPLINE_CURVE((1.,1.,1.,1.,1.,1.,1.,1.,1.,1.,1.,1.,1.,1.,1.,1.,
1.,1.,1.,1.,1.,1.,1.,1.,1.,1.,1.,1.,1.,1.,1.,1.,1.,1.,1.,1.,1.,1.,1.,1.,
1.,1.,1.,1.,1.,1.,1.,1.,1.,1.,1.,1.,1.,1.,1.,1.,1.,1.,1.,1.,1.,1.,1.,1.,
1.,1.,1.,1.,1.,1.))
REPRESENTATION_ITEM('')
);
#250=(
BOUNDED_CURVE()
B_SPLINE_CURVE(5,(#33000,#33001,#33002,#33003,#33004,#33005,#33006,#33007,
#33008,#33009,#33010,#33011,#33012,#33013,#33014,#33015,#33016,#33017,#33018,
#33019,#33020,#33021,#33022,#33023,#33024,#33025,#33026,#33027,#33028,#33029,
#33030,#33031,#33032,#33033,#33034,#33035,#33036,#33037,#33038,#33039,#33040,
#33041,#33042,#33043,#33044,#33045,#33046,#33047,#33048,#33049,#33050,#33051,
#33052,#33053,#33054,#33055,#33056,#33057,#33058,#33059,#33060,#33061,#33062,
#33063,#33064,#33065,#33066,#33067,#33068,#33069),.UNSPECIFIED.,.F.,.F.)
B_SPLINE_CURVE_WITH_KNOTS((6,1,1,1,1,1,1,1,1,1,1,1,1,1,1,1,1,1,1,1,1,1,
1,1,1,1,1,1,1,1,1,1,1,1,1,1,1,1,1,1,1,1,1,1,1,1,1,1,1,1,1,1,1,1,1,1,1,1,
1,1,1,1,1,1,1,6),(0.,0.0153846153846154,0.0307692307692308,0.0461538461538462,
0.0615384615384615,0.0769230769230769,0.0923076923076923,0.107692307692308,
0.123076923076923,0.138461538461538,0.153846153846154,0.169230769230769,
0.184615384615385,0.2,0.215384615384615,0.230769230769231,0.246153846153846,
0.261538461538462,0.276923076923077,0.292307692307692,0.307692307692308,
0.323076923076923,0.338461538461538,0.353846153846154,0.369230769230769,
0.384615384615385,0.4,0.415384615384615,0.430769230769231,0.446153846153846,
0.461538461538462,0.476923076923077,0.492307692307692,0.507692307692308,
0.523076923076923,0.538461538461538,0.553846153846154,0.569230769230769,
0.584615384615384,0.6,0.615384615384615,0.63076923076923,0.646153846153846,
0.661538461538461,0.676923076923076,0.692307692307692,0.707692307692307,
0.723076923076922,0.738461538461538,0.753846153846153,0.769230769230768,
0.784615384615384,0.799999999999999,0.815384615384614,0.83076923076923,
0.846153846153845,0.86153846153846,0.876923076923076,0.892307692307691,
0.907692307692306,0.923076923076922,0.938461538461537,0.953846153846152,
0.969230769230768,0.984615384615383,0.994228156739711),.UNSPECIFIED.)
CURVE()
GEOMETRIC_REPRESENTATION_ITEM()
RATIONAL_B_SPLINE_CURVE((1.,1.,1.,1.,1.,1.,1.,1.,1.,1.,1.,1.,1.,1.,1.,1.,
1.,1.,1.,1.,1.,1.,1.,1.,1.,1.,1.,1.,1.,1.,1.,1.,1.,1.,1.,1.,1.,1.,1.,1.,
1.,1.,1.,1.,1.,1.,1.,1.,1.,1.,1.,1.,1.,1.,1.,1.,1.,1.,1.,1.,1.,1.,1.,1.,
1.,1.,1.,1.,1.,1.))
REPRESENTATION_ITEM('')
);
#251=(
BOUNDED_CURVE()
B_SPLINE_CURVE(5,(#33073,#33074,#33075,#33076,#33077,#33078,#33079,#33080,
#33081,#33082,#33083,#33084,#33085,#33086,#33087,#33088,#33089,#33090,#33091,
#33092,#33093,#33094,#33095,#33096,#33097,#33098,#33099,#33100,#33101,#33102,
#33103,#33104,#33105,#33106,#33107,#33108,#33109,#33110,#33111,#33112,#33113,
#33114,#33115,#33116,#33117,#33118,#33119,#33120,#33121,#33122,#33123,#33124,
#33125,#33126,#33127,#33128,#33129,#33130,#33131,#33132,#33133,#33134,#33135,
#33136,#33137,#33138,#33139,#33140,#33141,#33142),.UNSPECIFIED.,.F.,.F.)
B_SPLINE_CURVE_WITH_KNOTS((6,1,1,1,1,1,1,1,1,1,1,1,1,1,1,1,1,1,1,1,1,1,
1,1,1,1,1,1,1,1,1,1,1,1,1,1,1,1,1,1,1,1,1,1,1,1,1,1,1,1,1,1,1,1,1,1,1,1,
1,1,1,1,1,1,1,6),(0.00577184337450313,0.0153846153846154,0.0307692307692308,
0.0461538461538462,0.0615384615384615,0.0769230769230769,0.0923076923076923,
0.107692307692308,0.123076923076923,0.138461538461538,0.153846153846154,
0.169230769230769,0.184615384615385,0.2,0.215384615384615,0.230769230769231,
0.246153846153846,0.261538461538462,0.276923076923077,0.292307692307692,
0.307692307692308,0.323076923076923,0.338461538461538,0.353846153846154,
0.369230769230769,0.384615384615385,0.4,0.415384615384615,0.430769230769231,
0.446153846153846,0.461538461538462,0.476923076923077,0.492307692307692,
0.507692307692308,0.523076923076923,0.538461538461538,0.553846153846154,
0.569230769230769,0.584615384615384,0.6,0.615384615384615,0.63076923076923,
0.646153846153846,0.661538461538461,0.676923076923076,0.692307692307692,
0.707692307692307,0.723076923076922,0.738461538461538,0.753846153846153,
0.769230769230768,0.784615384615384,0.799999999999999,0.815384615384614,
0.83076923076923,0.846153846153845,0.86153846153846,0.876923076923076,0.892307692307691,
0.907692307692306,0.923076923076922,0.938461538461537,0.953846153846152,
0.969230769230768,0.984615384615383,1.),.UNSPECIFIED.)
CURVE()
GEOMETRIC_REPRESENTATION_ITEM()
RATIONAL_B_SPLINE_CURVE((1.,1.,1.,1.,1.,1.,1.,1.,1.,1.,1.,1.,1.,1.,1.,1.,
1.,1.,1.,1.,1.,1.,1.,1.,1.,1.,1.,1.,1.,1.,1.,1.,1.,1.,1.,1.,1.,1.,1.,1.,
1.,1.,1.,1.,1.,1.,1.,1.,1.,1.,1.,1.,1.,1.,1.,1.,1.,1.,1.,1.,1.,1.,1.,1.,
1.,1.,1.,1.,1.,1.))
REPRESENTATION_ITEM('')
);
#252=(
BOUNDED_CURVE()
B_SPLINE_CURVE(5,(#33146,#33147,#33148,#33149,#33150,#33151,#33152,#33153,
#33154,#33155,#33156,#33157,#33158,#33159,#33160,#33161,#33162,#33163,#33164,
#33165,#33166,#33167,#33168,#33169,#33170,#33171,#33172,#33173,#33174,#33175,
#33176,#33177,#33178,#33179,#33180,#33181,#33182,#33183,#33184,#33185,#33186,
#33187,#33188,#33189,#33190,#33191,#33192,#33193,#33194,#33195,#33196,#33197,
#33198,#33199,#33200,#33201,#33202,#33203,#33204,#33205,#33206,#33207,#33208,
#33209,#33210,#33211,#33212,#33213,#33214,#33215),.UNSPECIFIED.,.F.,.F.)
B_SPLINE_CURVE_WITH_KNOTS((6,1,1,1,1,1,1,1,1,1,1,1,1,1,1,1,1,1,1,1,1,1,
1,1,1,1,1,1,1,1,1,1,1,1,1,1,1,1,1,1,1,1,1,1,1,1,1,1,1,1,1,1,1,1,1,1,1,1,
1,1,1,1,1,1,1,6),(0.,0.0153846153846154,0.0307692307692308,0.0461538461538462,
0.0615384615384615,0.0769230769230769,0.0923076923076923,0.107692307692308,
0.123076923076923,0.138461538461538,0.153846153846154,0.169230769230769,
0.184615384615385,0.2,0.215384615384615,0.230769230769231,0.246153846153846,
0.261538461538462,0.276923076923077,0.292307692307692,0.307692307692308,
0.323076923076923,0.338461538461538,0.353846153846154,0.369230769230769,
0.384615384615385,0.4,0.415384615384615,0.430769230769231,0.446153846153846,
0.461538461538462,0.476923076923077,0.492307692307692,0.507692307692308,
0.523076923076923,0.538461538461538,0.553846153846154,0.569230769230769,
0.584615384615384,0.6,0.615384615384615,0.63076923076923,0.646153846153846,
0.661538461538461,0.676923076923076,0.692307692307692,0.707692307692307,
0.723076923076922,0.738461538461538,0.753846153846153,0.769230769230768,
0.784615384615384,0.799999999999999,0.815384615384614,0.83076923076923,
0.846153846153845,0.86153846153846,0.876923076923076,0.892307692307691,
0.907692307692306,0.923076923076922,0.938461538461537,0.953846153846152,
0.969230769230768,0.984615384615383,0.9942281567397),.UNSPECIFIED.)
CURVE()
GEOMETRIC_REPRESENTATION_ITEM()
RATIONAL_B_SPLINE_CURVE((1.,1.,1.,1.,1.,1.,1.,1.,1.,1.,1.,1.,1.,1.,1.,1.,
1.,1.,1.,1.,1.,1.,1.,1.,1.,1.,1.,1.,1.,1.,1.,1.,1.,1.,1.,1.,1.,1.,1.,1.,
1.,1.,1.,1.,1.,1.,1.,1.,1.,1.,1.,1.,1.,1.,1.,1.,1.,1.,1.,1.,1.,1.,1.,1.,
1.,1.,1.,1.,1.,1.))
REPRESENTATION_ITEM('')
);
#253=(
BOUNDED_CURVE()
B_SPLINE_CURVE(5,(#33219,#33220,#33221,#33222,#33223,#33224,#33225,#33226,
#33227,#33228,#33229,#33230,#33231,#33232,#33233,#33234,#33235,#33236,#33237,
#33238,#33239,#33240,#33241,#33242,#33243,#33244,#33245,#33246,#33247,#33248,
#33249,#33250,#33251,#33252,#33253,#33254,#33255,#33256,#33257,#33258,#33259,
#33260,#33261,#33262,#33263,#33264,#33265,#33266,#33267,#33268,#33269,#33270,
#33271,#33272,#33273,#33274,#33275,#33276,#33277,#33278,#33279,#33280,#33281,
#33282,#33283,#33284,#33285,#33286,#33287,#33288),.UNSPECIFIED.,.F.,.F.)
B_SPLINE_CURVE_WITH_KNOTS((6,1,1,1,1,1,1,1,1,1,1,1,1,1,1,1,1,1,1,1,1,1,
1,1,1,1,1,1,1,1,1,1,1,1,1,1,1,1,1,1,1,1,1,1,1,1,1,1,1,1,1,1,1,1,1,1,1,1,
1,1,1,1,1,1,1,6),(0.00577184337452087,0.0153846153846154,0.0307692307692308,
0.0461538461538462,0.0615384615384615,0.0769230769230769,0.0923076923076923,
0.107692307692308,0.123076923076923,0.138461538461538,0.153846153846154,
0.169230769230769,0.184615384615385,0.2,0.215384615384615,0.230769230769231,
0.246153846153846,0.261538461538462,0.276923076923077,0.292307692307692,
0.307692307692308,0.323076923076923,0.338461538461538,0.353846153846154,
0.369230769230769,0.384615384615385,0.4,0.415384615384615,0.430769230769231,
0.446153846153846,0.461538461538462,0.476923076923077,0.492307692307692,
0.507692307692308,0.523076923076923,0.538461538461538,0.553846153846154,
0.569230769230769,0.584615384615384,0.6,0.615384615384615,0.63076923076923,
0.646153846153846,0.661538461538461,0.676923076923076,0.692307692307692,
0.707692307692307,0.723076923076922,0.738461538461538,0.753846153846153,
0.769230769230768,0.784615384615384,0.799999999999999,0.815384615384614,
0.83076923076923,0.846153846153845,0.86153846153846,0.876923076923076,0.892307692307691,
0.907692307692306,0.923076923076922,0.938461538461537,0.953846153846152,
0.969230769230768,0.984615384615383,1.),.UNSPECIFIED.)
CURVE()
GEOMETRIC_REPRESENTATION_ITEM()
RATIONAL_B_SPLINE_CURVE((1.,1.,1.,1.,1.,1.,1.,1.,1.,1.,1.,1.,1.,1.,1.,1.,
1.,1.,1.,1.,1.,1.,1.,1.,1.,1.,1.,1.,1.,1.,1.,1.,1.,1.,1.,1.,1.,1.,1.,1.,
1.,1.,1.,1.,1.,1.,1.,1.,1.,1.,1.,1.,1.,1.,1.,1.,1.,1.,1.,1.,1.,1.,1.,1.,
1.,1.,1.,1.,1.,1.))
REPRESENTATION_ITEM('')
);
#254=(
BOUNDED_CURVE()
B_SPLINE_CURVE(5,(#33292,#33293,#33294,#33295,#33296,#33297,#33298,#33299,
#33300,#33301,#33302,#33303,#33304,#33305,#33306,#33307,#33308,#33309,#33310,
#33311,#33312,#33313,#33314,#33315,#33316,#33317,#33318,#33319,#33320,#33321,
#33322,#33323,#33324,#33325,#33326,#33327,#33328,#33329,#33330,#33331,#33332,
#33333,#33334,#33335,#33336,#33337,#33338,#33339,#33340,#33341,#33342,#33343,
#33344,#33345,#33346,#33347,#33348,#33349,#33350,#33351,#33352,#33353,#33354,
#33355,#33356,#33357,#33358,#33359,#33360,#33361),.UNSPECIFIED.,.F.,.F.)
B_SPLINE_CURVE_WITH_KNOTS((6,1,1,1,1,1,1,1,1,1,1,1,1,1,1,1,1,1,1,1,1,1,
1,1,1,1,1,1,1,1,1,1,1,1,1,1,1,1,1,1,1,1,1,1,1,1,1,1,1,1,1,1,1,1,1,1,1,1,
1,1,1,1,1,1,1,6),(0.,0.0153846153846154,0.0307692307692308,0.0461538461538462,
0.0615384615384615,0.0769230769230769,0.0923076923076923,0.107692307692308,
0.123076923076923,0.138461538461538,0.153846153846154,0.169230769230769,
0.184615384615385,0.2,0.215384615384615,0.230769230769231,0.246153846153846,
0.261538461538462,0.276923076923077,0.292307692307692,0.307692307692308,
0.323076923076923,0.338461538461538,0.353846153846154,0.369230769230769,
0.384615384615385,0.4,0.415384615384615,0.430769230769231,0.446153846153846,
0.461538461538462,0.476923076923077,0.492307692307692,0.507692307692308,
0.523076923076923,0.538461538461538,0.553846153846154,0.569230769230769,
0.584615384615384,0.6,0.615384615384615,0.63076923076923,0.646153846153846,
0.661538461538461,0.676923076923076,0.692307692307692,0.707692307692307,
0.723076923076922,0.738461538461538,0.753846153846153,0.769230769230768,
0.784615384615384,0.799999999999999,0.815384615384614,0.83076923076923,
0.846153846153845,0.86153846153846,0.876923076923076,0.892307692307691,
0.907692307692306,0.923076923076922,0.938461538461537,0.953846153846152,
0.969230769230768,0.984615384615383,0.994228156739692),.UNSPECIFIED.)
CURVE()
GEOMETRIC_REPRESENTATION_ITEM()
RATIONAL_B_SPLINE_CURVE((1.,1.,1.,1.,1.,1.,1.,1.,1.,1.,1.,1.,1.,1.,1.,1.,
1.,1.,1.,1.,1.,1.,1.,1.,1.,1.,1.,1.,1.,1.,1.,1.,1.,1.,1.,1.,1.,1.,1.,1.,
1.,1.,1.,1.,1.,1.,1.,1.,1.,1.,1.,1.,1.,1.,1.,1.,1.,1.,1.,1.,1.,1.,1.,1.,
1.,1.,1.,1.,1.,1.))
REPRESENTATION_ITEM('')
);
#255=(
BOUNDED_CURVE()
B_SPLINE_CURVE(5,(#33365,#33366,#33367,#33368,#33369,#33370,#33371,#33372,
#33373,#33374,#33375,#33376,#33377,#33378,#33379,#33380,#33381,#33382,#33383,
#33384,#33385,#33386,#33387,#33388,#33389,#33390,#33391,#33392,#33393,#33394,
#33395,#33396,#33397,#33398,#33399,#33400,#33401,#33402,#33403,#33404,#33405,
#33406,#33407,#33408,#33409,#33410,#33411,#33412,#33413,#33414,#33415,#33416,
#33417,#33418,#33419,#33420,#33421,#33422,#33423,#33424,#33425,#33426,#33427,
#33428,#33429,#33430,#33431,#33432,#33433,#33434),.UNSPECIFIED.,.F.,.F.)
B_SPLINE_CURVE_WITH_KNOTS((6,1,1,1,1,1,1,1,1,1,1,1,1,1,1,1,1,1,1,1,1,1,
1,1,1,1,1,1,1,1,1,1,1,1,1,1,1,1,1,1,1,1,1,1,1,1,1,1,1,1,1,1,1,1,1,1,1,1,
1,1,1,1,1,1,1,6),(0.00577184337450777,0.0153846153846154,0.0307692307692308,
0.0461538461538462,0.0615384615384615,0.0769230769230769,0.0923076923076923,
0.107692307692308,0.123076923076923,0.138461538461538,0.153846153846154,
0.169230769230769,0.184615384615385,0.2,0.215384615384615,0.230769230769231,
0.246153846153846,0.261538461538462,0.276923076923077,0.292307692307692,
0.307692307692308,0.323076923076923,0.338461538461538,0.353846153846154,
0.369230769230769,0.384615384615385,0.4,0.415384615384615,0.430769230769231,
0.446153846153846,0.461538461538462,0.476923076923077,0.492307692307692,
0.507692307692308,0.523076923076923,0.538461538461538,0.553846153846154,
0.569230769230769,0.584615384615384,0.6,0.615384615384615,0.63076923076923,
0.646153846153846,0.661538461538461,0.676923076923076,0.692307692307692,
0.707692307692307,0.723076923076922,0.738461538461538,0.753846153846153,
0.769230769230768,0.784615384615384,0.799999999999999,0.815384615384614,
0.83076923076923,0.846153846153845,0.86153846153846,0.876923076923076,0.892307692307691,
0.907692307692306,0.923076923076922,0.938461538461537,0.953846153846152,
0.969230769230768,0.984615384615383,1.),.UNSPECIFIED.)
CURVE()
GEOMETRIC_REPRESENTATION_ITEM()
RATIONAL_B_SPLINE_CURVE((1.,1.,1.,1.,1.,1.,1.,1.,1.,1.,1.,1.,1.,1.,1.,1.,
1.,1.,1.,1.,1.,1.,1.,1.,1.,1.,1.,1.,1.,1.,1.,1.,1.,1.,1.,1.,1.,1.,1.,1.,
1.,1.,1.,1.,1.,1.,1.,1.,1.,1.,1.,1.,1.,1.,1.,1.,1.,1.,1.,1.,1.,1.,1.,1.,
1.,1.,1.,1.,1.,1.))
REPRESENTATION_ITEM('')
);
#256=(
BOUNDED_CURVE()
B_SPLINE_CURVE(5,(#33438,#33439,#33440,#33441,#33442,#33443,#33444,#33445,
#33446,#33447,#33448,#33449,#33450,#33451,#33452,#33453,#33454,#33455,#33456,
#33457,#33458,#33459,#33460,#33461,#33462,#33463,#33464,#33465,#33466,#33467,
#33468,#33469,#33470,#33471,#33472,#33473,#33474,#33475,#33476,#33477,#33478,
#33479,#33480,#33481,#33482,#33483,#33484,#33485,#33486,#33487,#33488,#33489,
#33490,#33491,#33492,#33493,#33494,#33495,#33496,#33497,#33498,#33499,#33500,
#33501,#33502,#33503,#33504,#33505,#33506,#33507),.UNSPECIFIED.,.F.,.F.)
B_SPLINE_CURVE_WITH_KNOTS((6,1,1,1,1,1,1,1,1,1,1,1,1,1,1,1,1,1,1,1,1,1,
1,1,1,1,1,1,1,1,1,1,1,1,1,1,1,1,1,1,1,1,1,1,1,1,1,1,1,1,1,1,1,1,1,1,1,1,
1,1,1,1,1,1,1,6),(0.,0.0153846153846154,0.0307692307692308,0.0461538461538462,
0.0615384615384615,0.0769230769230769,0.0923076923076923,0.107692307692308,
0.123076923076923,0.138461538461538,0.153846153846154,0.169230769230769,
0.184615384615385,0.2,0.215384615384615,0.230769230769231,0.246153846153846,
0.261538461538462,0.276923076923077,0.292307692307692,0.307692307692308,
0.323076923076923,0.338461538461538,0.353846153846154,0.369230769230769,
0.384615384615385,0.4,0.415384615384615,0.430769230769231,0.446153846153846,
0.461538461538462,0.476923076923077,0.492307692307692,0.507692307692308,
0.523076923076923,0.538461538461538,0.553846153846154,0.569230769230769,
0.584615384615384,0.6,0.615384615384615,0.63076923076923,0.646153846153846,
0.661538461538461,0.676923076923076,0.692307692307692,0.707692307692307,
0.723076923076922,0.738461538461538,0.753846153846153,0.769230769230768,
0.784615384615384,0.799999999999999,0.815384615384614,0.83076923076923,
0.846153846153845,0.86153846153846,0.876923076923076,0.892307692307691,
0.907692307692306,0.923076923076922,0.938461538461537,0.953846153846152,
0.969230769230768,0.984615384615383,0.994228156739701),.UNSPECIFIED.)
CURVE()
GEOMETRIC_REPRESENTATION_ITEM()
RATIONAL_B_SPLINE_CURVE((1.,1.,1.,1.,1.,1.,1.,1.,1.,1.,1.,1.,1.,1.,1.,1.,
1.,1.,1.,1.,1.,1.,1.,1.,1.,1.,1.,1.,1.,1.,1.,1.,1.,1.,1.,1.,1.,1.,1.,1.,
1.,1.,1.,1.,1.,1.,1.,1.,1.,1.,1.,1.,1.,1.,1.,1.,1.,1.,1.,1.,1.,1.,1.,1.,
1.,1.,1.,1.,1.,1.))
REPRESENTATION_ITEM('')
);
#257=(
BOUNDED_CURVE()
B_SPLINE_CURVE(5,(#33511,#33512,#33513,#33514,#33515,#33516,#33517,#33518,
#33519,#33520,#33521,#33522,#33523,#33524,#33525,#33526,#33527,#33528,#33529,
#33530,#33531,#33532,#33533,#33534,#33535,#33536,#33537,#33538,#33539,#33540,
#33541,#33542,#33543,#33544,#33545,#33546,#33547,#33548,#33549,#33550,#33551,
#33552,#33553,#33554,#33555,#33556,#33557,#33558,#33559,#33560,#33561,#33562,
#33563,#33564,#33565,#33566,#33567,#33568,#33569,#33570,#33571,#33572,#33573,
#33574,#33575,#33576,#33577,#33578,#33579,#33580),.UNSPECIFIED.,.F.,.F.)
B_SPLINE_CURVE_WITH_KNOTS((6,1,1,1,1,1,1,1,1,1,1,1,1,1,1,1,1,1,1,1,1,1,
1,1,1,1,1,1,1,1,1,1,1,1,1,1,1,1,1,1,1,1,1,1,1,1,1,1,1,1,1,1,1,1,1,1,1,1,
1,1,1,1,1,1,1,6),(0.00577184337450943,0.0153846153846154,0.0307692307692308,
0.0461538461538462,0.0615384615384615,0.0769230769230769,0.0923076923076923,
0.107692307692308,0.123076923076923,0.138461538461538,0.153846153846154,
0.169230769230769,0.184615384615385,0.2,0.215384615384615,0.230769230769231,
0.246153846153846,0.261538461538462,0.276923076923077,0.292307692307692,
0.307692307692308,0.323076923076923,0.338461538461538,0.353846153846154,
0.369230769230769,0.384615384615385,0.4,0.415384615384615,0.430769230769231,
0.446153846153846,0.461538461538462,0.476923076923077,0.492307692307692,
0.507692307692308,0.523076923076923,0.538461538461538,0.553846153846154,
0.569230769230769,0.584615384615384,0.6,0.615384615384615,0.63076923076923,
0.646153846153846,0.661538461538461,0.676923076923076,0.692307692307692,
0.707692307692307,0.723076923076922,0.738461538461538,0.753846153846153,
0.769230769230768,0.784615384615384,0.799999999999999,0.815384615384614,
0.83076923076923,0.846153846153845,0.86153846153846,0.876923076923076,0.892307692307691,
0.907692307692306,0.923076923076922,0.938461538461537,0.953846153846152,
0.969230769230768,0.984615384615383,1.),.UNSPECIFIED.)
CURVE()
GEOMETRIC_REPRESENTATION_ITEM()
RATIONAL_B_SPLINE_CURVE((1.,1.,1.,1.,1.,1.,1.,1.,1.,1.,1.,1.,1.,1.,1.,1.,
1.,1.,1.,1.,1.,1.,1.,1.,1.,1.,1.,1.,1.,1.,1.,1.,1.,1.,1.,1.,1.,1.,1.,1.,
1.,1.,1.,1.,1.,1.,1.,1.,1.,1.,1.,1.,1.,1.,1.,1.,1.,1.,1.,1.,1.,1.,1.,1.,
1.,1.,1.,1.,1.,1.))
REPRESENTATION_ITEM('')
);
#258=(
BOUNDED_CURVE()
B_SPLINE_CURVE(5,(#33584,#33585,#33586,#33587,#33588,#33589,#33590,#33591,
#33592,#33593,#33594,#33595,#33596,#33597,#33598,#33599,#33600,#33601,#33602,
#33603,#33604,#33605,#33606,#33607,#33608,#33609,#33610,#33611,#33612,#33613,
#33614,#33615,#33616,#33617,#33618,#33619,#33620,#33621,#33622,#33623,#33624,
#33625,#33626,#33627,#33628,#33629,#33630,#33631,#33632,#33633,#33634,#33635,
#33636,#33637,#33638,#33639,#33640,#33641,#33642,#33643,#33644,#33645,#33646,
#33647,#33648,#33649,#33650,#33651,#33652,#33653),.UNSPECIFIED.,.F.,.F.)
B_SPLINE_CURVE_WITH_KNOTS((6,1,1,1,1,1,1,1,1,1,1,1,1,1,1,1,1,1,1,1,1,1,
1,1,1,1,1,1,1,1,1,1,1,1,1,1,1,1,1,1,1,1,1,1,1,1,1,1,1,1,1,1,1,1,1,1,1,1,
1,1,1,1,1,1,1,6),(0.,0.0153846153846154,0.0307692307692308,0.0461538461538462,
0.0615384615384615,0.0769230769230769,0.0923076923076923,0.107692307692308,
0.123076923076923,0.138461538461538,0.153846153846154,0.169230769230769,
0.184615384615385,0.2,0.215384615384615,0.230769230769231,0.246153846153846,
0.261538461538462,0.276923076923077,0.292307692307692,0.307692307692308,
0.323076923076923,0.338461538461538,0.353846153846154,0.369230769230769,
0.384615384615385,0.4,0.415384615384615,0.430769230769231,0.446153846153846,
0.461538461538462,0.476923076923077,0.492307692307692,0.507692307692308,
0.523076923076923,0.538461538461538,0.553846153846154,0.569230769230769,
0.584615384615384,0.6,0.615384615384615,0.63076923076923,0.646153846153846,
0.661538461538461,0.676923076923076,0.692307692307692,0.707692307692307,
0.723076923076922,0.738461538461538,0.753846153846153,0.769230769230768,
0.784615384615384,0.799999999999999,0.815384615384614,0.83076923076923,
0.846153846153845,0.86153846153846,0.876923076923076,0.892307692307691,
0.907692307692306,0.923076923076922,0.938461538461537,0.953846153846152,
0.969230769230768,0.984615384615383,0.994228156739699),.UNSPECIFIED.)
CURVE()
GEOMETRIC_REPRESENTATION_ITEM()
RATIONAL_B_SPLINE_CURVE((1.,1.,1.,1.,1.,1.,1.,1.,1.,1.,1.,1.,1.,1.,1.,1.,
1.,1.,1.,1.,1.,1.,1.,1.,1.,1.,1.,1.,1.,1.,1.,1.,1.,1.,1.,1.,1.,1.,1.,1.,
1.,1.,1.,1.,1.,1.,1.,1.,1.,1.,1.,1.,1.,1.,1.,1.,1.,1.,1.,1.,1.,1.,1.,1.,
1.,1.,1.,1.,1.,1.))
REPRESENTATION_ITEM('')
);
#259=(
BOUNDED_CURVE()
B_SPLINE_CURVE(5,(#33657,#33658,#33659,#33660,#33661,#33662,#33663,#33664,
#33665,#33666,#33667,#33668,#33669,#33670,#33671,#33672,#33673,#33674,#33675,
#33676,#33677,#33678,#33679,#33680,#33681,#33682,#33683,#33684,#33685,#33686,
#33687,#33688,#33689,#33690,#33691,#33692,#33693,#33694,#33695,#33696,#33697,
#33698,#33699,#33700,#33701,#33702,#33703,#33704,#33705,#33706,#33707,#33708,
#33709,#33710,#33711,#33712,#33713,#33714,#33715,#33716,#33717,#33718,#33719,
#33720,#33721,#33722,#33723,#33724,#33725,#33726),.UNSPECIFIED.,.F.,.F.)
B_SPLINE_CURVE_WITH_KNOTS((6,1,1,1,1,1,1,1,1,1,1,1,1,1,1,1,1,1,1,1,1,1,
1,1,1,1,1,1,1,1,1,1,1,1,1,1,1,1,1,1,1,1,1,1,1,1,1,1,1,1,1,1,1,1,1,1,1,1,
1,1,1,1,1,1,1,6),(0.00577184337448657,0.0153846153846154,0.0307692307692308,
0.0461538461538462,0.0615384615384615,0.0769230769230769,0.0923076923076923,
0.107692307692308,0.123076923076923,0.138461538461538,0.153846153846154,
0.169230769230769,0.184615384615385,0.2,0.215384615384615,0.230769230769231,
0.246153846153846,0.261538461538462,0.276923076923077,0.292307692307692,
0.307692307692308,0.323076923076923,0.338461538461538,0.353846153846154,
0.369230769230769,0.384615384615385,0.4,0.415384615384615,0.430769230769231,
0.446153846153846,0.461538461538462,0.476923076923077,0.492307692307692,
0.507692307692308,0.523076923076923,0.538461538461538,0.553846153846154,
0.569230769230769,0.584615384615384,0.6,0.615384615384615,0.63076923076923,
0.646153846153846,0.661538461538461,0.676923076923076,0.692307692307692,
0.707692307692307,0.723076923076922,0.738461538461538,0.753846153846153,
0.769230769230768,0.784615384615384,0.799999999999999,0.815384615384614,
0.83076923076923,0.846153846153845,0.86153846153846,0.876923076923076,0.892307692307691,
0.907692307692306,0.923076923076922,0.938461538461537,0.953846153846152,
0.969230769230768,0.984615384615383,1.),.UNSPECIFIED.)
CURVE()
GEOMETRIC_REPRESENTATION_ITEM()
RATIONAL_B_SPLINE_CURVE((1.,1.,1.,1.,1.,1.,1.,1.,1.,1.,1.,1.,1.,1.,1.,1.,
1.,1.,1.,1.,1.,1.,1.,1.,1.,1.,1.,1.,1.,1.,1.,1.,1.,1.,1.,1.,1.,1.,1.,1.,
1.,1.,1.,1.,1.,1.,1.,1.,1.,1.,1.,1.,1.,1.,1.,1.,1.,1.,1.,1.,1.,1.,1.,1.,
1.,1.,1.,1.,1.,1.))
REPRESENTATION_ITEM('')
);
#260=(
BOUNDED_CURVE()
B_SPLINE_CURVE(5,(#33730,#33731,#33732,#33733,#33734,#33735,#33736,#33737,
#33738,#33739,#33740,#33741,#33742,#33743,#33744,#33745,#33746,#33747,#33748,
#33749,#33750,#33751,#33752,#33753,#33754,#33755,#33756,#33757,#33758,#33759,
#33760,#33761,#33762,#33763,#33764,#33765,#33766,#33767,#33768,#33769,#33770,
#33771,#33772,#33773,#33774,#33775,#33776,#33777,#33778,#33779,#33780,#33781,
#33782,#33783,#33784,#33785,#33786,#33787,#33788,#33789,#33790,#33791,#33792,
#33793,#33794,#33795,#33796,#33797,#33798,#33799),.UNSPECIFIED.,.F.,.F.)
B_SPLINE_CURVE_WITH_KNOTS((6,1,1,1,1,1,1,1,1,1,1,1,1,1,1,1,1,1,1,1,1,1,
1,1,1,1,1,1,1,1,1,1,1,1,1,1,1,1,1,1,1,1,1,1,1,1,1,1,1,1,1,1,1,1,1,1,1,1,
1,1,1,1,1,1,1,6),(0.,0.0153846153846154,0.0307692307692308,0.0461538461538462,
0.0615384615384615,0.0769230769230769,0.0923076923076923,0.107692307692308,
0.123076923076923,0.138461538461538,0.153846153846154,0.169230769230769,
0.184615384615385,0.2,0.215384615384615,0.230769230769231,0.246153846153846,
0.261538461538462,0.276923076923077,0.292307692307692,0.307692307692308,
0.323076923076923,0.338461538461538,0.353846153846154,0.369230769230769,
0.384615384615385,0.4,0.415384615384615,0.430769230769231,0.446153846153846,
0.461538461538462,0.476923076923077,0.492307692307692,0.507692307692308,
0.523076923076923,0.538461538461538,0.553846153846154,0.569230769230769,
0.584615384615384,0.6,0.615384615384615,0.63076923076923,0.646153846153846,
0.661538461538461,0.676923076923076,0.692307692307692,0.707692307692307,
0.723076923076922,0.738461538461538,0.753846153846153,0.769230769230768,
0.784615384615384,0.799999999999999,0.815384615384614,0.83076923076923,
0.846153846153845,0.86153846153846,0.876923076923076,0.892307692307691,
0.907692307692306,0.923076923076922,0.938461538461537,0.953846153846152,
0.969230769230768,0.984615384615383,0.994228156739709),.UNSPECIFIED.)
CURVE()
GEOMETRIC_REPRESENTATION_ITEM()
RATIONAL_B_SPLINE_CURVE((1.,1.,1.,1.,1.,1.,1.,1.,1.,1.,1.,1.,1.,1.,1.,1.,
1.,1.,1.,1.,1.,1.,1.,1.,1.,1.,1.,1.,1.,1.,1.,1.,1.,1.,1.,1.,1.,1.,1.,1.,
1.,1.,1.,1.,1.,1.,1.,1.,1.,1.,1.,1.,1.,1.,1.,1.,1.,1.,1.,1.,1.,1.,1.,1.,
1.,1.,1.,1.,1.,1.))
REPRESENTATION_ITEM('')
);
#261=(
BOUNDED_CURVE()
B_SPLINE_CURVE(5,(#33803,#33804,#33805,#33806,#33807,#33808,#33809,#33810,
#33811,#33812,#33813,#33814,#33815,#33816,#33817,#33818,#33819,#33820,#33821,
#33822,#33823,#33824,#33825,#33826,#33827,#33828,#33829,#33830,#33831,#33832,
#33833,#33834,#33835,#33836,#33837,#33838,#33839,#33840,#33841,#33842,#33843,
#33844,#33845,#33846,#33847,#33848,#33849,#33850,#33851,#33852,#33853,#33854,
#33855,#33856,#33857,#33858,#33859,#33860,#33861,#33862,#33863,#33864,#33865,
#33866,#33867,#33868,#33869,#33870,#33871,#33872),.UNSPECIFIED.,.F.,.F.)
B_SPLINE_CURVE_WITH_KNOTS((6,1,1,1,1,1,1,1,1,1,1,1,1,1,1,1,1,1,1,1,1,1,
1,1,1,1,1,1,1,1,1,1,1,1,1,1,1,1,1,1,1,1,1,1,1,1,1,1,1,1,1,1,1,1,1,1,1,1,
1,1,1,1,1,1,1,6),(0.00577184337451132,0.0153846153846154,0.0307692307692308,
0.0461538461538462,0.0615384615384615,0.0769230769230769,0.0923076923076923,
0.107692307692308,0.123076923076923,0.138461538461538,0.153846153846154,
0.169230769230769,0.184615384615385,0.2,0.215384615384615,0.230769230769231,
0.246153846153846,0.261538461538462,0.276923076923077,0.292307692307692,
0.307692307692308,0.323076923076923,0.338461538461538,0.353846153846154,
0.369230769230769,0.384615384615385,0.4,0.415384615384615,0.430769230769231,
0.446153846153846,0.461538461538462,0.476923076923077,0.492307692307692,
0.507692307692308,0.523076923076923,0.538461538461538,0.553846153846154,
0.569230769230769,0.584615384615384,0.6,0.615384615384615,0.63076923076923,
0.646153846153846,0.661538461538461,0.676923076923076,0.692307692307692,
0.707692307692307,0.723076923076922,0.738461538461538,0.753846153846153,
0.769230769230768,0.784615384615384,0.799999999999999,0.815384615384614,
0.83076923076923,0.846153846153845,0.86153846153846,0.876923076923076,0.892307692307691,
0.907692307692306,0.923076923076922,0.938461538461537,0.953846153846152,
0.969230769230768,0.984615384615383,1.),.UNSPECIFIED.)
CURVE()
GEOMETRIC_REPRESENTATION_ITEM()
RATIONAL_B_SPLINE_CURVE((1.,1.,1.,1.,1.,1.,1.,1.,1.,1.,1.,1.,1.,1.,1.,1.,
1.,1.,1.,1.,1.,1.,1.,1.,1.,1.,1.,1.,1.,1.,1.,1.,1.,1.,1.,1.,1.,1.,1.,1.,
1.,1.,1.,1.,1.,1.,1.,1.,1.,1.,1.,1.,1.,1.,1.,1.,1.,1.,1.,1.,1.,1.,1.,1.,
1.,1.,1.,1.,1.,1.))
REPRESENTATION_ITEM('')
);
#262=(
BOUNDED_CURVE()
B_SPLINE_CURVE(5,(#33876,#33877,#33878,#33879,#33880,#33881,#33882,#33883,
#33884,#33885,#33886,#33887,#33888,#33889,#33890,#33891,#33892,#33893,#33894,
#33895,#33896,#33897,#33898,#33899,#33900,#33901,#33902,#33903,#33904,#33905,
#33906,#33907,#33908,#33909,#33910,#33911,#33912,#33913,#33914,#33915,#33916,
#33917,#33918,#33919,#33920,#33921,#33922,#33923,#33924,#33925,#33926,#33927,
#33928,#33929,#33930,#33931,#33932,#33933,#33934,#33935,#33936,#33937,#33938,
#33939,#33940,#33941,#33942,#33943,#33944,#33945),.UNSPECIFIED.,.F.,.F.)
B_SPLINE_CURVE_WITH_KNOTS((6,1,1,1,1,1,1,1,1,1,1,1,1,1,1,1,1,1,1,1,1,1,
1,1,1,1,1,1,1,1,1,1,1,1,1,1,1,1,1,1,1,1,1,1,1,1,1,1,1,1,1,1,1,1,1,1,1,1,
1,1,1,1,1,1,1,6),(0.,0.0153846153846154,0.0307692307692308,0.0461538461538462,
0.0615384615384615,0.0769230769230769,0.0923076923076923,0.107692307692308,
0.123076923076923,0.138461538461538,0.153846153846154,0.169230769230769,
0.184615384615385,0.2,0.215384615384615,0.230769230769231,0.246153846153846,
0.261538461538462,0.276923076923077,0.292307692307692,0.307692307692308,
0.323076923076923,0.338461538461538,0.353846153846154,0.369230769230769,
0.384615384615385,0.4,0.415384615384615,0.430769230769231,0.446153846153846,
0.461538461538462,0.476923076923077,0.492307692307692,0.507692307692308,
0.523076923076923,0.538461538461538,0.553846153846154,0.569230769230769,
0.584615384615384,0.6,0.615384615384615,0.63076923076923,0.646153846153846,
0.661538461538461,0.676923076923076,0.692307692307692,0.707692307692307,
0.723076923076922,0.738461538461538,0.753846153846153,0.769230769230768,
0.784615384615384,0.799999999999999,0.815384615384614,0.83076923076923,
0.846153846153845,0.86153846153846,0.876923076923076,0.892307692307691,
0.907692307692306,0.923076923076922,0.938461538461537,0.953846153846152,
0.969230769230768,0.984615384615383,0.994228156739705),.UNSPECIFIED.)
CURVE()
GEOMETRIC_REPRESENTATION_ITEM()
RATIONAL_B_SPLINE_CURVE((1.,1.,1.,1.,1.,1.,1.,1.,1.,1.,1.,1.,1.,1.,1.,1.,
1.,1.,1.,1.,1.,1.,1.,1.,1.,1.,1.,1.,1.,1.,1.,1.,1.,1.,1.,1.,1.,1.,1.,1.,
1.,1.,1.,1.,1.,1.,1.,1.,1.,1.,1.,1.,1.,1.,1.,1.,1.,1.,1.,1.,1.,1.,1.,1.,
1.,1.,1.,1.,1.,1.))
REPRESENTATION_ITEM('')
);
#263=(
BOUNDED_CURVE()
B_SPLINE_CURVE(5,(#33949,#33950,#33951,#33952,#33953,#33954,#33955,#33956,
#33957,#33958,#33959,#33960,#33961,#33962,#33963,#33964,#33965,#33966,#33967,
#33968,#33969,#33970,#33971,#33972,#33973,#33974,#33975,#33976,#33977,#33978,
#33979,#33980,#33981,#33982,#33983,#33984,#33985,#33986,#33987,#33988,#33989,
#33990,#33991,#33992,#33993,#33994,#33995,#33996,#33997,#33998,#33999,#34000,
#34001,#34002,#34003,#34004,#34005,#34006,#34007,#34008,#34009,#34010,#34011,
#34012,#34013,#34014,#34015,#34016,#34017,#34018),.UNSPECIFIED.,.F.,.F.)
B_SPLINE_CURVE_WITH_KNOTS((6,1,1,1,1,1,1,1,1,1,1,1,1,1,1,1,1,1,1,1,1,1,
1,1,1,1,1,1,1,1,1,1,1,1,1,1,1,1,1,1,1,1,1,1,1,1,1,1,1,1,1,1,1,1,1,1,1,1,
1,1,1,1,1,1,1,6),(0.00577184337450072,0.0153846153846154,0.0307692307692308,
0.0461538461538462,0.0615384615384615,0.0769230769230769,0.0923076923076923,
0.107692307692308,0.123076923076923,0.138461538461538,0.153846153846154,
0.169230769230769,0.184615384615385,0.2,0.215384615384615,0.230769230769231,
0.246153846153846,0.261538461538462,0.276923076923077,0.292307692307692,
0.307692307692308,0.323076923076923,0.338461538461538,0.353846153846154,
0.369230769230769,0.384615384615385,0.4,0.415384615384615,0.430769230769231,
0.446153846153846,0.461538461538462,0.476923076923077,0.492307692307692,
0.507692307692308,0.523076923076923,0.538461538461538,0.553846153846154,
0.569230769230769,0.584615384615384,0.6,0.615384615384615,0.63076923076923,
0.646153846153846,0.661538461538461,0.676923076923076,0.692307692307692,
0.707692307692307,0.723076923076922,0.738461538461538,0.753846153846153,
0.769230769230768,0.784615384615384,0.799999999999999,0.815384615384614,
0.83076923076923,0.846153846153845,0.86153846153846,0.876923076923076,0.892307692307691,
0.907692307692306,0.923076923076922,0.938461538461537,0.953846153846152,
0.969230769230768,0.984615384615383,1.),.UNSPECIFIED.)
CURVE()
GEOMETRIC_REPRESENTATION_ITEM()
RATIONAL_B_SPLINE_CURVE((1.,1.,1.,1.,1.,1.,1.,1.,1.,1.,1.,1.,1.,1.,1.,1.,
1.,1.,1.,1.,1.,1.,1.,1.,1.,1.,1.,1.,1.,1.,1.,1.,1.,1.,1.,1.,1.,1.,1.,1.,
1.,1.,1.,1.,1.,1.,1.,1.,1.,1.,1.,1.,1.,1.,1.,1.,1.,1.,1.,1.,1.,1.,1.,1.,
1.,1.,1.,1.,1.,1.))
REPRESENTATION_ITEM('')
);
#264=(
BOUNDED_CURVE()
B_SPLINE_CURVE(5,(#34022,#34023,#34024,#34025,#34026,#34027,#34028,#34029,
#34030,#34031,#34032,#34033,#34034,#34035,#34036,#34037,#34038,#34039,#34040,
#34041,#34042,#34043,#34044,#34045,#34046,#34047,#34048,#34049,#34050,#34051,
#34052,#34053,#34054,#34055,#34056,#34057,#34058,#34059,#34060,#34061,#34062,
#34063,#34064,#34065,#34066,#34067,#34068,#34069,#34070,#34071,#34072,#34073,
#34074,#34075,#34076,#34077,#34078,#34079,#34080,#34081,#34082,#34083,#34084,
#34085,#34086,#34087,#34088,#34089,#34090,#34091),.UNSPECIFIED.,.F.,.F.)
B_SPLINE_CURVE_WITH_KNOTS((6,1,1,1,1,1,1,1,1,1,1,1,1,1,1,1,1,1,1,1,1,1,
1,1,1,1,1,1,1,1,1,1,1,1,1,1,1,1,1,1,1,1,1,1,1,1,1,1,1,1,1,1,1,1,1,1,1,1,
1,1,1,1,1,1,1,6),(0.,0.0153846153846154,0.0307692307692308,0.0461538461538462,
0.0615384615384615,0.0769230769230769,0.0923076923076923,0.107692307692308,
0.123076923076923,0.138461538461538,0.153846153846154,0.169230769230769,
0.184615384615385,0.2,0.215384615384615,0.230769230769231,0.246153846153846,
0.261538461538462,0.276923076923077,0.292307692307692,0.307692307692308,
0.323076923076923,0.338461538461538,0.353846153846154,0.369230769230769,
0.384615384615385,0.4,0.415384615384615,0.430769230769231,0.446153846153846,
0.461538461538462,0.476923076923077,0.492307692307692,0.507692307692308,
0.523076923076923,0.538461538461538,0.553846153846154,0.569230769230769,
0.584615384615384,0.6,0.615384615384615,0.63076923076923,0.646153846153846,
0.661538461538461,0.676923076923076,0.692307692307692,0.707692307692307,
0.723076923076922,0.738461538461538,0.753846153846153,0.769230769230768,
0.784615384615384,0.799999999999999,0.815384615384614,0.83076923076923,
0.846153846153845,0.86153846153846,0.876923076923076,0.892307692307691,
0.907692307692306,0.923076923076922,0.938461538461537,0.953846153846152,
0.969230769230768,0.984615384615383,0.994228156739706),.UNSPECIFIED.)
CURVE()
GEOMETRIC_REPRESENTATION_ITEM()
RATIONAL_B_SPLINE_CURVE((1.,1.,1.,1.,1.,1.,1.,1.,1.,1.,1.,1.,1.,1.,1.,1.,
1.,1.,1.,1.,1.,1.,1.,1.,1.,1.,1.,1.,1.,1.,1.,1.,1.,1.,1.,1.,1.,1.,1.,1.,
1.,1.,1.,1.,1.,1.,1.,1.,1.,1.,1.,1.,1.,1.,1.,1.,1.,1.,1.,1.,1.,1.,1.,1.,
1.,1.,1.,1.,1.,1.))
REPRESENTATION_ITEM('')
);
#265=(
BOUNDED_CURVE()
B_SPLINE_CURVE(5,(#34095,#34096,#34097,#34098,#34099,#34100,#34101,#34102,
#34103,#34104,#34105,#34106,#34107,#34108,#34109,#34110,#34111,#34112,#34113,
#34114,#34115,#34116,#34117,#34118,#34119,#34120,#34121,#34122,#34123,#34124,
#34125,#34126,#34127,#34128,#34129,#34130,#34131,#34132,#34133,#34134,#34135,
#34136,#34137,#34138,#34139,#34140,#34141,#34142,#34143,#34144,#34145,#34146,
#34147,#34148,#34149,#34150,#34151,#34152,#34153,#34154,#34155,#34156,#34157,
#34158,#34159,#34160,#34161,#34162,#34163,#34164),.UNSPECIFIED.,.F.,.F.)
B_SPLINE_CURVE_WITH_KNOTS((6,1,1,1,1,1,1,1,1,1,1,1,1,1,1,1,1,1,1,1,1,1,
1,1,1,1,1,1,1,1,1,1,1,1,1,1,1,1,1,1,1,1,1,1,1,1,1,1,1,1,1,1,1,1,1,1,1,1,
1,1,1,1,1,1,1,6),(0.00577184337450902,0.0153846153846154,0.0307692307692308,
0.0461538461538462,0.0615384615384615,0.0769230769230769,0.0923076923076923,
0.107692307692308,0.123076923076923,0.138461538461538,0.153846153846154,
0.169230769230769,0.184615384615385,0.2,0.215384615384615,0.230769230769231,
0.246153846153846,0.261538461538462,0.276923076923077,0.292307692307692,
0.307692307692308,0.323076923076923,0.338461538461538,0.353846153846154,
0.369230769230769,0.384615384615385,0.4,0.415384615384615,0.430769230769231,
0.446153846153846,0.461538461538462,0.476923076923077,0.492307692307692,
0.507692307692308,0.523076923076923,0.538461538461538,0.553846153846154,
0.569230769230769,0.584615384615384,0.6,0.615384615384615,0.63076923076923,
0.646153846153846,0.661538461538461,0.676923076923076,0.692307692307692,
0.707692307692307,0.723076923076922,0.738461538461538,0.753846153846153,
0.769230769230768,0.784615384615384,0.799999999999999,0.815384615384614,
0.83076923076923,0.846153846153845,0.86153846153846,0.876923076923076,0.892307692307691,
0.907692307692306,0.923076923076922,0.938461538461537,0.953846153846152,
0.969230769230768,0.984615384615383,1.),.UNSPECIFIED.)
CURVE()
GEOMETRIC_REPRESENTATION_ITEM()
RATIONAL_B_SPLINE_CURVE((1.,1.,1.,1.,1.,1.,1.,1.,1.,1.,1.,1.,1.,1.,1.,1.,
1.,1.,1.,1.,1.,1.,1.,1.,1.,1.,1.,1.,1.,1.,1.,1.,1.,1.,1.,1.,1.,1.,1.,1.,
1.,1.,1.,1.,1.,1.,1.,1.,1.,1.,1.,1.,1.,1.,1.,1.,1.,1.,1.,1.,1.,1.,1.,1.,
1.,1.,1.,1.,1.,1.))
REPRESENTATION_ITEM('')
);
#266=(
BOUNDED_CURVE()
B_SPLINE_CURVE(5,(#34168,#34169,#34170,#34171,#34172,#34173,#34174,#34175,
#34176,#34177,#34178,#34179,#34180,#34181,#34182,#34183,#34184,#34185,#34186,
#34187,#34188,#34189,#34190,#34191,#34192,#34193,#34194,#34195,#34196,#34197,
#34198,#34199,#34200,#34201,#34202,#34203,#34204,#34205,#34206,#34207,#34208,
#34209,#34210,#34211,#34212,#34213,#34214,#34215,#34216,#34217,#34218,#34219,
#34220,#34221,#34222,#34223,#34224,#34225,#34226,#34227,#34228,#34229,#34230,
#34231,#34232,#34233,#34234,#34235,#34236,#34237),.UNSPECIFIED.,.F.,.F.)
B_SPLINE_CURVE_WITH_KNOTS((6,1,1,1,1,1,1,1,1,1,1,1,1,1,1,1,1,1,1,1,1,1,
1,1,1,1,1,1,1,1,1,1,1,1,1,1,1,1,1,1,1,1,1,1,1,1,1,1,1,1,1,1,1,1,1,1,1,1,
1,1,1,1,1,1,1,6),(0.,0.0153846153846154,0.0307692307692308,0.0461538461538462,
0.0615384615384615,0.0769230769230769,0.0923076923076923,0.107692307692308,
0.123076923076923,0.138461538461538,0.153846153846154,0.169230769230769,
0.184615384615385,0.2,0.215384615384615,0.230769230769231,0.246153846153846,
0.261538461538462,0.276923076923077,0.292307692307692,0.307692307692308,
0.323076923076923,0.338461538461538,0.353846153846154,0.369230769230769,
0.384615384615385,0.4,0.415384615384615,0.430769230769231,0.446153846153846,
0.461538461538462,0.476923076923077,0.492307692307692,0.507692307692308,
0.523076923076923,0.538461538461538,0.553846153846154,0.569230769230769,
0.584615384615384,0.6,0.615384615384615,0.63076923076923,0.646153846153846,
0.661538461538461,0.676923076923076,0.692307692307692,0.707692307692307,
0.723076923076922,0.738461538461538,0.753846153846153,0.769230769230768,
0.784615384615384,0.799999999999999,0.815384615384614,0.83076923076923,
0.846153846153845,0.86153846153846,0.876923076923076,0.892307692307691,
0.907692307692306,0.923076923076922,0.938461538461537,0.953846153846152,
0.969230769230768,0.984615384615383,0.994228156739698),.UNSPECIFIED.)
CURVE()
GEOMETRIC_REPRESENTATION_ITEM()
RATIONAL_B_SPLINE_CURVE((1.,1.,1.,1.,1.,1.,1.,1.,1.,1.,1.,1.,1.,1.,1.,1.,
1.,1.,1.,1.,1.,1.,1.,1.,1.,1.,1.,1.,1.,1.,1.,1.,1.,1.,1.,1.,1.,1.,1.,1.,
1.,1.,1.,1.,1.,1.,1.,1.,1.,1.,1.,1.,1.,1.,1.,1.,1.,1.,1.,1.,1.,1.,1.,1.,
1.,1.,1.,1.,1.,1.))
REPRESENTATION_ITEM('')
);
#267=(
BOUNDED_CURVE()
B_SPLINE_CURVE(5,(#34241,#34242,#34243,#34244,#34245,#34246,#34247,#34248,
#34249,#34250,#34251,#34252,#34253,#34254,#34255,#34256,#34257,#34258,#34259,
#34260,#34261,#34262,#34263,#34264,#34265,#34266,#34267,#34268,#34269,#34270,
#34271,#34272,#34273,#34274,#34275,#34276,#34277,#34278,#34279,#34280,#34281,
#34282,#34283,#34284,#34285,#34286,#34287,#34288,#34289,#34290,#34291,#34292,
#34293,#34294,#34295,#34296,#34297,#34298,#34299,#34300,#34301,#34302,#34303,
#34304,#34305,#34306,#34307,#34308,#34309,#34310),.UNSPECIFIED.,.F.,.F.)
B_SPLINE_CURVE_WITH_KNOTS((6,1,1,1,1,1,1,1,1,1,1,1,1,1,1,1,1,1,1,1,1,1,
1,1,1,1,1,1,1,1,1,1,1,1,1,1,1,1,1,1,1,1,1,1,1,1,1,1,1,1,1,1,1,1,1,1,1,1,
1,1,1,1,1,1,1,6),(0.00577184337451611,0.0153846153846154,0.0307692307692308,
0.0461538461538462,0.0615384615384615,0.0769230769230769,0.0923076923076923,
0.107692307692308,0.123076923076923,0.138461538461538,0.153846153846154,
0.169230769230769,0.184615384615385,0.2,0.215384615384615,0.230769230769231,
0.246153846153846,0.261538461538462,0.276923076923077,0.292307692307692,
0.307692307692308,0.323076923076923,0.338461538461538,0.353846153846154,
0.369230769230769,0.384615384615385,0.4,0.415384615384615,0.430769230769231,
0.446153846153846,0.461538461538462,0.476923076923077,0.492307692307692,
0.507692307692308,0.523076923076923,0.538461538461538,0.553846153846154,
0.569230769230769,0.584615384615384,0.6,0.615384615384615,0.63076923076923,
0.646153846153846,0.661538461538461,0.676923076923076,0.692307692307692,
0.707692307692307,0.723076923076922,0.738461538461538,0.753846153846153,
0.769230769230768,0.784615384615384,0.799999999999999,0.815384615384614,
0.83076923076923,0.846153846153845,0.86153846153846,0.876923076923076,0.892307692307691,
0.907692307692306,0.923076923076922,0.938461538461537,0.953846153846152,
0.969230769230768,0.984615384615383,1.),.UNSPECIFIED.)
CURVE()
GEOMETRIC_REPRESENTATION_ITEM()
RATIONAL_B_SPLINE_CURVE((1.,1.,1.,1.,1.,1.,1.,1.,1.,1.,1.,1.,1.,1.,1.,1.,
1.,1.,1.,1.,1.,1.,1.,1.,1.,1.,1.,1.,1.,1.,1.,1.,1.,1.,1.,1.,1.,1.,1.,1.,
1.,1.,1.,1.,1.,1.,1.,1.,1.,1.,1.,1.,1.,1.,1.,1.,1.,1.,1.,1.,1.,1.,1.,1.,
1.,1.,1.,1.,1.,1.))
REPRESENTATION_ITEM('')
);
#268=(
BOUNDED_CURVE()
B_SPLINE_CURVE(5,(#34314,#34315,#34316,#34317,#34318,#34319,#34320,#34321,
#34322,#34323,#34324,#34325,#34326,#34327,#34328,#34329,#34330,#34331,#34332,
#34333,#34334,#34335,#34336,#34337,#34338,#34339,#34340,#34341,#34342,#34343,
#34344,#34345,#34346,#34347,#34348,#34349,#34350,#34351,#34352,#34353,#34354,
#34355,#34356,#34357,#34358,#34359,#34360,#34361,#34362,#34363,#34364,#34365,
#34366,#34367,#34368,#34369,#34370,#34371,#34372,#34373,#34374,#34375,#34376,
#34377,#34378,#34379,#34380,#34381,#34382,#34383),.UNSPECIFIED.,.F.,.F.)
B_SPLINE_CURVE_WITH_KNOTS((6,1,1,1,1,1,1,1,1,1,1,1,1,1,1,1,1,1,1,1,1,1,
1,1,1,1,1,1,1,1,1,1,1,1,1,1,1,1,1,1,1,1,1,1,1,1,1,1,1,1,1,1,1,1,1,1,1,1,
1,1,1,1,1,1,1,6),(0.,0.0153846153846154,0.0307692307692308,0.0461538461538462,
0.0615384615384615,0.0769230769230769,0.0923076923076923,0.107692307692308,
0.123076923076923,0.138461538461538,0.153846153846154,0.169230769230769,
0.184615384615385,0.2,0.215384615384615,0.230769230769231,0.246153846153846,
0.261538461538462,0.276923076923077,0.292307692307692,0.307692307692308,
0.323076923076923,0.338461538461538,0.353846153846154,0.369230769230769,
0.384615384615385,0.4,0.415384615384615,0.430769230769231,0.446153846153846,
0.461538461538462,0.476923076923077,0.492307692307692,0.507692307692308,
0.523076923076923,0.538461538461538,0.553846153846154,0.569230769230769,
0.584615384615384,0.6,0.615384615384615,0.63076923076923,0.646153846153846,
0.661538461538461,0.676923076923076,0.692307692307692,0.707692307692307,
0.723076923076922,0.738461538461538,0.753846153846153,0.769230769230768,
0.784615384615384,0.799999999999999,0.815384615384614,0.83076923076923,
0.846153846153845,0.86153846153846,0.876923076923076,0.892307692307691,
0.907692307692306,0.923076923076922,0.938461538461537,0.953846153846152,
0.969230769230768,0.984615384615383,0.994228156739704),.UNSPECIFIED.)
CURVE()
GEOMETRIC_REPRESENTATION_ITEM()
RATIONAL_B_SPLINE_CURVE((1.,1.,1.,1.,1.,1.,1.,1.,1.,1.,1.,1.,1.,1.,1.,1.,
1.,1.,1.,1.,1.,1.,1.,1.,1.,1.,1.,1.,1.,1.,1.,1.,1.,1.,1.,1.,1.,1.,1.,1.,
1.,1.,1.,1.,1.,1.,1.,1.,1.,1.,1.,1.,1.,1.,1.,1.,1.,1.,1.,1.,1.,1.,1.,1.,
1.,1.,1.,1.,1.,1.))
REPRESENTATION_ITEM('')
);
#269=(
BOUNDED_CURVE()
B_SPLINE_CURVE(5,(#34387,#34388,#34389,#34390,#34391,#34392,#34393,#34394,
#34395,#34396,#34397,#34398,#34399,#34400,#34401,#34402,#34403,#34404,#34405,
#34406,#34407,#34408,#34409,#34410,#34411,#34412,#34413,#34414,#34415,#34416,
#34417,#34418,#34419,#34420,#34421,#34422,#34423,#34424,#34425,#34426,#34427,
#34428,#34429,#34430,#34431,#34432,#34433,#34434,#34435,#34436,#34437,#34438,
#34439,#34440,#34441,#34442,#34443,#34444,#34445,#34446,#34447,#34448,#34449,
#34450,#34451,#34452,#34453,#34454,#34455,#34456),.UNSPECIFIED.,.F.,.F.)
B_SPLINE_CURVE_WITH_KNOTS((6,1,1,1,1,1,1,1,1,1,1,1,1,1,1,1,1,1,1,1,1,1,
1,1,1,1,1,1,1,1,1,1,1,1,1,1,1,1,1,1,1,1,1,1,1,1,1,1,1,1,1,1,1,1,1,1,1,1,
1,1,1,1,1,1,1,6),(0.00577184337449682,0.0153846153846154,0.0307692307692308,
0.0461538461538462,0.0615384615384615,0.0769230769230769,0.0923076923076923,
0.107692307692308,0.123076923076923,0.138461538461538,0.153846153846154,
0.169230769230769,0.184615384615385,0.2,0.215384615384615,0.230769230769231,
0.246153846153846,0.261538461538462,0.276923076923077,0.292307692307692,
0.307692307692308,0.323076923076923,0.338461538461538,0.353846153846154,
0.369230769230769,0.384615384615385,0.4,0.415384615384615,0.430769230769231,
0.446153846153846,0.461538461538462,0.476923076923077,0.492307692307692,
0.507692307692308,0.523076923076923,0.538461538461538,0.553846153846154,
0.569230769230769,0.584615384615384,0.6,0.615384615384615,0.63076923076923,
0.646153846153846,0.661538461538461,0.676923076923076,0.692307692307692,
0.707692307692307,0.723076923076922,0.738461538461538,0.753846153846153,
0.769230769230768,0.784615384615384,0.799999999999999,0.815384615384614,
0.83076923076923,0.846153846153845,0.86153846153846,0.876923076923076,0.892307692307691,
0.907692307692306,0.923076923076922,0.938461538461537,0.953846153846152,
0.969230769230768,0.984615384615383,1.),.UNSPECIFIED.)
CURVE()
GEOMETRIC_REPRESENTATION_ITEM()
RATIONAL_B_SPLINE_CURVE((1.,1.,1.,1.,1.,1.,1.,1.,1.,1.,1.,1.,1.,1.,1.,1.,
1.,1.,1.,1.,1.,1.,1.,1.,1.,1.,1.,1.,1.,1.,1.,1.,1.,1.,1.,1.,1.,1.,1.,1.,
1.,1.,1.,1.,1.,1.,1.,1.,1.,1.,1.,1.,1.,1.,1.,1.,1.,1.,1.,1.,1.,1.,1.,1.,
1.,1.,1.,1.,1.,1.))
REPRESENTATION_ITEM('')
);
#270=(
BOUNDED_CURVE()
B_SPLINE_CURVE(5,(#34460,#34461,#34462,#34463,#34464,#34465,#34466,#34467,
#34468,#34469,#34470,#34471,#34472,#34473,#34474,#34475,#34476,#34477,#34478,
#34479,#34480,#34481,#34482,#34483,#34484,#34485,#34486,#34487,#34488,#34489,
#34490,#34491,#34492,#34493,#34494,#34495,#34496,#34497,#34498,#34499,#34500,
#34501,#34502,#34503,#34504,#34505,#34506,#34507,#34508,#34509,#34510,#34511,
#34512,#34513,#34514,#34515,#34516,#34517,#34518,#34519,#34520,#34521,#34522,
#34523,#34524,#34525,#34526,#34527,#34528,#34529),.UNSPECIFIED.,.F.,.F.)
B_SPLINE_CURVE_WITH_KNOTS((6,1,1,1,1,1,1,1,1,1,1,1,1,1,1,1,1,1,1,1,1,1,
1,1,1,1,1,1,1,1,1,1,1,1,1,1,1,1,1,1,1,1,1,1,1,1,1,1,1,1,1,1,1,1,1,1,1,1,
1,1,1,1,1,1,1,6),(0.,0.0153846153846154,0.0307692307692308,0.0461538461538462,
0.0615384615384615,0.0769230769230769,0.0923076923076923,0.107692307692308,
0.123076923076923,0.138461538461538,0.153846153846154,0.169230769230769,
0.184615384615385,0.2,0.215384615384615,0.230769230769231,0.246153846153846,
0.261538461538462,0.276923076923077,0.292307692307692,0.307692307692308,
0.323076923076923,0.338461538461538,0.353846153846154,0.369230769230769,
0.384615384615385,0.4,0.415384615384615,0.430769230769231,0.446153846153846,
0.461538461538462,0.476923076923077,0.492307692307692,0.507692307692308,
0.523076923076923,0.538461538461538,0.553846153846154,0.569230769230769,
0.584615384615384,0.6,0.615384615384615,0.63076923076923,0.646153846153846,
0.661538461538461,0.676923076923076,0.692307692307692,0.707692307692307,
0.723076923076922,0.738461538461538,0.753846153846153,0.769230769230768,
0.784615384615384,0.799999999999999,0.815384615384614,0.83076923076923,
0.846153846153845,0.86153846153846,0.876923076923076,0.892307692307691,
0.907692307692306,0.923076923076922,0.938461538461537,0.953846153846152,
0.969230769230768,0.984615384615383,0.994228156739711),.UNSPECIFIED.)
CURVE()
GEOMETRIC_REPRESENTATION_ITEM()
RATIONAL_B_SPLINE_CURVE((1.,1.,1.,1.,1.,1.,1.,1.,1.,1.,1.,1.,1.,1.,1.,1.,
1.,1.,1.,1.,1.,1.,1.,1.,1.,1.,1.,1.,1.,1.,1.,1.,1.,1.,1.,1.,1.,1.,1.,1.,
1.,1.,1.,1.,1.,1.,1.,1.,1.,1.,1.,1.,1.,1.,1.,1.,1.,1.,1.,1.,1.,1.,1.,1.,
1.,1.,1.,1.,1.,1.))
REPRESENTATION_ITEM('')
);
#271=(
BOUNDED_CURVE()
B_SPLINE_CURVE(5,(#34533,#34534,#34535,#34536,#34537,#34538,#34539,#34540,
#34541,#34542,#34543,#34544,#34545,#34546,#34547,#34548,#34549,#34550,#34551,
#34552,#34553,#34554,#34555,#34556,#34557,#34558,#34559,#34560,#34561,#34562,
#34563,#34564,#34565,#34566,#34567,#34568,#34569,#34570,#34571,#34572,#34573,
#34574,#34575,#34576,#34577,#34578,#34579,#34580,#34581,#34582,#34583,#34584,
#34585,#34586,#34587,#34588,#34589,#34590,#34591,#34592,#34593,#34594,#34595,
#34596,#34597,#34598,#34599,#34600,#34601,#34602),.UNSPECIFIED.,.F.,.F.)
B_SPLINE_CURVE_WITH_KNOTS((6,1,1,1,1,1,1,1,1,1,1,1,1,1,1,1,1,1,1,1,1,1,
1,1,1,1,1,1,1,1,1,1,1,1,1,1,1,1,1,1,1,1,1,1,1,1,1,1,1,1,1,1,1,1,1,1,1,1,
1,1,1,1,1,1,1,6),(0.00577184337449159,0.0153846153846154,0.0307692307692308,
0.0461538461538462,0.0615384615384615,0.0769230769230769,0.0923076923076923,
0.107692307692308,0.123076923076923,0.138461538461538,0.153846153846154,
0.169230769230769,0.184615384615385,0.2,0.215384615384615,0.230769230769231,
0.246153846153846,0.261538461538462,0.276923076923077,0.292307692307692,
0.307692307692308,0.323076923076923,0.338461538461538,0.353846153846154,
0.369230769230769,0.384615384615385,0.4,0.415384615384615,0.430769230769231,
0.446153846153846,0.461538461538462,0.476923076923077,0.492307692307692,
0.507692307692308,0.523076923076923,0.538461538461538,0.553846153846154,
0.569230769230769,0.584615384615384,0.6,0.615384615384615,0.63076923076923,
0.646153846153846,0.661538461538461,0.676923076923076,0.692307692307692,
0.707692307692307,0.723076923076922,0.738461538461538,0.753846153846153,
0.769230769230768,0.784615384615384,0.799999999999999,0.815384615384614,
0.83076923076923,0.846153846153845,0.86153846153846,0.876923076923076,0.892307692307691,
0.907692307692306,0.923076923076922,0.938461538461537,0.953846153846152,
0.969230769230768,0.984615384615383,1.),.UNSPECIFIED.)
CURVE()
GEOMETRIC_REPRESENTATION_ITEM()
RATIONAL_B_SPLINE_CURVE((1.,1.,1.,1.,1.,1.,1.,1.,1.,1.,1.,1.,1.,1.,1.,1.,
1.,1.,1.,1.,1.,1.,1.,1.,1.,1.,1.,1.,1.,1.,1.,1.,1.,1.,1.,1.,1.,1.,1.,1.,
1.,1.,1.,1.,1.,1.,1.,1.,1.,1.,1.,1.,1.,1.,1.,1.,1.,1.,1.,1.,1.,1.,1.,1.,
1.,1.,1.,1.,1.,1.))
REPRESENTATION_ITEM('')
);
#272=(
BOUNDED_CURVE()
B_SPLINE_CURVE(5,(#34606,#34607,#34608,#34609,#34610,#34611,#34612,#34613,
#34614,#34615,#34616,#34617,#34618,#34619,#34620,#34621,#34622,#34623,#34624,
#34625,#34626,#34627,#34628,#34629,#34630,#34631,#34632,#34633,#34634,#34635,
#34636,#34637,#34638,#34639,#34640,#34641,#34642,#34643,#34644,#34645,#34646,
#34647,#34648,#34649,#34650,#34651,#34652,#34653,#34654,#34655,#34656,#34657,
#34658,#34659,#34660,#34661,#34662,#34663,#34664,#34665,#34666,#34667,#34668,
#34669,#34670,#34671,#34672,#34673,#34674,#34675),.UNSPECIFIED.,.F.,.F.)
B_SPLINE_CURVE_WITH_KNOTS((6,1,1,1,1,1,1,1,1,1,1,1,1,1,1,1,1,1,1,1,1,1,
1,1,1,1,1,1,1,1,1,1,1,1,1,1,1,1,1,1,1,1,1,1,1,1,1,1,1,1,1,1,1,1,1,1,1,1,
1,1,1,1,1,1,1,6),(0.,0.0153846153846154,0.0307692307692308,0.0461538461538462,
0.0615384615384615,0.0769230769230769,0.0923076923076923,0.107692307692308,
0.123076923076923,0.138461538461538,0.153846153846154,0.169230769230769,
0.184615384615385,0.2,0.215384615384615,0.230769230769231,0.246153846153846,
0.261538461538462,0.276923076923077,0.292307692307692,0.307692307692308,
0.323076923076923,0.338461538461538,0.353846153846154,0.369230769230769,
0.384615384615385,0.4,0.415384615384615,0.430769230769231,0.446153846153846,
0.461538461538462,0.476923076923077,0.492307692307692,0.507692307692308,
0.523076923076923,0.538461538461538,0.553846153846154,0.569230769230769,
0.584615384615384,0.6,0.615384615384615,0.63076923076923,0.646153846153846,
0.661538461538461,0.676923076923076,0.692307692307692,0.707692307692307,
0.723076923076922,0.738461538461538,0.753846153846153,0.769230769230768,
0.784615384615384,0.799999999999999,0.815384615384614,0.83076923076923,
0.846153846153845,0.86153846153846,0.876923076923076,0.892307692307691,
0.907692307692306,0.923076923076922,0.938461538461537,0.953846153846152,
0.969230769230768,0.984615384615383,0.994228156739723),.UNSPECIFIED.)
CURVE()
GEOMETRIC_REPRESENTATION_ITEM()
RATIONAL_B_SPLINE_CURVE((1.,1.,1.,1.,1.,1.,1.,1.,1.,1.,1.,1.,1.,1.,1.,1.,
1.,1.,1.,1.,1.,1.,1.,1.,1.,1.,1.,1.,1.,1.,1.,1.,1.,1.,1.,1.,1.,1.,1.,1.,
1.,1.,1.,1.,1.,1.,1.,1.,1.,1.,1.,1.,1.,1.,1.,1.,1.,1.,1.,1.,1.,1.,1.,1.,
1.,1.,1.,1.,1.,1.))
REPRESENTATION_ITEM('')
);
#273=(
BOUNDED_CURVE()
B_SPLINE_CURVE(5,(#34679,#34680,#34681,#34682,#34683,#34684,#34685,#34686,
#34687,#34688,#34689,#34690,#34691,#34692,#34693,#34694,#34695,#34696,#34697,
#34698,#34699,#34700,#34701,#34702,#34703,#34704,#34705,#34706,#34707,#34708,
#34709,#34710,#34711,#34712,#34713,#34714,#34715,#34716,#34717,#34718,#34719,
#34720,#34721,#34722,#34723,#34724,#34725,#34726,#34727,#34728,#34729,#34730,
#34731,#34732,#34733,#34734,#34735,#34736,#34737,#34738,#34739,#34740,#34741,
#34742,#34743,#34744,#34745,#34746,#34747,#34748),.UNSPECIFIED.,.F.,.F.)
B_SPLINE_CURVE_WITH_KNOTS((6,1,1,1,1,1,1,1,1,1,1,1,1,1,1,1,1,1,1,1,1,1,
1,1,1,1,1,1,1,1,1,1,1,1,1,1,1,1,1,1,1,1,1,1,1,1,1,1,1,1,1,1,1,1,1,1,1,1,
1,1,1,1,1,1,1,6),(0.00577184337450718,0.0153846153846154,0.0307692307692308,
0.0461538461538462,0.0615384615384615,0.0769230769230769,0.0923076923076923,
0.107692307692308,0.123076923076923,0.138461538461538,0.153846153846154,
0.169230769230769,0.184615384615385,0.2,0.215384615384615,0.230769230769231,
0.246153846153846,0.261538461538462,0.276923076923077,0.292307692307692,
0.307692307692308,0.323076923076923,0.338461538461538,0.353846153846154,
0.369230769230769,0.384615384615385,0.4,0.415384615384615,0.430769230769231,
0.446153846153846,0.461538461538462,0.476923076923077,0.492307692307692,
0.507692307692308,0.523076923076923,0.538461538461538,0.553846153846154,
0.569230769230769,0.584615384615384,0.6,0.615384615384615,0.63076923076923,
0.646153846153846,0.661538461538461,0.676923076923076,0.692307692307692,
0.707692307692307,0.723076923076922,0.738461538461538,0.753846153846153,
0.769230769230768,0.784615384615384,0.799999999999999,0.815384615384614,
0.83076923076923,0.846153846153845,0.86153846153846,0.876923076923076,0.892307692307691,
0.907692307692306,0.923076923076922,0.938461538461537,0.953846153846152,
0.969230769230768,0.984615384615383,1.),.UNSPECIFIED.)
CURVE()
GEOMETRIC_REPRESENTATION_ITEM()
RATIONAL_B_SPLINE_CURVE((1.,1.,1.,1.,1.,1.,1.,1.,1.,1.,1.,1.,1.,1.,1.,1.,
1.,1.,1.,1.,1.,1.,1.,1.,1.,1.,1.,1.,1.,1.,1.,1.,1.,1.,1.,1.,1.,1.,1.,1.,
1.,1.,1.,1.,1.,1.,1.,1.,1.,1.,1.,1.,1.,1.,1.,1.,1.,1.,1.,1.,1.,1.,1.,1.,
1.,1.,1.,1.,1.,1.))
REPRESENTATION_ITEM('')
);
#274=(
BOUNDED_CURVE()
B_SPLINE_CURVE(5,(#34752,#34753,#34754,#34755,#34756,#34757,#34758,#34759,
#34760,#34761,#34762,#34763,#34764,#34765,#34766,#34767,#34768,#34769,#34770,
#34771,#34772,#34773,#34774,#34775,#34776,#34777,#34778,#34779,#34780,#34781,
#34782,#34783,#34784,#34785,#34786,#34787,#34788,#34789,#34790,#34791,#34792,
#34793,#34794,#34795,#34796,#34797,#34798,#34799,#34800,#34801,#34802,#34803,
#34804,#34805,#34806,#34807,#34808,#34809,#34810,#34811,#34812,#34813,#34814,
#34815,#34816,#34817,#34818,#34819,#34820,#34821),.UNSPECIFIED.,.F.,.F.)
B_SPLINE_CURVE_WITH_KNOTS((6,1,1,1,1,1,1,1,1,1,1,1,1,1,1,1,1,1,1,1,1,1,
1,1,1,1,1,1,1,1,1,1,1,1,1,1,1,1,1,1,1,1,1,1,1,1,1,1,1,1,1,1,1,1,1,1,1,1,
1,1,1,1,1,1,1,6),(0.,0.0153846153846154,0.0307692307692308,0.0461538461538462,
0.0615384615384615,0.0769230769230769,0.0923076923076923,0.107692307692308,
0.123076923076923,0.138461538461538,0.153846153846154,0.169230769230769,
0.184615384615385,0.2,0.215384615384615,0.230769230769231,0.246153846153846,
0.261538461538462,0.276923076923077,0.292307692307692,0.307692307692308,
0.323076923076923,0.338461538461538,0.353846153846154,0.369230769230769,
0.384615384615385,0.4,0.415384615384615,0.430769230769231,0.446153846153846,
0.461538461538462,0.476923076923077,0.492307692307692,0.507692307692308,
0.523076923076923,0.538461538461538,0.553846153846154,0.569230769230769,
0.584615384615384,0.6,0.615384615384615,0.63076923076923,0.646153846153846,
0.661538461538461,0.676923076923076,0.692307692307692,0.707692307692307,
0.723076923076922,0.738461538461538,0.753846153846153,0.769230769230768,
0.784615384615384,0.799999999999999,0.815384615384614,0.83076923076923,
0.846153846153845,0.86153846153846,0.876923076923076,0.892307692307691,
0.907692307692306,0.923076923076922,0.938461538461537,0.953846153846152,
0.969230769230768,0.984615384615383,0.994228156739716),.UNSPECIFIED.)
CURVE()
GEOMETRIC_REPRESENTATION_ITEM()
RATIONAL_B_SPLINE_CURVE((1.,1.,1.,1.,1.,1.,1.,1.,1.,1.,1.,1.,1.,1.,1.,1.,
1.,1.,1.,1.,1.,1.,1.,1.,1.,1.,1.,1.,1.,1.,1.,1.,1.,1.,1.,1.,1.,1.,1.,1.,
1.,1.,1.,1.,1.,1.,1.,1.,1.,1.,1.,1.,1.,1.,1.,1.,1.,1.,1.,1.,1.,1.,1.,1.,
1.,1.,1.,1.,1.,1.))
REPRESENTATION_ITEM('')
);
#275=(
BOUNDED_CURVE()
B_SPLINE_CURVE(5,(#34825,#34826,#34827,#34828,#34829,#34830,#34831,#34832,
#34833,#34834,#34835,#34836,#34837,#34838,#34839,#34840,#34841,#34842,#34843,
#34844,#34845,#34846,#34847,#34848,#34849,#34850,#34851,#34852,#34853,#34854,
#34855,#34856,#34857,#34858,#34859,#34860,#34861,#34862,#34863,#34864,#34865,
#34866,#34867,#34868,#34869,#34870,#34871,#34872,#34873,#34874,#34875,#34876,
#34877,#34878,#34879,#34880,#34881,#34882,#34883,#34884,#34885,#34886,#34887,
#34888,#34889,#34890,#34891,#34892,#34893,#34894),.UNSPECIFIED.,.F.,.F.)
B_SPLINE_CURVE_WITH_KNOTS((6,1,1,1,1,1,1,1,1,1,1,1,1,1,1,1,1,1,1,1,1,1,
1,1,1,1,1,1,1,1,1,1,1,1,1,1,1,1,1,1,1,1,1,1,1,1,1,1,1,1,1,1,1,1,1,1,1,1,
1,1,1,1,1,1,1,6),(0.00577184337450174,0.0153846153846154,0.0307692307692308,
0.0461538461538462,0.0615384615384615,0.0769230769230769,0.0923076923076923,
0.107692307692308,0.123076923076923,0.138461538461538,0.153846153846154,
0.169230769230769,0.184615384615385,0.2,0.215384615384615,0.230769230769231,
0.246153846153846,0.261538461538462,0.276923076923077,0.292307692307692,
0.307692307692308,0.323076923076923,0.338461538461538,0.353846153846154,
0.369230769230769,0.384615384615385,0.4,0.415384615384615,0.430769230769231,
0.446153846153846,0.461538461538462,0.476923076923077,0.492307692307692,
0.507692307692308,0.523076923076923,0.538461538461538,0.553846153846154,
0.569230769230769,0.584615384615384,0.6,0.615384615384615,0.63076923076923,
0.646153846153846,0.661538461538461,0.676923076923076,0.692307692307692,
0.707692307692307,0.723076923076922,0.738461538461538,0.753846153846153,
0.769230769230768,0.784615384615384,0.799999999999999,0.815384615384614,
0.83076923076923,0.846153846153845,0.86153846153846,0.876923076923076,0.892307692307691,
0.907692307692306,0.923076923076922,0.938461538461537,0.953846153846152,
0.969230769230768,0.984615384615383,1.),.UNSPECIFIED.)
CURVE()
GEOMETRIC_REPRESENTATION_ITEM()
RATIONAL_B_SPLINE_CURVE((1.,1.,1.,1.,1.,1.,1.,1.,1.,1.,1.,1.,1.,1.,1.,1.,
1.,1.,1.,1.,1.,1.,1.,1.,1.,1.,1.,1.,1.,1.,1.,1.,1.,1.,1.,1.,1.,1.,1.,1.,
1.,1.,1.,1.,1.,1.,1.,1.,1.,1.,1.,1.,1.,1.,1.,1.,1.,1.,1.,1.,1.,1.,1.,1.,
1.,1.,1.,1.,1.,1.))
REPRESENTATION_ITEM('')
);
#276=(
BOUNDED_CURVE()
B_SPLINE_CURVE(5,(#34898,#34899,#34900,#34901,#34902,#34903,#34904,#34905,
#34906,#34907,#34908,#34909,#34910,#34911,#34912,#34913,#34914,#34915,#34916,
#34917,#34918,#34919,#34920,#34921,#34922,#34923,#34924,#34925,#34926,#34927,
#34928,#34929,#34930,#34931,#34932,#34933,#34934,#34935,#34936,#34937,#34938,
#34939,#34940,#34941,#34942,#34943,#34944,#34945,#34946,#34947,#34948,#34949,
#34950,#34951,#34952,#34953,#34954,#34955,#34956,#34957,#34958,#34959,#34960,
#34961,#34962,#34963,#34964,#34965,#34966,#34967),.UNSPECIFIED.,.F.,.F.)
B_SPLINE_CURVE_WITH_KNOTS((6,1,1,1,1,1,1,1,1,1,1,1,1,1,1,1,1,1,1,1,1,1,
1,1,1,1,1,1,1,1,1,1,1,1,1,1,1,1,1,1,1,1,1,1,1,1,1,1,1,1,1,1,1,1,1,1,1,1,
1,1,1,1,1,1,1,6),(0.,0.0153846153846154,0.0307692307692308,0.0461538461538462,
0.0615384615384615,0.0769230769230769,0.0923076923076923,0.107692307692308,
0.123076923076923,0.138461538461538,0.153846153846154,0.169230769230769,
0.184615384615385,0.2,0.215384615384615,0.230769230769231,0.246153846153846,
0.261538461538462,0.276923076923077,0.292307692307692,0.307692307692308,
0.323076923076923,0.338461538461538,0.353846153846154,0.369230769230769,
0.384615384615385,0.4,0.415384615384615,0.430769230769231,0.446153846153846,
0.461538461538462,0.476923076923077,0.492307692307692,0.507692307692308,
0.523076923076923,0.538461538461538,0.553846153846154,0.569230769230769,
0.584615384615384,0.6,0.615384615384615,0.63076923076923,0.646153846153846,
0.661538461538461,0.676923076923076,0.692307692307692,0.707692307692307,
0.723076923076922,0.738461538461538,0.753846153846153,0.769230769230768,
0.784615384615384,0.799999999999999,0.815384615384614,0.83076923076923,
0.846153846153845,0.86153846153846,0.876923076923076,0.892307692307691,
0.907692307692306,0.923076923076922,0.938461538461537,0.953846153846152,
0.969230769230768,0.984615384615383,0.994228156739722),.UNSPECIFIED.)
CURVE()
GEOMETRIC_REPRESENTATION_ITEM()
RATIONAL_B_SPLINE_CURVE((1.,1.,1.,1.,1.,1.,1.,1.,1.,1.,1.,1.,1.,1.,1.,1.,
1.,1.,1.,1.,1.,1.,1.,1.,1.,1.,1.,1.,1.,1.,1.,1.,1.,1.,1.,1.,1.,1.,1.,1.,
1.,1.,1.,1.,1.,1.,1.,1.,1.,1.,1.,1.,1.,1.,1.,1.,1.,1.,1.,1.,1.,1.,1.,1.,
1.,1.,1.,1.,1.,1.))
REPRESENTATION_ITEM('')
);
#277=(
BOUNDED_CURVE()
B_SPLINE_CURVE(5,(#34971,#34972,#34973,#34974,#34975,#34976,#34977,#34978,
#34979,#34980,#34981,#34982,#34983,#34984,#34985,#34986,#34987,#34988,#34989,
#34990,#34991,#34992,#34993,#34994,#34995,#34996,#34997,#34998,#34999,#35000,
#35001,#35002,#35003,#35004,#35005,#35006,#35007,#35008,#35009,#35010,#35011,
#35012,#35013,#35014,#35015,#35016,#35017,#35018,#35019,#35020,#35021,#35022,
#35023,#35024,#35025,#35026,#35027,#35028,#35029,#35030,#35031,#35032,#35033,
#35034,#35035,#35036,#35037,#35038,#35039,#35040),.UNSPECIFIED.,.F.,.F.)
B_SPLINE_CURVE_WITH_KNOTS((6,1,1,1,1,1,1,1,1,1,1,1,1,1,1,1,1,1,1,1,1,1,
1,1,1,1,1,1,1,1,1,1,1,1,1,1,1,1,1,1,1,1,1,1,1,1,1,1,1,1,1,1,1,1,1,1,1,1,
1,1,1,1,1,1,1,6),(0.00577184337450943,0.0153846153846154,0.0307692307692308,
0.0461538461538462,0.0615384615384615,0.0769230769230769,0.0923076923076923,
0.107692307692308,0.123076923076923,0.138461538461538,0.153846153846154,
0.169230769230769,0.184615384615385,0.2,0.215384615384615,0.230769230769231,
0.246153846153846,0.261538461538462,0.276923076923077,0.292307692307692,
0.307692307692308,0.323076923076923,0.338461538461538,0.353846153846154,
0.369230769230769,0.384615384615385,0.4,0.415384615384615,0.430769230769231,
0.446153846153846,0.461538461538462,0.476923076923077,0.492307692307692,
0.507692307692308,0.523076923076923,0.538461538461538,0.553846153846154,
0.569230769230769,0.584615384615384,0.6,0.615384615384615,0.63076923076923,
0.646153846153846,0.661538461538461,0.676923076923076,0.692307692307692,
0.707692307692307,0.723076923076922,0.738461538461538,0.753846153846153,
0.769230769230768,0.784615384615384,0.799999999999999,0.815384615384614,
0.83076923076923,0.846153846153845,0.86153846153846,0.876923076923076,0.892307692307691,
0.907692307692306,0.923076923076922,0.938461538461537,0.953846153846152,
0.969230769230768,0.984615384615383,1.),.UNSPECIFIED.)
CURVE()
GEOMETRIC_REPRESENTATION_ITEM()
RATIONAL_B_SPLINE_CURVE((1.,1.,1.,1.,1.,1.,1.,1.,1.,1.,1.,1.,1.,1.,1.,1.,
1.,1.,1.,1.,1.,1.,1.,1.,1.,1.,1.,1.,1.,1.,1.,1.,1.,1.,1.,1.,1.,1.,1.,1.,
1.,1.,1.,1.,1.,1.,1.,1.,1.,1.,1.,1.,1.,1.,1.,1.,1.,1.,1.,1.,1.,1.,1.,1.,
1.,1.,1.,1.,1.,1.))
REPRESENTATION_ITEM('')
);
#278=(
BOUNDED_CURVE()
B_SPLINE_CURVE(5,(#35044,#35045,#35046,#35047,#35048,#35049,#35050,#35051,
#35052,#35053,#35054,#35055,#35056,#35057,#35058,#35059,#35060,#35061,#35062,
#35063,#35064,#35065,#35066,#35067,#35068,#35069,#35070,#35071,#35072,#35073,
#35074,#35075,#35076,#35077,#35078,#35079,#35080,#35081,#35082,#35083,#35084,
#35085,#35086,#35087,#35088,#35089,#35090,#35091,#35092,#35093,#35094,#35095,
#35096,#35097,#35098,#35099,#35100,#35101,#35102,#35103,#35104,#35105,#35106,
#35107,#35108,#35109,#35110,#35111,#35112,#35113),.UNSPECIFIED.,.F.,.F.)
B_SPLINE_CURVE_WITH_KNOTS((6,1,1,1,1,1,1,1,1,1,1,1,1,1,1,1,1,1,1,1,1,1,
1,1,1,1,1,1,1,1,1,1,1,1,1,1,1,1,1,1,1,1,1,1,1,1,1,1,1,1,1,1,1,1,1,1,1,1,
1,1,1,1,1,1,1,6),(0.,0.0153846153846154,0.0307692307692308,0.0461538461538462,
0.0615384615384615,0.0769230769230769,0.0923076923076923,0.107692307692308,
0.123076923076923,0.138461538461538,0.153846153846154,0.169230769230769,
0.184615384615385,0.2,0.215384615384615,0.230769230769231,0.246153846153846,
0.261538461538462,0.276923076923077,0.292307692307692,0.307692307692308,
0.323076923076923,0.338461538461538,0.353846153846154,0.369230769230769,
0.384615384615385,0.4,0.415384615384615,0.430769230769231,0.446153846153846,
0.461538461538462,0.476923076923077,0.492307692307692,0.507692307692308,
0.523076923076923,0.538461538461538,0.553846153846154,0.569230769230769,
0.584615384615384,0.6,0.615384615384615,0.63076923076923,0.646153846153846,
0.661538461538461,0.676923076923076,0.692307692307692,0.707692307692307,
0.723076923076922,0.738461538461538,0.753846153846153,0.769230769230768,
0.784615384615384,0.799999999999999,0.815384615384614,0.83076923076923,
0.846153846153845,0.86153846153846,0.876923076923076,0.892307692307691,
0.907692307692306,0.923076923076922,0.938461538461537,0.953846153846152,
0.969230769230768,0.984615384615383,0.994228156739699),.UNSPECIFIED.)
CURVE()
GEOMETRIC_REPRESENTATION_ITEM()
RATIONAL_B_SPLINE_CURVE((1.,1.,1.,1.,1.,1.,1.,1.,1.,1.,1.,1.,1.,1.,1.,1.,
1.,1.,1.,1.,1.,1.,1.,1.,1.,1.,1.,1.,1.,1.,1.,1.,1.,1.,1.,1.,1.,1.,1.,1.,
1.,1.,1.,1.,1.,1.,1.,1.,1.,1.,1.,1.,1.,1.,1.,1.,1.,1.,1.,1.,1.,1.,1.,1.,
1.,1.,1.,1.,1.,1.))
REPRESENTATION_ITEM('')
);
#279=(
BOUNDED_CURVE()
B_SPLINE_CURVE(5,(#35117,#35118,#35119,#35120,#35121,#35122,#35123,#35124,
#35125,#35126,#35127,#35128,#35129,#35130,#35131,#35132,#35133,#35134,#35135,
#35136,#35137,#35138,#35139,#35140,#35141,#35142,#35143,#35144,#35145,#35146,
#35147,#35148,#35149,#35150,#35151,#35152,#35153,#35154,#35155,#35156,#35157,
#35158,#35159,#35160,#35161,#35162,#35163,#35164,#35165,#35166,#35167,#35168,
#35169,#35170,#35171,#35172,#35173,#35174,#35175,#35176,#35177,#35178,#35179,
#35180,#35181,#35182,#35183,#35184,#35185,#35186),.UNSPECIFIED.,.F.,.F.)
B_SPLINE_CURVE_WITH_KNOTS((6,1,1,1,1,1,1,1,1,1,1,1,1,1,1,1,1,1,1,1,1,1,
1,1,1,1,1,1,1,1,1,1,1,1,1,1,1,1,1,1,1,1,1,1,1,1,1,1,1,1,1,1,1,1,1,1,1,1,
1,1,1,1,1,1,1,6),(0.00577184337450665,0.0153846153846154,0.0307692307692308,
0.0461538461538462,0.0615384615384615,0.0769230769230769,0.0923076923076923,
0.107692307692308,0.123076923076923,0.138461538461538,0.153846153846154,
0.169230769230769,0.184615384615385,0.2,0.215384615384615,0.230769230769231,
0.246153846153846,0.261538461538462,0.276923076923077,0.292307692307692,
0.307692307692308,0.323076923076923,0.338461538461538,0.353846153846154,
0.369230769230769,0.384615384615385,0.4,0.415384615384615,0.430769230769231,
0.446153846153846,0.461538461538462,0.476923076923077,0.492307692307692,
0.507692307692308,0.523076923076923,0.538461538461538,0.553846153846154,
0.569230769230769,0.584615384615384,0.6,0.615384615384615,0.63076923076923,
0.646153846153846,0.661538461538461,0.676923076923076,0.692307692307692,
0.707692307692307,0.723076923076922,0.738461538461538,0.753846153846153,
0.769230769230768,0.784615384615384,0.799999999999999,0.815384615384614,
0.83076923076923,0.846153846153845,0.86153846153846,0.876923076923076,0.892307692307691,
0.907692307692306,0.923076923076922,0.938461538461537,0.953846153846152,
0.969230769230768,0.984615384615383,1.),.UNSPECIFIED.)
CURVE()
GEOMETRIC_REPRESENTATION_ITEM()
RATIONAL_B_SPLINE_CURVE((1.,1.,1.,1.,1.,1.,1.,1.,1.,1.,1.,1.,1.,1.,1.,1.,
1.,1.,1.,1.,1.,1.,1.,1.,1.,1.,1.,1.,1.,1.,1.,1.,1.,1.,1.,1.,1.,1.,1.,1.,
1.,1.,1.,1.,1.,1.,1.,1.,1.,1.,1.,1.,1.,1.,1.,1.,1.,1.,1.,1.,1.,1.,1.,1.,
1.,1.,1.,1.,1.,1.))
REPRESENTATION_ITEM('')
);
#280=(
BOUNDED_CURVE()
B_SPLINE_CURVE(5,(#35190,#35191,#35192,#35193,#35194,#35195,#35196,#35197,
#35198,#35199,#35200,#35201,#35202,#35203,#35204,#35205,#35206,#35207,#35208,
#35209,#35210,#35211,#35212,#35213,#35214,#35215,#35216,#35217,#35218,#35219,
#35220,#35221,#35222,#35223,#35224,#35225,#35226,#35227,#35228,#35229,#35230,
#35231,#35232,#35233,#35234,#35235,#35236,#35237,#35238,#35239,#35240,#35241,
#35242,#35243,#35244,#35245,#35246,#35247,#35248,#35249,#35250,#35251,#35252,
#35253,#35254,#35255,#35256,#35257,#35258,#35259),.UNSPECIFIED.,.F.,.F.)
B_SPLINE_CURVE_WITH_KNOTS((6,1,1,1,1,1,1,1,1,1,1,1,1,1,1,1,1,1,1,1,1,1,
1,1,1,1,1,1,1,1,1,1,1,1,1,1,1,1,1,1,1,1,1,1,1,1,1,1,1,1,1,1,1,1,1,1,1,1,
1,1,1,1,1,1,1,6),(0.,0.0153846153846154,0.0307692307692308,0.0461538461538462,
0.0615384615384615,0.0769230769230769,0.0923076923076923,0.107692307692308,
0.123076923076923,0.138461538461538,0.153846153846154,0.169230769230769,
0.184615384615385,0.2,0.215384615384615,0.230769230769231,0.246153846153846,
0.261538461538462,0.276923076923077,0.292307692307692,0.307692307692308,
0.323076923076923,0.338461538461538,0.353846153846154,0.369230769230769,
0.384615384615385,0.4,0.415384615384615,0.430769230769231,0.446153846153846,
0.461538461538462,0.476923076923077,0.492307692307692,0.507692307692308,
0.523076923076923,0.538461538461538,0.553846153846154,0.569230769230769,
0.584615384615384,0.6,0.615384615384615,0.63076923076923,0.646153846153846,
0.661538461538461,0.676923076923076,0.692307692307692,0.707692307692307,
0.723076923076922,0.738461538461538,0.753846153846153,0.769230769230768,
0.784615384615384,0.799999999999999,0.815384615384614,0.83076923076923,
0.846153846153845,0.86153846153846,0.876923076923076,0.892307692307691,
0.907692307692306,0.923076923076922,0.938461538461537,0.953846153846152,
0.969230769230768,0.984615384615383,0.994228156739691),.UNSPECIFIED.)
CURVE()
GEOMETRIC_REPRESENTATION_ITEM()
RATIONAL_B_SPLINE_CURVE((1.,1.,1.,1.,1.,1.,1.,1.,1.,1.,1.,1.,1.,1.,1.,1.,
1.,1.,1.,1.,1.,1.,1.,1.,1.,1.,1.,1.,1.,1.,1.,1.,1.,1.,1.,1.,1.,1.,1.,1.,
1.,1.,1.,1.,1.,1.,1.,1.,1.,1.,1.,1.,1.,1.,1.,1.,1.,1.,1.,1.,1.,1.,1.,1.,
1.,1.,1.,1.,1.,1.))
REPRESENTATION_ITEM('')
);
#281=(
BOUNDED_CURVE()
B_SPLINE_CURVE(5,(#35263,#35264,#35265,#35266,#35267,#35268,#35269,#35270,
#35271,#35272,#35273,#35274,#35275,#35276,#35277,#35278,#35279,#35280,#35281,
#35282,#35283,#35284,#35285,#35286,#35287,#35288,#35289,#35290,#35291,#35292,
#35293,#35294,#35295,#35296,#35297,#35298,#35299,#35300,#35301,#35302,#35303,
#35304,#35305,#35306,#35307,#35308,#35309,#35310,#35311,#35312,#35313,#35314,
#35315,#35316,#35317,#35318,#35319,#35320,#35321,#35322,#35323,#35324,#35325,
#35326,#35327,#35328,#35329,#35330,#35331,#35332),.UNSPECIFIED.,.F.,.F.)
B_SPLINE_CURVE_WITH_KNOTS((6,1,1,1,1,1,1,1,1,1,1,1,1,1,1,1,1,1,1,1,1,1,
1,1,1,1,1,1,1,1,1,1,1,1,1,1,1,1,1,1,1,1,1,1,1,1,1,1,1,1,1,1,1,1,1,1,1,1,
1,1,1,1,1,1,1,6),(0.00577184337450785,0.0153846153846154,0.0307692307692308,
0.0461538461538462,0.0615384615384615,0.0769230769230769,0.0923076923076923,
0.107692307692308,0.123076923076923,0.138461538461538,0.153846153846154,
0.169230769230769,0.184615384615385,0.2,0.215384615384615,0.230769230769231,
0.246153846153846,0.261538461538462,0.276923076923077,0.292307692307692,
0.307692307692308,0.323076923076923,0.338461538461538,0.353846153846154,
0.369230769230769,0.384615384615385,0.4,0.415384615384615,0.430769230769231,
0.446153846153846,0.461538461538462,0.476923076923077,0.492307692307692,
0.507692307692308,0.523076923076923,0.538461538461538,0.553846153846154,
0.569230769230769,0.584615384615384,0.6,0.615384615384615,0.63076923076923,
0.646153846153846,0.661538461538461,0.676923076923076,0.692307692307692,
0.707692307692307,0.723076923076922,0.738461538461538,0.753846153846153,
0.769230769230768,0.784615384615384,0.799999999999999,0.815384615384614,
0.83076923076923,0.846153846153845,0.86153846153846,0.876923076923076,0.892307692307691,
0.907692307692306,0.923076923076922,0.938461538461537,0.953846153846152,
0.969230769230768,0.984615384615383,1.),.UNSPECIFIED.)
CURVE()
GEOMETRIC_REPRESENTATION_ITEM()
RATIONAL_B_SPLINE_CURVE((1.,1.,1.,1.,1.,1.,1.,1.,1.,1.,1.,1.,1.,1.,1.,1.,
1.,1.,1.,1.,1.,1.,1.,1.,1.,1.,1.,1.,1.,1.,1.,1.,1.,1.,1.,1.,1.,1.,1.,1.,
1.,1.,1.,1.,1.,1.,1.,1.,1.,1.,1.,1.,1.,1.,1.,1.,1.,1.,1.,1.,1.,1.,1.,1.,
1.,1.,1.,1.,1.,1.))
REPRESENTATION_ITEM('')
);
#282=(
BOUNDED_CURVE()
B_SPLINE_CURVE(5,(#35336,#35337,#35338,#35339,#35340,#35341,#35342,#35343,
#35344,#35345,#35346,#35347,#35348,#35349,#35350,#35351,#35352,#35353,#35354,
#35355,#35356,#35357,#35358,#35359,#35360,#35361,#35362,#35363,#35364,#35365,
#35366,#35367,#35368,#35369,#35370,#35371,#35372,#35373,#35374,#35375,#35376,
#35377,#35378,#35379,#35380,#35381,#35382,#35383,#35384,#35385,#35386,#35387,
#35388,#35389,#35390,#35391,#35392,#35393,#35394,#35395,#35396,#35397,#35398,
#35399,#35400,#35401,#35402,#35403,#35404,#35405),.UNSPECIFIED.,.F.,.F.)
B_SPLINE_CURVE_WITH_KNOTS((6,1,1,1,1,1,1,1,1,1,1,1,1,1,1,1,1,1,1,1,1,1,
1,1,1,1,1,1,1,1,1,1,1,1,1,1,1,1,1,1,1,1,1,1,1,1,1,1,1,1,1,1,1,1,1,1,1,1,
1,1,1,1,1,1,1,6),(0.,0.0153846153846154,0.0307692307692308,0.0461538461538462,
0.0615384615384615,0.0769230769230769,0.0923076923076923,0.107692307692308,
0.123076923076923,0.138461538461538,0.153846153846154,0.169230769230769,
0.184615384615385,0.2,0.215384615384615,0.230769230769231,0.246153846153846,
0.261538461538462,0.276923076923077,0.292307692307692,0.307692307692308,
0.323076923076923,0.338461538461538,0.353846153846154,0.369230769230769,
0.384615384615385,0.4,0.415384615384615,0.430769230769231,0.446153846153846,
0.461538461538462,0.476923076923077,0.492307692307692,0.507692307692308,
0.523076923076923,0.538461538461538,0.553846153846154,0.569230769230769,
0.584615384615384,0.6,0.615384615384615,0.63076923076923,0.646153846153846,
0.661538461538461,0.676923076923076,0.692307692307692,0.707692307692307,
0.723076923076922,0.738461538461538,0.753846153846153,0.769230769230768,
0.784615384615384,0.799999999999999,0.815384615384614,0.83076923076923,
0.846153846153845,0.86153846153846,0.876923076923076,0.892307692307691,
0.907692307692306,0.923076923076922,0.938461538461537,0.953846153846152,
0.969230769230768,0.984615384615383,0.994228156739708),.UNSPECIFIED.)
CURVE()
GEOMETRIC_REPRESENTATION_ITEM()
RATIONAL_B_SPLINE_CURVE((1.,1.,1.,1.,1.,1.,1.,1.,1.,1.,1.,1.,1.,1.,1.,1.,
1.,1.,1.,1.,1.,1.,1.,1.,1.,1.,1.,1.,1.,1.,1.,1.,1.,1.,1.,1.,1.,1.,1.,1.,
1.,1.,1.,1.,1.,1.,1.,1.,1.,1.,1.,1.,1.,1.,1.,1.,1.,1.,1.,1.,1.,1.,1.,1.,
1.,1.,1.,1.,1.,1.))
REPRESENTATION_ITEM('')
);
#283=(
BOUNDED_CURVE()
B_SPLINE_CURVE(5,(#35409,#35410,#35411,#35412,#35413,#35414,#35415,#35416,
#35417,#35418,#35419,#35420,#35421,#35422,#35423,#35424,#35425,#35426,#35427,
#35428,#35429,#35430,#35431,#35432,#35433,#35434,#35435,#35436,#35437,#35438,
#35439,#35440,#35441,#35442,#35443,#35444,#35445,#35446,#35447,#35448,#35449,
#35450,#35451,#35452,#35453,#35454,#35455,#35456,#35457,#35458,#35459,#35460,
#35461,#35462,#35463,#35464,#35465,#35466,#35467,#35468,#35469,#35470,#35471,
#35472,#35473,#35474,#35475,#35476,#35477,#35478),.UNSPECIFIED.,.F.,.F.)
B_SPLINE_CURVE_WITH_KNOTS((6,1,1,1,1,1,1,1,1,1,1,1,1,1,1,1,1,1,1,1,1,1,
1,1,1,1,1,1,1,1,1,1,1,1,1,1,1,1,1,1,1,1,1,1,1,1,1,1,1,1,1,1,1,1,1,1,1,1,
1,1,1,1,1,1,1,6),(0.00577184337450072,0.0153846153846154,0.0307692307692308,
0.0461538461538462,0.0615384615384615,0.0769230769230769,0.0923076923076923,
0.107692307692308,0.123076923076923,0.138461538461538,0.153846153846154,
0.169230769230769,0.184615384615385,0.2,0.215384615384615,0.230769230769231,
0.246153846153846,0.261538461538462,0.276923076923077,0.292307692307692,
0.307692307692308,0.323076923076923,0.338461538461538,0.353846153846154,
0.369230769230769,0.384615384615385,0.4,0.415384615384615,0.430769230769231,
0.446153846153846,0.461538461538462,0.476923076923077,0.492307692307692,
0.507692307692308,0.523076923076923,0.538461538461538,0.553846153846154,
0.569230769230769,0.584615384615384,0.6,0.615384615384615,0.63076923076923,
0.646153846153846,0.661538461538461,0.676923076923076,0.692307692307692,
0.707692307692307,0.723076923076922,0.738461538461538,0.753846153846153,
0.769230769230768,0.784615384615384,0.799999999999999,0.815384615384614,
0.83076923076923,0.846153846153845,0.86153846153846,0.876923076923076,0.892307692307691,
0.907692307692306,0.923076923076922,0.938461538461537,0.953846153846152,
0.969230769230768,0.984615384615383,1.),.UNSPECIFIED.)
CURVE()
GEOMETRIC_REPRESENTATION_ITEM()
RATIONAL_B_SPLINE_CURVE((1.,1.,1.,1.,1.,1.,1.,1.,1.,1.,1.,1.,1.,1.,1.,1.,
1.,1.,1.,1.,1.,1.,1.,1.,1.,1.,1.,1.,1.,1.,1.,1.,1.,1.,1.,1.,1.,1.,1.,1.,
1.,1.,1.,1.,1.,1.,1.,1.,1.,1.,1.,1.,1.,1.,1.,1.,1.,1.,1.,1.,1.,1.,1.,1.,
1.,1.,1.,1.,1.,1.))
REPRESENTATION_ITEM('')
);
#284=(
BOUNDED_CURVE()
B_SPLINE_CURVE(5,(#35482,#35483,#35484,#35485,#35486,#35487,#35488,#35489,
#35490,#35491,#35492,#35493,#35494,#35495,#35496,#35497,#35498,#35499,#35500,
#35501,#35502,#35503,#35504,#35505,#35506,#35507,#35508,#35509,#35510,#35511,
#35512,#35513,#35514,#35515,#35516,#35517,#35518,#35519,#35520,#35521,#35522,
#35523,#35524,#35525,#35526,#35527,#35528,#35529,#35530,#35531,#35532,#35533,
#35534,#35535,#35536,#35537,#35538,#35539,#35540,#35541,#35542,#35543,#35544,
#35545,#35546,#35547,#35548,#35549,#35550,#35551),.UNSPECIFIED.,.F.,.F.)
B_SPLINE_CURVE_WITH_KNOTS((6,1,1,1,1,1,1,1,1,1,1,1,1,1,1,1,1,1,1,1,1,1,
1,1,1,1,1,1,1,1,1,1,1,1,1,1,1,1,1,1,1,1,1,1,1,1,1,1,1,1,1,1,1,1,1,1,1,1,
1,1,1,1,1,1,1,6),(0.,0.0153846153846154,0.0307692307692308,0.0461538461538462,
0.0615384615384615,0.0769230769230769,0.0923076923076923,0.107692307692308,
0.123076923076923,0.138461538461538,0.153846153846154,0.169230769230769,
0.184615384615385,0.2,0.215384615384615,0.230769230769231,0.246153846153846,
0.261538461538462,0.276923076923077,0.292307692307692,0.307692307692308,
0.323076923076923,0.338461538461538,0.353846153846154,0.369230769230769,
0.384615384615385,0.4,0.415384615384615,0.430769230769231,0.446153846153846,
0.461538461538462,0.476923076923077,0.492307692307692,0.507692307692308,
0.523076923076923,0.538461538461538,0.553846153846154,0.569230769230769,
0.584615384615384,0.6,0.615384615384615,0.63076923076923,0.646153846153846,
0.661538461538461,0.676923076923076,0.692307692307692,0.707692307692307,
0.723076923076922,0.738461538461538,0.753846153846153,0.769230769230768,
0.784615384615384,0.799999999999999,0.815384615384614,0.83076923076923,
0.846153846153845,0.86153846153846,0.876923076923076,0.892307692307691,
0.907692307692306,0.923076923076922,0.938461538461537,0.953846153846152,
0.969230769230768,0.984615384615383,0.994228156739706),.UNSPECIFIED.)
CURVE()
GEOMETRIC_REPRESENTATION_ITEM()
RATIONAL_B_SPLINE_CURVE((1.,1.,1.,1.,1.,1.,1.,1.,1.,1.,1.,1.,1.,1.,1.,1.,
1.,1.,1.,1.,1.,1.,1.,1.,1.,1.,1.,1.,1.,1.,1.,1.,1.,1.,1.,1.,1.,1.,1.,1.,
1.,1.,1.,1.,1.,1.,1.,1.,1.,1.,1.,1.,1.,1.,1.,1.,1.,1.,1.,1.,1.,1.,1.,1.,
1.,1.,1.,1.,1.,1.))
REPRESENTATION_ITEM('')
);
#285=(
BOUNDED_CURVE()
B_SPLINE_CURVE(5,(#35555,#35556,#35557,#35558,#35559,#35560,#35561,#35562,
#35563,#35564,#35565,#35566,#35567,#35568,#35569,#35570,#35571,#35572,#35573,
#35574,#35575,#35576,#35577,#35578,#35579,#35580,#35581,#35582,#35583,#35584,
#35585,#35586,#35587,#35588,#35589,#35590,#35591,#35592,#35593,#35594,#35595,
#35596,#35597,#35598,#35599,#35600,#35601,#35602,#35603,#35604,#35605,#35606,
#35607,#35608,#35609,#35610,#35611,#35612,#35613,#35614,#35615,#35616,#35617,
#35618,#35619,#35620,#35621,#35622,#35623,#35624),.UNSPECIFIED.,.F.,.F.)
B_SPLINE_CURVE_WITH_KNOTS((6,1,1,1,1,1,1,1,1,1,1,1,1,1,1,1,1,1,1,1,1,1,
1,1,1,1,1,1,1,1,1,1,1,1,1,1,1,1,1,1,1,1,1,1,1,1,1,1,1,1,1,1,1,1,1,1,1,1,
1,1,1,1,1,1,1,6),(0.00577184337450902,0.0153846153846154,0.0307692307692308,
0.0461538461538462,0.0615384615384615,0.0769230769230769,0.0923076923076923,
0.107692307692308,0.123076923076923,0.138461538461538,0.153846153846154,
0.169230769230769,0.184615384615385,0.2,0.215384615384615,0.230769230769231,
0.246153846153846,0.261538461538462,0.276923076923077,0.292307692307692,
0.307692307692308,0.323076923076923,0.338461538461538,0.353846153846154,
0.369230769230769,0.384615384615385,0.4,0.415384615384615,0.430769230769231,
0.446153846153846,0.461538461538462,0.476923076923077,0.492307692307692,
0.507692307692308,0.523076923076923,0.538461538461538,0.553846153846154,
0.569230769230769,0.584615384615384,0.6,0.615384615384615,0.63076923076923,
0.646153846153846,0.661538461538461,0.676923076923076,0.692307692307692,
0.707692307692307,0.723076923076922,0.738461538461538,0.753846153846153,
0.769230769230768,0.784615384615384,0.799999999999999,0.815384615384614,
0.83076923076923,0.846153846153845,0.86153846153846,0.876923076923076,0.892307692307691,
0.907692307692306,0.923076923076922,0.938461538461537,0.953846153846152,
0.969230769230768,0.984615384615383,1.),.UNSPECIFIED.)
CURVE()
GEOMETRIC_REPRESENTATION_ITEM()
RATIONAL_B_SPLINE_CURVE((1.,1.,1.,1.,1.,1.,1.,1.,1.,1.,1.,1.,1.,1.,1.,1.,
1.,1.,1.,1.,1.,1.,1.,1.,1.,1.,1.,1.,1.,1.,1.,1.,1.,1.,1.,1.,1.,1.,1.,1.,
1.,1.,1.,1.,1.,1.,1.,1.,1.,1.,1.,1.,1.,1.,1.,1.,1.,1.,1.,1.,1.,1.,1.,1.,
1.,1.,1.,1.,1.,1.))
REPRESENTATION_ITEM('')
);
#286=(
BOUNDED_CURVE()
B_SPLINE_CURVE(5,(#35628,#35629,#35630,#35631,#35632,#35633,#35634,#35635,
#35636,#35637,#35638,#35639,#35640,#35641,#35642,#35643,#35644,#35645,#35646,
#35647,#35648,#35649,#35650,#35651,#35652,#35653,#35654,#35655,#35656,#35657,
#35658,#35659,#35660,#35661,#35662,#35663,#35664,#35665,#35666,#35667,#35668,
#35669,#35670,#35671,#35672,#35673,#35674,#35675,#35676,#35677,#35678,#35679,
#35680,#35681,#35682,#35683,#35684,#35685,#35686,#35687,#35688,#35689,#35690,
#35691,#35692,#35693,#35694,#35695,#35696,#35697),.UNSPECIFIED.,.F.,.F.)
B_SPLINE_CURVE_WITH_KNOTS((6,1,1,1,1,1,1,1,1,1,1,1,1,1,1,1,1,1,1,1,1,1,
1,1,1,1,1,1,1,1,1,1,1,1,1,1,1,1,1,1,1,1,1,1,1,1,1,1,1,1,1,1,1,1,1,1,1,1,
1,1,1,1,1,1,1,6),(0.,0.0153846153846154,0.0307692307692308,0.0461538461538462,
0.0615384615384615,0.0769230769230769,0.0923076923076923,0.107692307692308,
0.123076923076923,0.138461538461538,0.153846153846154,0.169230769230769,
0.184615384615385,0.2,0.215384615384615,0.230769230769231,0.246153846153846,
0.261538461538462,0.276923076923077,0.292307692307692,0.307692307692308,
0.323076923076923,0.338461538461538,0.353846153846154,0.369230769230769,
0.384615384615385,0.4,0.415384615384615,0.430769230769231,0.446153846153846,
0.461538461538462,0.476923076923077,0.492307692307692,0.507692307692308,
0.523076923076923,0.538461538461538,0.553846153846154,0.569230769230769,
0.584615384615384,0.6,0.615384615384615,0.63076923076923,0.646153846153846,
0.661538461538461,0.676923076923076,0.692307692307692,0.707692307692307,
0.723076923076922,0.738461538461538,0.753846153846153,0.769230769230768,
0.784615384615384,0.799999999999999,0.815384615384614,0.83076923076923,
0.846153846153845,0.86153846153846,0.876923076923076,0.892307692307691,
0.907692307692306,0.923076923076922,0.938461538461537,0.953846153846152,
0.969230769230768,0.984615384615383,0.994228156739698),.UNSPECIFIED.)
CURVE()
GEOMETRIC_REPRESENTATION_ITEM()
RATIONAL_B_SPLINE_CURVE((1.,1.,1.,1.,1.,1.,1.,1.,1.,1.,1.,1.,1.,1.,1.,1.,
1.,1.,1.,1.,1.,1.,1.,1.,1.,1.,1.,1.,1.,1.,1.,1.,1.,1.,1.,1.,1.,1.,1.,1.,
1.,1.,1.,1.,1.,1.,1.,1.,1.,1.,1.,1.,1.,1.,1.,1.,1.,1.,1.,1.,1.,1.,1.,1.,
1.,1.,1.,1.,1.,1.))
REPRESENTATION_ITEM('')
);
#287=(
BOUNDED_CURVE()
B_SPLINE_CURVE(5,(#35701,#35702,#35703,#35704,#35705,#35706,#35707,#35708,
#35709,#35710,#35711,#35712,#35713,#35714,#35715,#35716,#35717,#35718,#35719,
#35720,#35721,#35722,#35723,#35724,#35725,#35726,#35727,#35728,#35729,#35730,
#35731,#35732,#35733,#35734,#35735,#35736,#35737,#35738,#35739,#35740,#35741,
#35742,#35743,#35744,#35745,#35746,#35747,#35748,#35749,#35750,#35751,#35752,
#35753,#35754,#35755,#35756,#35757,#35758,#35759,#35760,#35761,#35762,#35763,
#35764,#35765,#35766,#35767,#35768,#35769,#35770),.UNSPECIFIED.,.F.,.F.)
B_SPLINE_CURVE_WITH_KNOTS((6,1,1,1,1,1,1,1,1,1,1,1,1,1,1,1,1,1,1,1,1,1,
1,1,1,1,1,1,1,1,1,1,1,1,1,1,1,1,1,1,1,1,1,1,1,1,1,1,1,1,1,1,1,1,1,1,1,1,
1,1,1,1,1,1,1,6),(0.00577184337451611,0.0153846153846154,0.0307692307692308,
0.0461538461538462,0.0615384615384615,0.0769230769230769,0.0923076923076923,
0.107692307692308,0.123076923076923,0.138461538461538,0.153846153846154,
0.169230769230769,0.184615384615385,0.2,0.215384615384615,0.230769230769231,
0.246153846153846,0.261538461538462,0.276923076923077,0.292307692307692,
0.307692307692308,0.323076923076923,0.338461538461538,0.353846153846154,
0.369230769230769,0.384615384615385,0.4,0.415384615384615,0.430769230769231,
0.446153846153846,0.461538461538462,0.476923076923077,0.492307692307692,
0.507692307692308,0.523076923076923,0.538461538461538,0.553846153846154,
0.569230769230769,0.584615384615384,0.6,0.615384615384615,0.63076923076923,
0.646153846153846,0.661538461538461,0.676923076923076,0.692307692307692,
0.707692307692307,0.723076923076922,0.738461538461538,0.753846153846153,
0.769230769230768,0.784615384615384,0.799999999999999,0.815384615384614,
0.83076923076923,0.846153846153845,0.86153846153846,0.876923076923076,0.892307692307691,
0.907692307692306,0.923076923076922,0.938461538461537,0.953846153846152,
0.969230769230768,0.984615384615383,1.),.UNSPECIFIED.)
CURVE()
GEOMETRIC_REPRESENTATION_ITEM()
RATIONAL_B_SPLINE_CURVE((1.,1.,1.,1.,1.,1.,1.,1.,1.,1.,1.,1.,1.,1.,1.,1.,
1.,1.,1.,1.,1.,1.,1.,1.,1.,1.,1.,1.,1.,1.,1.,1.,1.,1.,1.,1.,1.,1.,1.,1.,
1.,1.,1.,1.,1.,1.,1.,1.,1.,1.,1.,1.,1.,1.,1.,1.,1.,1.,1.,1.,1.,1.,1.,1.,
1.,1.,1.,1.,1.,1.))
REPRESENTATION_ITEM('')
);
#288=(
BOUNDED_CURVE()
B_SPLINE_CURVE(5,(#35774,#35775,#35776,#35777,#35778,#35779,#35780,#35781,
#35782,#35783,#35784,#35785,#35786,#35787,#35788,#35789,#35790,#35791,#35792,
#35793,#35794,#35795,#35796,#35797,#35798,#35799,#35800,#35801,#35802,#35803,
#35804,#35805,#35806,#35807,#35808,#35809,#35810,#35811,#35812,#35813,#35814,
#35815,#35816,#35817,#35818,#35819,#35820,#35821,#35822,#35823,#35824,#35825,
#35826,#35827,#35828,#35829,#35830,#35831,#35832,#35833,#35834,#35835,#35836,
#35837,#35838,#35839,#35840,#35841,#35842,#35843),.UNSPECIFIED.,.F.,.F.)
B_SPLINE_CURVE_WITH_KNOTS((6,1,1,1,1,1,1,1,1,1,1,1,1,1,1,1,1,1,1,1,1,1,
1,1,1,1,1,1,1,1,1,1,1,1,1,1,1,1,1,1,1,1,1,1,1,1,1,1,1,1,1,1,1,1,1,1,1,1,
1,1,1,1,1,1,1,6),(0.,0.0153846153846154,0.0307692307692308,0.0461538461538462,
0.0615384615384615,0.0769230769230769,0.0923076923076923,0.107692307692308,
0.123076923076923,0.138461538461538,0.153846153846154,0.169230769230769,
0.184615384615385,0.2,0.215384615384615,0.230769230769231,0.246153846153846,
0.261538461538462,0.276923076923077,0.292307692307692,0.307692307692308,
0.323076923076923,0.338461538461538,0.353846153846154,0.369230769230769,
0.384615384615385,0.4,0.415384615384615,0.430769230769231,0.446153846153846,
0.461538461538462,0.476923076923077,0.492307692307692,0.507692307692308,
0.523076923076923,0.538461538461538,0.553846153846154,0.569230769230769,
0.584615384615384,0.6,0.615384615384615,0.63076923076923,0.646153846153846,
0.661538461538461,0.676923076923076,0.692307692307692,0.707692307692307,
0.723076923076922,0.738461538461538,0.753846153846153,0.769230769230768,
0.784615384615384,0.799999999999999,0.815384615384614,0.83076923076923,
0.846153846153845,0.86153846153846,0.876923076923076,0.892307692307691,
0.907692307692306,0.923076923076922,0.938461538461537,0.953846153846152,
0.969230769230768,0.984615384615383,0.994228156739704),.UNSPECIFIED.)
CURVE()
GEOMETRIC_REPRESENTATION_ITEM()
RATIONAL_B_SPLINE_CURVE((1.,1.,1.,1.,1.,1.,1.,1.,1.,1.,1.,1.,1.,1.,1.,1.,
1.,1.,1.,1.,1.,1.,1.,1.,1.,1.,1.,1.,1.,1.,1.,1.,1.,1.,1.,1.,1.,1.,1.,1.,
1.,1.,1.,1.,1.,1.,1.,1.,1.,1.,1.,1.,1.,1.,1.,1.,1.,1.,1.,1.,1.,1.,1.,1.,
1.,1.,1.,1.,1.,1.))
REPRESENTATION_ITEM('')
);
#289=(
BOUNDED_CURVE()
B_SPLINE_CURVE(5,(#35847,#35848,#35849,#35850,#35851,#35852,#35853,#35854,
#35855,#35856,#35857,#35858,#35859,#35860,#35861,#35862,#35863,#35864,#35865,
#35866,#35867,#35868,#35869,#35870,#35871,#35872,#35873,#35874,#35875,#35876,
#35877,#35878,#35879,#35880,#35881,#35882,#35883,#35884,#35885,#35886,#35887,
#35888,#35889,#35890,#35891,#35892,#35893,#35894,#35895,#35896,#35897,#35898,
#35899,#35900,#35901,#35902,#35903,#35904,#35905,#35906,#35907,#35908,#35909,
#35910,#35911,#35912,#35913,#35914,#35915,#35916),.UNSPECIFIED.,.F.,.F.)
B_SPLINE_CURVE_WITH_KNOTS((6,1,1,1,1,1,1,1,1,1,1,1,1,1,1,1,1,1,1,1,1,1,
1,1,1,1,1,1,1,1,1,1,1,1,1,1,1,1,1,1,1,1,1,1,1,1,1,1,1,1,1,1,1,1,1,1,1,1,
1,1,1,1,1,1,1,6),(0.00577184337449692,0.0153846153846154,0.0307692307692308,
0.0461538461538462,0.0615384615384615,0.0769230769230769,0.0923076923076923,
0.107692307692308,0.123076923076923,0.138461538461538,0.153846153846154,
0.169230769230769,0.184615384615385,0.2,0.215384615384615,0.230769230769231,
0.246153846153846,0.261538461538462,0.276923076923077,0.292307692307692,
0.307692307692308,0.323076923076923,0.338461538461538,0.353846153846154,
0.369230769230769,0.384615384615385,0.4,0.415384615384615,0.430769230769231,
0.446153846153846,0.461538461538462,0.476923076923077,0.492307692307692,
0.507692307692308,0.523076923076923,0.538461538461538,0.553846153846154,
0.569230769230769,0.584615384615384,0.6,0.615384615384615,0.63076923076923,
0.646153846153846,0.661538461538461,0.676923076923076,0.692307692307692,
0.707692307692307,0.723076923076922,0.738461538461538,0.753846153846153,
0.769230769230768,0.784615384615384,0.799999999999999,0.815384615384614,
0.83076923076923,0.846153846153845,0.86153846153846,0.876923076923076,0.892307692307691,
0.907692307692306,0.923076923076922,0.938461538461537,0.953846153846152,
0.969230769230768,0.984615384615383,1.),.UNSPECIFIED.)
CURVE()
GEOMETRIC_REPRESENTATION_ITEM()
RATIONAL_B_SPLINE_CURVE((1.,1.,1.,1.,1.,1.,1.,1.,1.,1.,1.,1.,1.,1.,1.,1.,
1.,1.,1.,1.,1.,1.,1.,1.,1.,1.,1.,1.,1.,1.,1.,1.,1.,1.,1.,1.,1.,1.,1.,1.,
1.,1.,1.,1.,1.,1.,1.,1.,1.,1.,1.,1.,1.,1.,1.,1.,1.,1.,1.,1.,1.,1.,1.,1.,
1.,1.,1.,1.,1.,1.))
REPRESENTATION_ITEM('')
);
#290=(
BOUNDED_CURVE()
B_SPLINE_CURVE(5,(#35919,#35920,#35921,#35922,#35923,#35924,#35925,#35926,
#35927,#35928,#35929,#35930,#35931,#35932,#35933,#35934,#35935,#35936,#35937,
#35938,#35939,#35940,#35941,#35942,#35943,#35944,#35945,#35946,#35947,#35948,
#35949,#35950,#35951,#35952,#35953,#35954,#35955,#35956,#35957,#35958,#35959,
#35960,#35961,#35962,#35963,#35964,#35965,#35966,#35967,#35968,#35969,#35970,
#35971,#35972,#35973,#35974,#35975,#35976,#35977,#35978,#35979,#35980,#35981,
#35982,#35983,#35984,#35985,#35986,#35987,#35988),.UNSPECIFIED.,.F.,.F.)
B_SPLINE_CURVE_WITH_KNOTS((6,1,1,1,1,1,1,1,1,1,1,1,1,1,1,1,1,1,1,1,1,1,
1,1,1,1,1,1,1,1,1,1,1,1,1,1,1,1,1,1,1,1,1,1,1,1,1,1,1,1,1,1,1,1,1,1,1,1,
1,1,1,1,1,1,1,6),(0.,0.0153846153846154,0.0307692307692308,0.0461538461538462,
0.0615384615384615,0.0769230769230769,0.0923076923076923,0.107692307692308,
0.123076923076923,0.138461538461538,0.153846153846154,0.169230769230769,
0.184615384615385,0.2,0.215384615384615,0.230769230769231,0.246153846153846,
0.261538461538462,0.276923076923077,0.292307692307692,0.307692307692308,
0.323076923076923,0.338461538461538,0.353846153846154,0.369230769230769,
0.384615384615385,0.4,0.415384615384615,0.430769230769231,0.446153846153846,
0.461538461538462,0.476923076923077,0.492307692307692,0.507692307692308,
0.523076923076923,0.538461538461538,0.553846153846154,0.569230769230769,
0.584615384615384,0.6,0.615384615384615,0.63076923076923,0.646153846153846,
0.661538461538461,0.676923076923076,0.692307692307692,0.707692307692307,
0.723076923076922,0.738461538461538,0.753846153846153,0.769230769230768,
0.784615384615384,0.799999999999999,0.815384615384614,0.83076923076923,
0.846153846153845,0.86153846153846,0.876923076923076,0.892307692307691,
0.907692307692306,0.923076923076922,0.938461538461537,0.953846153846152,
0.969230769230768,0.984615384615383,0.994228156739723),.UNSPECIFIED.)
CURVE()
GEOMETRIC_REPRESENTATION_ITEM()
RATIONAL_B_SPLINE_CURVE((1.,1.,1.,1.,1.,1.,1.,1.,1.,1.,1.,1.,1.,1.,1.,1.,
1.,1.,1.,1.,1.,1.,1.,1.,1.,1.,1.,1.,1.,1.,1.,1.,1.,1.,1.,1.,1.,1.,1.,1.,
1.,1.,1.,1.,1.,1.,1.,1.,1.,1.,1.,1.,1.,1.,1.,1.,1.,1.,1.,1.,1.,1.,1.,1.,
1.,1.,1.,1.,1.,1.))
REPRESENTATION_ITEM('')
);
#291=(
BOUNDED_CURVE()
B_SPLINE_CURVE(5,(#36147,#36148,#36149,#36150,#36151,#36152,#36153,#36154,
#36155,#36156,#36157,#36158,#36159,#36160,#36161,#36162,#36163,#36164,#36165,
#36166,#36167,#36168,#36169,#36170,#36171,#36172,#36173,#36174,#36175,#36176,
#36177,#36178,#36179,#36180,#36181,#36182,#36183,#36184,#36185,#36186,#36187,
#36188,#36189,#36190,#36191,#36192,#36193,#36194,#36195,#36196,#36197,#36198,
#36199,#36200,#36201,#36202,#36203,#36204,#36205,#36206,#36207,#36208,#36209,
#36210,#36211,#36212,#36213,#36214,#36215,#36216),.UNSPECIFIED.,.F.,.F.)
B_SPLINE_CURVE_WITH_KNOTS((6,1,1,1,1,1,1,1,1,1,1,1,1,1,1,1,1,1,1,1,1,1,
1,1,1,1,1,1,1,1,1,1,1,1,1,1,1,1,1,1,1,1,1,1,1,1,1,1,1,1,1,1,1,1,1,1,1,1,
1,1,1,1,1,1,1,6),(-1.,-0.984615384615383,-0.969230769230768,-0.953846153846152,
-0.938461538461537,-0.923076923076922,-0.907692307692306,-0.892307692307691,
-0.876923076923076,-0.86153846153846,-0.846153846153845,-0.83076923076923,
-0.815384615384614,-0.799999999999999,-0.784615384615384,-0.769230769230768,
-0.753846153846153,-0.738461538461538,-0.723076923076922,-0.707692307692307,
-0.692307692307692,-0.676923076923076,-0.661538461538461,-0.646153846153846,
-0.63076923076923,-0.615384615384615,-0.6,-0.584615384615384,-0.569230769230769,
-0.553846153846154,-0.538461538461538,-0.523076923076923,-0.507692307692308,
-0.492307692307692,-0.476923076923077,-0.461538461538462,-0.446153846153846,
-0.430769230769231,-0.415384615384615,-0.4,-0.384615384615385,-0.369230769230769,
-0.353846153846154,-0.338461538461538,-0.323076923076923,-0.307692307692308,
-0.292307692307692,-0.276923076923077,-0.261538461538462,-0.246153846153846,
-0.230769230769231,-0.215384615384615,-0.2,-0.184615384615385,-0.169230769230769,
-0.153846153846154,-0.138461538461538,-0.123076923076923,-0.107692307692308,
-0.0923076923076923,-0.0769230769230769,-0.0615384615384615,-0.0461538461538462,
-0.0307692307692308,-0.0153846153846154,-0.00577184337448906),
 .UNSPECIFIED.)
CURVE()
GEOMETRIC_REPRESENTATION_ITEM()
RATIONAL_B_SPLINE_CURVE((1.,1.,1.,1.,1.,1.,1.,1.,1.,1.,1.,1.,1.,1.,1.,1.,
1.,1.,1.,1.,1.,1.,1.,1.,1.,1.,1.,1.,1.,1.,1.,1.,1.,1.,1.,1.,1.,1.,1.,1.,
1.,1.,1.,1.,1.,1.,1.,1.,1.,1.,1.,1.,1.,1.,1.,1.,1.,1.,1.,1.,1.,1.,1.,1.,
1.,1.,1.,1.,1.,1.))
REPRESENTATION_ITEM('')
);
#292=(
BOUNDED_CURVE()
B_SPLINE_CURVE(5,(#36367,#36368,#36369,#36370,#36371,#36372,#36373,#36374,
#36375,#36376,#36377,#36378,#36379,#36380,#36381,#36382,#36383,#36384,#36385,
#36386,#36387,#36388,#36389,#36390,#36391,#36392,#36393,#36394,#36395,#36396,
#36397,#36398,#36399,#36400,#36401,#36402,#36403,#36404,#36405,#36406,#36407,
#36408,#36409,#36410,#36411,#36412,#36413,#36414,#36415,#36416,#36417,#36418,
#36419,#36420,#36421,#36422,#36423,#36424,#36425,#36426,#36427,#36428,#36429,
#36430,#36431,#36432,#36433,#36434,#36435,#36436),.UNSPECIFIED.,.F.,.F.)
B_SPLINE_CURVE_WITH_KNOTS((6,1,1,1,1,1,1,1,1,1,1,1,1,1,1,1,1,1,1,1,1,1,
1,1,1,1,1,1,1,1,1,1,1,1,1,1,1,1,1,1,1,1,1,1,1,1,1,1,1,1,1,1,1,1,1,1,1,1,
1,1,1,1,1,1,1,6),(-0.994228156739728,-0.984615384615383,-0.969230769230768,
-0.953846153846152,-0.938461538461537,-0.923076923076922,-0.907692307692306,
-0.892307692307691,-0.876923076923076,-0.86153846153846,-0.846153846153845,
-0.83076923076923,-0.815384615384614,-0.799999999999999,-0.784615384615384,
-0.769230769230768,-0.753846153846153,-0.738461538461538,-0.723076923076922,
-0.707692307692307,-0.692307692307692,-0.676923076923076,-0.661538461538461,
-0.646153846153846,-0.63076923076923,-0.615384615384615,-0.6,-0.584615384615384,
-0.569230769230769,-0.553846153846154,-0.538461538461538,-0.523076923076923,
-0.507692307692308,-0.492307692307692,-0.476923076923077,-0.461538461538462,
-0.446153846153846,-0.430769230769231,-0.415384615384615,-0.4,-0.384615384615385,
-0.369230769230769,-0.353846153846154,-0.338461538461538,-0.323076923076923,
-0.307692307692308,-0.292307692307692,-0.276923076923077,-0.261538461538462,
-0.246153846153846,-0.230769230769231,-0.215384615384615,-0.2,-0.184615384615385,
-0.169230769230769,-0.153846153846154,-0.138461538461538,-0.123076923076923,
-0.107692307692308,-0.0923076923076923,-0.0769230769230769,-0.0615384615384615,
-0.0461538461538462,-0.0307692307692308,-0.0153846153846154,0.),
 .UNSPECIFIED.)
CURVE()
GEOMETRIC_REPRESENTATION_ITEM()
RATIONAL_B_SPLINE_CURVE((1.,1.,1.,1.,1.,1.,1.,1.,1.,1.,1.,1.,1.,1.,1.,1.,
1.,1.,1.,1.,1.,1.,1.,1.,1.,1.,1.,1.,1.,1.,1.,1.,1.,1.,1.,1.,1.,1.,1.,1.,
1.,1.,1.,1.,1.,1.,1.,1.,1.,1.,1.,1.,1.,1.,1.,1.,1.,1.,1.,1.,1.,1.,1.,1.,
1.,1.,1.,1.,1.,1.))
REPRESENTATION_ITEM('')
);
#293=(
BOUNDED_CURVE()
B_SPLINE_CURVE(5,(#36589,#36590,#36591,#36592,#36593,#36594,#36595,#36596,
#36597,#36598,#36599,#36600,#36601,#36602,#36603,#36604,#36605,#36606,#36607,
#36608,#36609,#36610,#36611,#36612,#36613,#36614,#36615,#36616,#36617,#36618,
#36619,#36620,#36621,#36622,#36623,#36624,#36625,#36626,#36627,#36628,#36629,
#36630,#36631,#36632,#36633,#36634,#36635,#36636,#36637,#36638,#36639,#36640,
#36641,#36642,#36643,#36644,#36645,#36646,#36647,#36648,#36649,#36650,#36651,
#36652,#36653,#36654,#36655,#36656,#36657,#36658),.UNSPECIFIED.,.F.,.F.)
B_SPLINE_CURVE_WITH_KNOTS((6,1,1,1,1,1,1,1,1,1,1,1,1,1,1,1,1,1,1,1,1,1,
1,1,1,1,1,1,1,1,1,1,1,1,1,1,1,1,1,1,1,1,1,1,1,1,1,1,1,1,1,1,1,1,1,1,1,1,
1,1,1,1,1,1,1,6),(-1.,-0.984615384615383,-0.969230769230768,-0.953846153846152,
-0.938461538461537,-0.923076923076922,-0.907692307692306,-0.892307692307691,
-0.876923076923076,-0.86153846153846,-0.846153846153845,-0.83076923076923,
-0.815384615384614,-0.799999999999999,-0.784615384615384,-0.769230769230768,
-0.753846153846153,-0.738461538461538,-0.723076923076922,-0.707692307692307,
-0.692307692307692,-0.676923076923076,-0.661538461538461,-0.646153846153846,
-0.63076923076923,-0.615384615384615,-0.6,-0.584615384615384,-0.569230769230769,
-0.553846153846154,-0.538461538461538,-0.523076923076923,-0.507692307692308,
-0.492307692307692,-0.476923076923077,-0.461538461538462,-0.446153846153846,
-0.430769230769231,-0.415384615384615,-0.4,-0.384615384615385,-0.369230769230769,
-0.353846153846154,-0.338461538461538,-0.323076923076923,-0.307692307692308,
-0.292307692307692,-0.276923076923077,-0.261538461538462,-0.246153846153846,
-0.230769230769231,-0.215384615384615,-0.2,-0.184615384615385,-0.169230769230769,
-0.153846153846154,-0.138461538461538,-0.123076923076923,-0.107692307692308,
-0.0923076923076923,-0.0769230769230769,-0.0615384615384615,-0.0461538461538462,
-0.0307692307692308,-0.0153846153846154,-0.0057718433744926),
 .UNSPECIFIED.)
CURVE()
GEOMETRIC_REPRESENTATION_ITEM()
RATIONAL_B_SPLINE_CURVE((1.,1.,1.,1.,1.,1.,1.,1.,1.,1.,1.,1.,1.,1.,1.,1.,
1.,1.,1.,1.,1.,1.,1.,1.,1.,1.,1.,1.,1.,1.,1.,1.,1.,1.,1.,1.,1.,1.,1.,1.,
1.,1.,1.,1.,1.,1.,1.,1.,1.,1.,1.,1.,1.,1.,1.,1.,1.,1.,1.,1.,1.,1.,1.,1.,
1.,1.,1.,1.,1.,1.))
REPRESENTATION_ITEM('')
);
#294=(
BOUNDED_CURVE()
B_SPLINE_CURVE(5,(#36809,#36810,#36811,#36812,#36813,#36814,#36815,#36816,
#36817,#36818,#36819,#36820,#36821,#36822,#36823,#36824,#36825,#36826,#36827,
#36828,#36829,#36830,#36831,#36832,#36833,#36834,#36835,#36836,#36837,#36838,
#36839,#36840,#36841,#36842,#36843,#36844,#36845,#36846,#36847,#36848,#36849,
#36850,#36851,#36852,#36853,#36854,#36855,#36856,#36857,#36858,#36859,#36860,
#36861,#36862,#36863,#36864,#36865,#36866,#36867,#36868,#36869,#36870,#36871,
#36872,#36873,#36874,#36875,#36876,#36877,#36878),.UNSPECIFIED.,.F.,.F.)
B_SPLINE_CURVE_WITH_KNOTS((6,1,1,1,1,1,1,1,1,1,1,1,1,1,1,1,1,1,1,1,1,1,
1,1,1,1,1,1,1,1,1,1,1,1,1,1,1,1,1,1,1,1,1,1,1,1,1,1,1,1,1,1,1,1,1,1,1,1,
1,1,1,1,1,1,1,6),(-0.994228156739718,-0.984615384615383,-0.969230769230768,
-0.953846153846152,-0.938461538461537,-0.923076923076922,-0.907692307692306,
-0.892307692307691,-0.876923076923076,-0.86153846153846,-0.846153846153845,
-0.83076923076923,-0.815384615384614,-0.799999999999999,-0.784615384615384,
-0.769230769230768,-0.753846153846153,-0.738461538461538,-0.723076923076922,
-0.707692307692307,-0.692307692307692,-0.676923076923076,-0.661538461538461,
-0.646153846153846,-0.63076923076923,-0.615384615384615,-0.6,-0.584615384615384,
-0.569230769230769,-0.553846153846154,-0.538461538461538,-0.523076923076923,
-0.507692307692308,-0.492307692307692,-0.476923076923077,-0.461538461538462,
-0.446153846153846,-0.430769230769231,-0.415384615384615,-0.4,-0.384615384615385,
-0.369230769230769,-0.353846153846154,-0.338461538461538,-0.323076923076923,
-0.307692307692308,-0.292307692307692,-0.276923076923077,-0.261538461538462,
-0.246153846153846,-0.230769230769231,-0.215384615384615,-0.2,-0.184615384615385,
-0.169230769230769,-0.153846153846154,-0.138461538461538,-0.123076923076923,
-0.107692307692308,-0.0923076923076923,-0.0769230769230769,-0.0615384615384615,
-0.0461538461538462,-0.0307692307692308,-0.0153846153846154,0.),
 .UNSPECIFIED.)
CURVE()
GEOMETRIC_REPRESENTATION_ITEM()
RATIONAL_B_SPLINE_CURVE((1.,1.,1.,1.,1.,1.,1.,1.,1.,1.,1.,1.,1.,1.,1.,1.,
1.,1.,1.,1.,1.,1.,1.,1.,1.,1.,1.,1.,1.,1.,1.,1.,1.,1.,1.,1.,1.,1.,1.,1.,
1.,1.,1.,1.,1.,1.,1.,1.,1.,1.,1.,1.,1.,1.,1.,1.,1.,1.,1.,1.,1.,1.,1.,1.,
1.,1.,1.,1.,1.,1.))
REPRESENTATION_ITEM('')
);
#295=(
BOUNDED_CURVE()
B_SPLINE_CURVE(5,(#37031,#37032,#37033,#37034,#37035,#37036,#37037,#37038,
#37039,#37040,#37041,#37042,#37043,#37044,#37045,#37046,#37047,#37048,#37049,
#37050,#37051,#37052,#37053,#37054,#37055,#37056,#37057,#37058,#37059,#37060,
#37061,#37062,#37063,#37064,#37065,#37066,#37067,#37068,#37069,#37070,#37071,
#37072,#37073,#37074,#37075,#37076,#37077,#37078,#37079,#37080,#37081,#37082,
#37083,#37084,#37085,#37086,#37087,#37088,#37089,#37090,#37091,#37092,#37093,
#37094,#37095,#37096,#37097,#37098,#37099,#37100),.UNSPECIFIED.,.F.,.F.)
B_SPLINE_CURVE_WITH_KNOTS((6,1,1,1,1,1,1,1,1,1,1,1,1,1,1,1,1,1,1,1,1,1,
1,1,1,1,1,1,1,1,1,1,1,1,1,1,1,1,1,1,1,1,1,1,1,1,1,1,1,1,1,1,1,1,1,1,1,1,
1,1,1,1,1,1,1,6),(-1.,-0.984615384615383,-0.969230769230768,-0.953846153846152,
-0.938461538461537,-0.923076923076922,-0.907692307692306,-0.892307692307691,
-0.876923076923076,-0.86153846153846,-0.846153846153845,-0.83076923076923,
-0.815384615384614,-0.799999999999999,-0.784615384615384,-0.769230769230768,
-0.753846153846153,-0.738461538461538,-0.723076923076922,-0.707692307692307,
-0.692307692307692,-0.676923076923076,-0.661538461538461,-0.646153846153846,
-0.63076923076923,-0.615384615384615,-0.6,-0.584615384615384,-0.569230769230769,
-0.553846153846154,-0.538461538461538,-0.523076923076923,-0.507692307692308,
-0.492307692307692,-0.476923076923077,-0.461538461538462,-0.446153846153846,
-0.430769230769231,-0.415384615384615,-0.4,-0.384615384615385,-0.369230769230769,
-0.353846153846154,-0.338461538461538,-0.323076923076923,-0.307692307692308,
-0.292307692307692,-0.276923076923077,-0.261538461538462,-0.246153846153846,
-0.230769230769231,-0.215384615384615,-0.2,-0.184615384615385,-0.169230769230769,
-0.153846153846154,-0.138461538461538,-0.123076923076923,-0.107692307692308,
-0.0923076923076923,-0.0769230769230769,-0.0615384615384615,-0.0461538461538462,
-0.0307692307692308,-0.0153846153846154,-0.00577184337449396),
 .UNSPECIFIED.)
CURVE()
GEOMETRIC_REPRESENTATION_ITEM()
RATIONAL_B_SPLINE_CURVE((1.,1.,1.,1.,1.,1.,1.,1.,1.,1.,1.,1.,1.,1.,1.,1.,
1.,1.,1.,1.,1.,1.,1.,1.,1.,1.,1.,1.,1.,1.,1.,1.,1.,1.,1.,1.,1.,1.,1.,1.,
1.,1.,1.,1.,1.,1.,1.,1.,1.,1.,1.,1.,1.,1.,1.,1.,1.,1.,1.,1.,1.,1.,1.,1.,
1.,1.,1.,1.,1.,1.))
REPRESENTATION_ITEM('')
);
#296=(
BOUNDED_CURVE()
B_SPLINE_CURVE(5,(#37251,#37252,#37253,#37254,#37255,#37256,#37257,#37258,
#37259,#37260,#37261,#37262,#37263,#37264,#37265,#37266,#37267,#37268,#37269,
#37270,#37271,#37272,#37273,#37274,#37275,#37276,#37277,#37278,#37279,#37280,
#37281,#37282,#37283,#37284,#37285,#37286,#37287,#37288,#37289,#37290,#37291,
#37292,#37293,#37294,#37295,#37296,#37297,#37298,#37299,#37300,#37301,#37302,
#37303,#37304,#37305,#37306,#37307,#37308,#37309,#37310,#37311,#37312,#37313,
#37314,#37315,#37316,#37317,#37318,#37319,#37320),.UNSPECIFIED.,.F.,.F.)
B_SPLINE_CURVE_WITH_KNOTS((6,1,1,1,1,1,1,1,1,1,1,1,1,1,1,1,1,1,1,1,1,1,
1,1,1,1,1,1,1,1,1,1,1,1,1,1,1,1,1,1,1,1,1,1,1,1,1,1,1,1,1,1,1,1,1,1,1,1,
1,1,1,1,1,1,1,6),(-0.994228156739702,-0.984615384615383,-0.969230769230768,
-0.953846153846152,-0.938461538461537,-0.923076923076922,-0.907692307692306,
-0.892307692307691,-0.876923076923076,-0.86153846153846,-0.846153846153845,
-0.83076923076923,-0.815384615384614,-0.799999999999999,-0.784615384615384,
-0.769230769230768,-0.753846153846153,-0.738461538461538,-0.723076923076922,
-0.707692307692307,-0.692307692307692,-0.676923076923076,-0.661538461538461,
-0.646153846153846,-0.63076923076923,-0.615384615384615,-0.6,-0.584615384615384,
-0.569230769230769,-0.553846153846154,-0.538461538461538,-0.523076923076923,
-0.507692307692308,-0.492307692307692,-0.476923076923077,-0.461538461538462,
-0.446153846153846,-0.430769230769231,-0.415384615384615,-0.4,-0.384615384615385,
-0.369230769230769,-0.353846153846154,-0.338461538461538,-0.323076923076923,
-0.307692307692308,-0.292307692307692,-0.276923076923077,-0.261538461538462,
-0.246153846153846,-0.230769230769231,-0.215384615384615,-0.2,-0.184615384615385,
-0.169230769230769,-0.153846153846154,-0.138461538461538,-0.123076923076923,
-0.107692307692308,-0.0923076923076923,-0.0769230769230769,-0.0615384615384615,
-0.0461538461538462,-0.0307692307692308,-0.0153846153846154,0.),
 .UNSPECIFIED.)
CURVE()
GEOMETRIC_REPRESENTATION_ITEM()
RATIONAL_B_SPLINE_CURVE((1.,1.,1.,1.,1.,1.,1.,1.,1.,1.,1.,1.,1.,1.,1.,1.,
1.,1.,1.,1.,1.,1.,1.,1.,1.,1.,1.,1.,1.,1.,1.,1.,1.,1.,1.,1.,1.,1.,1.,1.,
1.,1.,1.,1.,1.,1.,1.,1.,1.,1.,1.,1.,1.,1.,1.,1.,1.,1.,1.,1.,1.,1.,1.,1.,
1.,1.,1.,1.,1.,1.))
REPRESENTATION_ITEM('')
);
#297=(
BOUNDED_CURVE()
B_SPLINE_CURVE(5,(#37473,#37474,#37475,#37476,#37477,#37478,#37479,#37480,
#37481,#37482,#37483,#37484,#37485,#37486,#37487,#37488,#37489,#37490,#37491,
#37492,#37493,#37494,#37495,#37496,#37497,#37498,#37499,#37500,#37501,#37502,
#37503,#37504,#37505,#37506,#37507,#37508,#37509,#37510,#37511,#37512,#37513,
#37514,#37515,#37516,#37517,#37518,#37519,#37520,#37521,#37522,#37523,#37524,
#37525,#37526,#37527,#37528,#37529,#37530,#37531,#37532,#37533,#37534,#37535,
#37536,#37537,#37538,#37539,#37540,#37541,#37542),.UNSPECIFIED.,.F.,.F.)
B_SPLINE_CURVE_WITH_KNOTS((6,1,1,1,1,1,1,1,1,1,1,1,1,1,1,1,1,1,1,1,1,1,
1,1,1,1,1,1,1,1,1,1,1,1,1,1,1,1,1,1,1,1,1,1,1,1,1,1,1,1,1,1,1,1,1,1,1,1,
1,1,1,1,1,1,1,6),(-1.,-0.984615384615383,-0.969230769230768,-0.953846153846152,
-0.938461538461537,-0.923076923076922,-0.907692307692306,-0.892307692307691,
-0.876923076923076,-0.86153846153846,-0.846153846153845,-0.83076923076923,
-0.815384615384614,-0.799999999999999,-0.784615384615384,-0.769230769230768,
-0.753846153846153,-0.738461538461538,-0.723076923076922,-0.707692307692307,
-0.692307692307692,-0.676923076923076,-0.661538461538461,-0.646153846153846,
-0.63076923076923,-0.615384615384615,-0.6,-0.584615384615384,-0.569230769230769,
-0.553846153846154,-0.538461538461538,-0.523076923076923,-0.507692307692308,
-0.492307692307692,-0.476923076923077,-0.461538461538462,-0.446153846153846,
-0.430769230769231,-0.415384615384615,-0.4,-0.384615384615385,-0.369230769230769,
-0.353846153846154,-0.338461538461538,-0.323076923076923,-0.307692307692308,
-0.292307692307692,-0.276923076923077,-0.261538461538462,-0.246153846153846,
-0.230769230769231,-0.215384615384615,-0.2,-0.184615384615385,-0.169230769230769,
-0.153846153846154,-0.138461538461538,-0.123076923076923,-0.107692307692308,
-0.0923076923076923,-0.0769230769230769,-0.0615384615384615,-0.0461538461538462,
-0.0307692307692308,-0.0153846153846154,-0.00577184337450989),
 .UNSPECIFIED.)
CURVE()
GEOMETRIC_REPRESENTATION_ITEM()
RATIONAL_B_SPLINE_CURVE((1.,1.,1.,1.,1.,1.,1.,1.,1.,1.,1.,1.,1.,1.,1.,1.,
1.,1.,1.,1.,1.,1.,1.,1.,1.,1.,1.,1.,1.,1.,1.,1.,1.,1.,1.,1.,1.,1.,1.,1.,
1.,1.,1.,1.,1.,1.,1.,1.,1.,1.,1.,1.,1.,1.,1.,1.,1.,1.,1.,1.,1.,1.,1.,1.,
1.,1.,1.,1.,1.,1.))
REPRESENTATION_ITEM('')
);
#298=(
BOUNDED_CURVE()
B_SPLINE_CURVE(5,(#37693,#37694,#37695,#37696,#37697,#37698,#37699,#37700,
#37701,#37702,#37703,#37704,#37705,#37706,#37707,#37708,#37709,#37710,#37711,
#37712,#37713,#37714,#37715,#37716,#37717,#37718,#37719,#37720,#37721,#37722,
#37723,#37724,#37725,#37726,#37727,#37728,#37729,#37730,#37731,#37732,#37733,
#37734,#37735,#37736,#37737,#37738,#37739,#37740,#37741,#37742,#37743,#37744,
#37745,#37746,#37747,#37748,#37749,#37750,#37751,#37752,#37753,#37754,#37755,
#37756,#37757,#37758,#37759,#37760,#37761,#37762),.UNSPECIFIED.,.F.,.F.)
B_SPLINE_CURVE_WITH_KNOTS((6,1,1,1,1,1,1,1,1,1,1,1,1,1,1,1,1,1,1,1,1,1,
1,1,1,1,1,1,1,1,1,1,1,1,1,1,1,1,1,1,1,1,1,1,1,1,1,1,1,1,1,1,1,1,1,1,1,1,
1,1,1,1,1,1,1,6),(-0.994228156739736,-0.984615384615383,-0.969230769230768,
-0.953846153846152,-0.938461538461537,-0.923076923076922,-0.907692307692306,
-0.892307692307691,-0.876923076923076,-0.86153846153846,-0.846153846153845,
-0.83076923076923,-0.815384615384614,-0.799999999999999,-0.784615384615384,
-0.769230769230768,-0.753846153846153,-0.738461538461538,-0.723076923076922,
-0.707692307692307,-0.692307692307692,-0.676923076923076,-0.661538461538461,
-0.646153846153846,-0.63076923076923,-0.615384615384615,-0.6,-0.584615384615384,
-0.569230769230769,-0.553846153846154,-0.538461538461538,-0.523076923076923,
-0.507692307692308,-0.492307692307692,-0.476923076923077,-0.461538461538462,
-0.446153846153846,-0.430769230769231,-0.415384615384615,-0.4,-0.384615384615385,
-0.369230769230769,-0.353846153846154,-0.338461538461538,-0.323076923076923,
-0.307692307692308,-0.292307692307692,-0.276923076923077,-0.261538461538462,
-0.246153846153846,-0.230769230769231,-0.215384615384615,-0.2,-0.184615384615385,
-0.169230769230769,-0.153846153846154,-0.138461538461538,-0.123076923076923,
-0.107692307692308,-0.0923076923076923,-0.0769230769230769,-0.0615384615384615,
-0.0461538461538462,-0.0307692307692308,-0.0153846153846154,0.),
 .UNSPECIFIED.)
CURVE()
GEOMETRIC_REPRESENTATION_ITEM()
RATIONAL_B_SPLINE_CURVE((1.,1.,1.,1.,1.,1.,1.,1.,1.,1.,1.,1.,1.,1.,1.,1.,
1.,1.,1.,1.,1.,1.,1.,1.,1.,1.,1.,1.,1.,1.,1.,1.,1.,1.,1.,1.,1.,1.,1.,1.,
1.,1.,1.,1.,1.,1.,1.,1.,1.,1.,1.,1.,1.,1.,1.,1.,1.,1.,1.,1.,1.,1.,1.,1.,
1.,1.,1.,1.,1.,1.))
REPRESENTATION_ITEM('')
);
#299=(
BOUNDED_CURVE()
B_SPLINE_CURVE(5,(#37915,#37916,#37917,#37918,#37919,#37920,#37921,#37922,
#37923,#37924,#37925,#37926,#37927,#37928,#37929,#37930,#37931,#37932,#37933,
#37934,#37935,#37936,#37937,#37938,#37939,#37940,#37941,#37942,#37943,#37944,
#37945,#37946,#37947,#37948,#37949,#37950,#37951,#37952,#37953,#37954,#37955,
#37956,#37957,#37958,#37959,#37960,#37961,#37962,#37963,#37964,#37965,#37966,
#37967,#37968,#37969,#37970,#37971,#37972,#37973,#37974,#37975,#37976,#37977,
#37978,#37979,#37980,#37981,#37982,#37983,#37984),.UNSPECIFIED.,.F.,.F.)
B_SPLINE_CURVE_WITH_KNOTS((6,1,1,1,1,1,1,1,1,1,1,1,1,1,1,1,1,1,1,1,1,1,
1,1,1,1,1,1,1,1,1,1,1,1,1,1,1,1,1,1,1,1,1,1,1,1,1,1,1,1,1,1,1,1,1,1,1,1,
1,1,1,1,1,1,1,6),(-1.,-0.984615384615383,-0.969230769230768,-0.953846153846152,
-0.938461538461537,-0.923076923076922,-0.907692307692306,-0.892307692307691,
-0.876923076923076,-0.86153846153846,-0.846153846153845,-0.83076923076923,
-0.815384615384614,-0.799999999999999,-0.784615384615384,-0.769230769230768,
-0.753846153846153,-0.738461538461538,-0.723076923076922,-0.707692307692307,
-0.692307692307692,-0.676923076923076,-0.661538461538461,-0.646153846153846,
-0.63076923076923,-0.615384615384615,-0.6,-0.584615384615384,-0.569230769230769,
-0.553846153846154,-0.538461538461538,-0.523076923076923,-0.507692307692308,
-0.492307692307692,-0.476923076923077,-0.461538461538462,-0.446153846153846,
-0.430769230769231,-0.415384615384615,-0.4,-0.384615384615385,-0.369230769230769,
-0.353846153846154,-0.338461538461538,-0.323076923076923,-0.307692307692308,
-0.292307692307692,-0.276923076923077,-0.261538461538462,-0.246153846153846,
-0.230769230769231,-0.215384615384615,-0.2,-0.184615384615385,-0.169230769230769,
-0.153846153846154,-0.138461538461538,-0.123076923076923,-0.107692307692308,
-0.0923076923076923,-0.0769230769230769,-0.0615384615384615,-0.0461538461538462,
-0.0307692307692308,-0.0153846153846154,-0.00577184337452469),
 .UNSPECIFIED.)
CURVE()
GEOMETRIC_REPRESENTATION_ITEM()
RATIONAL_B_SPLINE_CURVE((1.,1.,1.,1.,1.,1.,1.,1.,1.,1.,1.,1.,1.,1.,1.,1.,
1.,1.,1.,1.,1.,1.,1.,1.,1.,1.,1.,1.,1.,1.,1.,1.,1.,1.,1.,1.,1.,1.,1.,1.,
1.,1.,1.,1.,1.,1.,1.,1.,1.,1.,1.,1.,1.,1.,1.,1.,1.,1.,1.,1.,1.,1.,1.,1.,
1.,1.,1.,1.,1.,1.))
REPRESENTATION_ITEM('')
);
#300=(
BOUNDED_CURVE()
B_SPLINE_CURVE(5,(#38135,#38136,#38137,#38138,#38139,#38140,#38141,#38142,
#38143,#38144,#38145,#38146,#38147,#38148,#38149,#38150,#38151,#38152,#38153,
#38154,#38155,#38156,#38157,#38158,#38159,#38160,#38161,#38162,#38163,#38164,
#38165,#38166,#38167,#38168,#38169,#38170,#38171,#38172,#38173,#38174,#38175,
#38176,#38177,#38178,#38179,#38180,#38181,#38182,#38183,#38184,#38185,#38186,
#38187,#38188,#38189,#38190,#38191,#38192,#38193,#38194,#38195,#38196,#38197,
#38198,#38199,#38200,#38201,#38202,#38203,#38204),.UNSPECIFIED.,.F.,.F.)
B_SPLINE_CURVE_WITH_KNOTS((6,1,1,1,1,1,1,1,1,1,1,1,1,1,1,1,1,1,1,1,1,1,
1,1,1,1,1,1,1,1,1,1,1,1,1,1,1,1,1,1,1,1,1,1,1,1,1,1,1,1,1,1,1,1,1,1,1,1,
1,1,1,1,1,1,1,6),(-0.994228156739717,-0.984615384615383,-0.969230769230768,
-0.953846153846152,-0.938461538461537,-0.923076923076922,-0.907692307692306,
-0.892307692307691,-0.876923076923076,-0.86153846153846,-0.846153846153845,
-0.83076923076923,-0.815384615384614,-0.799999999999999,-0.784615384615384,
-0.769230769230768,-0.753846153846153,-0.738461538461538,-0.723076923076922,
-0.707692307692307,-0.692307692307692,-0.676923076923076,-0.661538461538461,
-0.646153846153846,-0.63076923076923,-0.615384615384615,-0.6,-0.584615384615384,
-0.569230769230769,-0.553846153846154,-0.538461538461538,-0.523076923076923,
-0.507692307692308,-0.492307692307692,-0.476923076923077,-0.461538461538462,
-0.446153846153846,-0.430769230769231,-0.415384615384615,-0.4,-0.384615384615385,
-0.369230769230769,-0.353846153846154,-0.338461538461538,-0.323076923076923,
-0.307692307692308,-0.292307692307692,-0.276923076923077,-0.261538461538462,
-0.246153846153846,-0.230769230769231,-0.215384615384615,-0.2,-0.184615384615385,
-0.169230769230769,-0.153846153846154,-0.138461538461538,-0.123076923076923,
-0.107692307692308,-0.0923076923076923,-0.0769230769230769,-0.0615384615384615,
-0.0461538461538462,-0.0307692307692308,-0.0153846153846154,0.),
 .UNSPECIFIED.)
CURVE()
GEOMETRIC_REPRESENTATION_ITEM()
RATIONAL_B_SPLINE_CURVE((1.,1.,1.,1.,1.,1.,1.,1.,1.,1.,1.,1.,1.,1.,1.,1.,
1.,1.,1.,1.,1.,1.,1.,1.,1.,1.,1.,1.,1.,1.,1.,1.,1.,1.,1.,1.,1.,1.,1.,1.,
1.,1.,1.,1.,1.,1.,1.,1.,1.,1.,1.,1.,1.,1.,1.,1.,1.,1.,1.,1.,1.,1.,1.,1.,
1.,1.,1.,1.,1.,1.))
REPRESENTATION_ITEM('')
);
#301=(
BOUNDED_CURVE()
B_SPLINE_CURVE(5,(#38357,#38358,#38359,#38360,#38361,#38362,#38363,#38364,
#38365,#38366,#38367,#38368,#38369,#38370,#38371,#38372,#38373,#38374,#38375,
#38376,#38377,#38378,#38379,#38380,#38381,#38382,#38383,#38384,#38385,#38386,
#38387,#38388,#38389,#38390,#38391,#38392,#38393,#38394,#38395,#38396,#38397,
#38398,#38399,#38400,#38401,#38402,#38403,#38404,#38405,#38406,#38407,#38408,
#38409,#38410,#38411,#38412,#38413,#38414,#38415,#38416,#38417,#38418,#38419,
#38420,#38421,#38422,#38423,#38424,#38425,#38426),.UNSPECIFIED.,.F.,.F.)
B_SPLINE_CURVE_WITH_KNOTS((6,1,1,1,1,1,1,1,1,1,1,1,1,1,1,1,1,1,1,1,1,1,
1,1,1,1,1,1,1,1,1,1,1,1,1,1,1,1,1,1,1,1,1,1,1,1,1,1,1,1,1,1,1,1,1,1,1,1,
1,1,1,1,1,1,1,6),(-1.,-0.984615384615383,-0.969230769230768,-0.953846153846152,
-0.938461538461537,-0.923076923076922,-0.907692307692306,-0.892307692307691,
-0.876923076923076,-0.86153846153846,-0.846153846153845,-0.83076923076923,
-0.815384615384614,-0.799999999999999,-0.784615384615384,-0.769230769230768,
-0.753846153846153,-0.738461538461538,-0.723076923076922,-0.707692307692307,
-0.692307692307692,-0.676923076923076,-0.661538461538461,-0.646153846153846,
-0.63076923076923,-0.615384615384615,-0.6,-0.584615384615384,-0.569230769230769,
-0.553846153846154,-0.538461538461538,-0.523076923076923,-0.507692307692308,
-0.492307692307692,-0.476923076923077,-0.461538461538462,-0.446153846153846,
-0.430769230769231,-0.415384615384615,-0.4,-0.384615384615385,-0.369230769230769,
-0.353846153846154,-0.338461538461538,-0.323076923076923,-0.307692307692308,
-0.292307692307692,-0.276923076923077,-0.261538461538462,-0.246153846153846,
-0.230769230769231,-0.215384615384615,-0.2,-0.184615384615385,-0.169230769230769,
-0.153846153846154,-0.138461538461538,-0.123076923076923,-0.107692307692308,
-0.0923076923076923,-0.0769230769230769,-0.0615384615384615,-0.0461538461538462,
-0.0307692307692308,-0.0153846153846154,-0.00577184337453472),
 .UNSPECIFIED.)
CURVE()
GEOMETRIC_REPRESENTATION_ITEM()
RATIONAL_B_SPLINE_CURVE((1.,1.,1.,1.,1.,1.,1.,1.,1.,1.,1.,1.,1.,1.,1.,1.,
1.,1.,1.,1.,1.,1.,1.,1.,1.,1.,1.,1.,1.,1.,1.,1.,1.,1.,1.,1.,1.,1.,1.,1.,
1.,1.,1.,1.,1.,1.,1.,1.,1.,1.,1.,1.,1.,1.,1.,1.,1.,1.,1.,1.,1.,1.,1.,1.,
1.,1.,1.,1.,1.,1.))
REPRESENTATION_ITEM('')
);
#302=(
BOUNDED_CURVE()
B_SPLINE_CURVE(5,(#38577,#38578,#38579,#38580,#38581,#38582,#38583,#38584,
#38585,#38586,#38587,#38588,#38589,#38590,#38591,#38592,#38593,#38594,#38595,
#38596,#38597,#38598,#38599,#38600,#38601,#38602,#38603,#38604,#38605,#38606,
#38607,#38608,#38609,#38610,#38611,#38612,#38613,#38614,#38615,#38616,#38617,
#38618,#38619,#38620,#38621,#38622,#38623,#38624,#38625,#38626,#38627,#38628,
#38629,#38630,#38631,#38632,#38633,#38634,#38635,#38636,#38637,#38638,#38639,
#38640,#38641,#38642,#38643,#38644,#38645,#38646),.UNSPECIFIED.,.F.,.F.)
B_SPLINE_CURVE_WITH_KNOTS((6,1,1,1,1,1,1,1,1,1,1,1,1,1,1,1,1,1,1,1,1,1,
1,1,1,1,1,1,1,1,1,1,1,1,1,1,1,1,1,1,1,1,1,1,1,1,1,1,1,1,1,1,1,1,1,1,1,1,
1,1,1,1,1,1,1,6),(-0.994228156739652,-0.984615384615383,-0.969230769230768,
-0.953846153846152,-0.938461538461537,-0.923076923076922,-0.907692307692306,
-0.892307692307691,-0.876923076923076,-0.86153846153846,-0.846153846153845,
-0.83076923076923,-0.815384615384614,-0.799999999999999,-0.784615384615384,
-0.769230769230768,-0.753846153846153,-0.738461538461538,-0.723076923076922,
-0.707692307692307,-0.692307692307692,-0.676923076923076,-0.661538461538461,
-0.646153846153846,-0.63076923076923,-0.615384615384615,-0.6,-0.584615384615384,
-0.569230769230769,-0.553846153846154,-0.538461538461538,-0.523076923076923,
-0.507692307692308,-0.492307692307692,-0.476923076923077,-0.461538461538462,
-0.446153846153846,-0.430769230769231,-0.415384615384615,-0.4,-0.384615384615385,
-0.369230769230769,-0.353846153846154,-0.338461538461538,-0.323076923076923,
-0.307692307692308,-0.292307692307692,-0.276923076923077,-0.261538461538462,
-0.246153846153846,-0.230769230769231,-0.215384615384615,-0.2,-0.184615384615385,
-0.169230769230769,-0.153846153846154,-0.138461538461538,-0.123076923076923,
-0.107692307692308,-0.0923076923076923,-0.0769230769230769,-0.0615384615384615,
-0.0461538461538462,-0.0307692307692308,-0.0153846153846154,0.),
 .UNSPECIFIED.)
CURVE()
GEOMETRIC_REPRESENTATION_ITEM()
RATIONAL_B_SPLINE_CURVE((1.,1.,1.,1.,1.,1.,1.,1.,1.,1.,1.,1.,1.,1.,1.,1.,
1.,1.,1.,1.,1.,1.,1.,1.,1.,1.,1.,1.,1.,1.,1.,1.,1.,1.,1.,1.,1.,1.,1.,1.,
1.,1.,1.,1.,1.,1.,1.,1.,1.,1.,1.,1.,1.,1.,1.,1.,1.,1.,1.,1.,1.,1.,1.,1.,
1.,1.,1.,1.,1.,1.))
REPRESENTATION_ITEM('')
);
#303=(
BOUNDED_CURVE()
B_SPLINE_CURVE(5,(#38799,#38800,#38801,#38802,#38803,#38804,#38805,#38806,
#38807,#38808,#38809,#38810,#38811,#38812,#38813,#38814,#38815,#38816,#38817,
#38818,#38819,#38820,#38821,#38822,#38823,#38824,#38825,#38826,#38827,#38828,
#38829,#38830,#38831,#38832,#38833,#38834,#38835,#38836,#38837,#38838,#38839,
#38840,#38841,#38842,#38843,#38844,#38845,#38846,#38847,#38848,#38849,#38850,
#38851,#38852,#38853,#38854,#38855,#38856,#38857,#38858,#38859,#38860,#38861,
#38862,#38863,#38864,#38865,#38866,#38867,#38868),.UNSPECIFIED.,.F.,.F.)
B_SPLINE_CURVE_WITH_KNOTS((6,1,1,1,1,1,1,1,1,1,1,1,1,1,1,1,1,1,1,1,1,1,
1,1,1,1,1,1,1,1,1,1,1,1,1,1,1,1,1,1,1,1,1,1,1,1,1,1,1,1,1,1,1,1,1,1,1,1,
1,1,1,1,1,1,1,6),(-1.,-0.984615384615383,-0.969230769230768,-0.953846153846152,
-0.938461538461537,-0.923076923076922,-0.907692307692306,-0.892307692307691,
-0.876923076923076,-0.86153846153846,-0.846153846153845,-0.83076923076923,
-0.815384615384614,-0.799999999999999,-0.784615384615384,-0.769230769230768,
-0.753846153846153,-0.738461538461538,-0.723076923076922,-0.707692307692307,
-0.692307692307692,-0.676923076923076,-0.661538461538461,-0.646153846153846,
-0.63076923076923,-0.615384615384615,-0.6,-0.584615384615384,-0.569230769230769,
-0.553846153846154,-0.538461538461538,-0.523076923076923,-0.507692307692308,
-0.492307692307692,-0.476923076923077,-0.461538461538462,-0.446153846153846,
-0.430769230769231,-0.415384615384615,-0.4,-0.384615384615385,-0.369230769230769,
-0.353846153846154,-0.338461538461538,-0.323076923076923,-0.307692307692308,
-0.292307692307692,-0.276923076923077,-0.261538461538462,-0.246153846153846,
-0.230769230769231,-0.215384615384615,-0.2,-0.184615384615385,-0.169230769230769,
-0.153846153846154,-0.138461538461538,-0.123076923076923,-0.107692307692308,
-0.0923076923076923,-0.0769230769230769,-0.0615384615384615,-0.0461538461538462,
-0.0307692307692308,-0.0153846153846154,-0.00577184337450876),
 .UNSPECIFIED.)
CURVE()
GEOMETRIC_REPRESENTATION_ITEM()
RATIONAL_B_SPLINE_CURVE((1.,1.,1.,1.,1.,1.,1.,1.,1.,1.,1.,1.,1.,1.,1.,1.,
1.,1.,1.,1.,1.,1.,1.,1.,1.,1.,1.,1.,1.,1.,1.,1.,1.,1.,1.,1.,1.,1.,1.,1.,
1.,1.,1.,1.,1.,1.,1.,1.,1.,1.,1.,1.,1.,1.,1.,1.,1.,1.,1.,1.,1.,1.,1.,1.,
1.,1.,1.,1.,1.,1.))
REPRESENTATION_ITEM('')
);
#304=(
BOUNDED_CURVE()
B_SPLINE_CURVE(5,(#39019,#39020,#39021,#39022,#39023,#39024,#39025,#39026,
#39027,#39028,#39029,#39030,#39031,#39032,#39033,#39034,#39035,#39036,#39037,
#39038,#39039,#39040,#39041,#39042,#39043,#39044,#39045,#39046,#39047,#39048,
#39049,#39050,#39051,#39052,#39053,#39054,#39055,#39056,#39057,#39058,#39059,
#39060,#39061,#39062,#39063,#39064,#39065,#39066,#39067,#39068,#39069,#39070,
#39071,#39072,#39073,#39074,#39075,#39076,#39077,#39078,#39079,#39080,#39081,
#39082,#39083,#39084,#39085,#39086,#39087,#39088),.UNSPECIFIED.,.F.,.F.)
B_SPLINE_CURVE_WITH_KNOTS((6,1,1,1,1,1,1,1,1,1,1,1,1,1,1,1,1,1,1,1,1,1,
1,1,1,1,1,1,1,1,1,1,1,1,1,1,1,1,1,1,1,1,1,1,1,1,1,1,1,1,1,1,1,1,1,1,1,1,
1,1,1,1,1,1,1,6),(-0.994228156739683,-0.984615384615383,-0.969230769230768,
-0.953846153846152,-0.938461538461537,-0.923076923076922,-0.907692307692306,
-0.892307692307691,-0.876923076923076,-0.86153846153846,-0.846153846153845,
-0.83076923076923,-0.815384615384614,-0.799999999999999,-0.784615384615384,
-0.769230769230768,-0.753846153846153,-0.738461538461538,-0.723076923076922,
-0.707692307692307,-0.692307692307692,-0.676923076923076,-0.661538461538461,
-0.646153846153846,-0.63076923076923,-0.615384615384615,-0.6,-0.584615384615384,
-0.569230769230769,-0.553846153846154,-0.538461538461538,-0.523076923076923,
-0.507692307692308,-0.492307692307692,-0.476923076923077,-0.461538461538462,
-0.446153846153846,-0.430769230769231,-0.415384615384615,-0.4,-0.384615384615385,
-0.369230769230769,-0.353846153846154,-0.338461538461538,-0.323076923076923,
-0.307692307692308,-0.292307692307692,-0.276923076923077,-0.261538461538462,
-0.246153846153846,-0.230769230769231,-0.215384615384615,-0.2,-0.184615384615385,
-0.169230769230769,-0.153846153846154,-0.138461538461538,-0.123076923076923,
-0.107692307692308,-0.0923076923076923,-0.0769230769230769,-0.0615384615384615,
-0.0461538461538462,-0.0307692307692308,-0.0153846153846154,0.),
 .UNSPECIFIED.)
CURVE()
GEOMETRIC_REPRESENTATION_ITEM()
RATIONAL_B_SPLINE_CURVE((1.,1.,1.,1.,1.,1.,1.,1.,1.,1.,1.,1.,1.,1.,1.,1.,
1.,1.,1.,1.,1.,1.,1.,1.,1.,1.,1.,1.,1.,1.,1.,1.,1.,1.,1.,1.,1.,1.,1.,1.,
1.,1.,1.,1.,1.,1.,1.,1.,1.,1.,1.,1.,1.,1.,1.,1.,1.,1.,1.,1.,1.,1.,1.,1.,
1.,1.,1.,1.,1.,1.))
REPRESENTATION_ITEM('')
);
#305=(
BOUNDED_CURVE()
B_SPLINE_CURVE(5,(#39241,#39242,#39243,#39244,#39245,#39246,#39247,#39248,
#39249,#39250,#39251,#39252,#39253,#39254,#39255,#39256,#39257,#39258,#39259,
#39260,#39261,#39262,#39263,#39264,#39265,#39266,#39267,#39268,#39269,#39270,
#39271,#39272,#39273,#39274,#39275,#39276,#39277,#39278,#39279,#39280,#39281,
#39282,#39283,#39284,#39285,#39286,#39287,#39288,#39289,#39290,#39291,#39292,
#39293,#39294,#39295,#39296,#39297,#39298,#39299,#39300,#39301,#39302,#39303,
#39304,#39305,#39306,#39307,#39308,#39309,#39310),.UNSPECIFIED.,.F.,.F.)
B_SPLINE_CURVE_WITH_KNOTS((6,1,1,1,1,1,1,1,1,1,1,1,1,1,1,1,1,1,1,1,1,1,
1,1,1,1,1,1,1,1,1,1,1,1,1,1,1,1,1,1,1,1,1,1,1,1,1,1,1,1,1,1,1,1,1,1,1,1,
1,1,1,1,1,1,1,6),(-1.,-0.984615384615383,-0.969230769230768,-0.953846153846152,
-0.938461538461537,-0.923076923076922,-0.907692307692306,-0.892307692307691,
-0.876923076923076,-0.86153846153846,-0.846153846153845,-0.83076923076923,
-0.815384615384614,-0.799999999999999,-0.784615384615384,-0.769230769230768,
-0.753846153846153,-0.738461538461538,-0.723076923076922,-0.707692307692307,
-0.692307692307692,-0.676923076923076,-0.661538461538461,-0.646153846153846,
-0.63076923076923,-0.615384615384615,-0.6,-0.584615384615384,-0.569230769230769,
-0.553846153846154,-0.538461538461538,-0.523076923076923,-0.507692307692308,
-0.492307692307692,-0.476923076923077,-0.461538461538462,-0.446153846153846,
-0.430769230769231,-0.415384615384615,-0.4,-0.384615384615385,-0.369230769230769,
-0.353846153846154,-0.338461538461538,-0.323076923076923,-0.307692307692308,
-0.292307692307692,-0.276923076923077,-0.261538461538462,-0.246153846153846,
-0.230769230769231,-0.215384615384615,-0.2,-0.184615384615385,-0.169230769230769,
-0.153846153846154,-0.138461538461538,-0.123076923076923,-0.107692307692308,
-0.0923076923076923,-0.0769230769230769,-0.0615384615384615,-0.0461538461538462,
-0.0307692307692308,-0.0153846153846154,-0.00577184337450277),
 .UNSPECIFIED.)
CURVE()
GEOMETRIC_REPRESENTATION_ITEM()
RATIONAL_B_SPLINE_CURVE((1.,1.,1.,1.,1.,1.,1.,1.,1.,1.,1.,1.,1.,1.,1.,1.,
1.,1.,1.,1.,1.,1.,1.,1.,1.,1.,1.,1.,1.,1.,1.,1.,1.,1.,1.,1.,1.,1.,1.,1.,
1.,1.,1.,1.,1.,1.,1.,1.,1.,1.,1.,1.,1.,1.,1.,1.,1.,1.,1.,1.,1.,1.,1.,1.,
1.,1.,1.,1.,1.,1.))
REPRESENTATION_ITEM('')
);
#306=(
BOUNDED_CURVE()
B_SPLINE_CURVE(5,(#39461,#39462,#39463,#39464,#39465,#39466,#39467,#39468,
#39469,#39470,#39471,#39472,#39473,#39474,#39475,#39476,#39477,#39478,#39479,
#39480,#39481,#39482,#39483,#39484,#39485,#39486,#39487,#39488,#39489,#39490,
#39491,#39492,#39493,#39494,#39495,#39496,#39497,#39498,#39499,#39500,#39501,
#39502,#39503,#39504,#39505,#39506,#39507,#39508,#39509,#39510,#39511,#39512,
#39513,#39514,#39515,#39516,#39517,#39518,#39519,#39520,#39521,#39522,#39523,
#39524,#39525,#39526,#39527,#39528,#39529,#39530),.UNSPECIFIED.,.F.,.F.)
B_SPLINE_CURVE_WITH_KNOTS((6,1,1,1,1,1,1,1,1,1,1,1,1,1,1,1,1,1,1,1,1,1,
1,1,1,1,1,1,1,1,1,1,1,1,1,1,1,1,1,1,1,1,1,1,1,1,1,1,1,1,1,1,1,1,1,1,1,1,
1,1,1,1,1,1,1,6),(-0.994228156739689,-0.984615384615383,-0.969230769230768,
-0.953846153846152,-0.938461538461537,-0.923076923076922,-0.907692307692306,
-0.892307692307691,-0.876923076923076,-0.86153846153846,-0.846153846153845,
-0.83076923076923,-0.815384615384614,-0.799999999999999,-0.784615384615384,
-0.769230769230768,-0.753846153846153,-0.738461538461538,-0.723076923076922,
-0.707692307692307,-0.692307692307692,-0.676923076923076,-0.661538461538461,
-0.646153846153846,-0.63076923076923,-0.615384615384615,-0.6,-0.584615384615384,
-0.569230769230769,-0.553846153846154,-0.538461538461538,-0.523076923076923,
-0.507692307692308,-0.492307692307692,-0.476923076923077,-0.461538461538462,
-0.446153846153846,-0.430769230769231,-0.415384615384615,-0.4,-0.384615384615385,
-0.369230769230769,-0.353846153846154,-0.338461538461538,-0.323076923076923,
-0.307692307692308,-0.292307692307692,-0.276923076923077,-0.261538461538462,
-0.246153846153846,-0.230769230769231,-0.215384615384615,-0.2,-0.184615384615385,
-0.169230769230769,-0.153846153846154,-0.138461538461538,-0.123076923076923,
-0.107692307692308,-0.0923076923076923,-0.0769230769230769,-0.0615384615384615,
-0.0461538461538462,-0.0307692307692308,-0.0153846153846154,0.),
 .UNSPECIFIED.)
CURVE()
GEOMETRIC_REPRESENTATION_ITEM()
RATIONAL_B_SPLINE_CURVE((1.,1.,1.,1.,1.,1.,1.,1.,1.,1.,1.,1.,1.,1.,1.,1.,
1.,1.,1.,1.,1.,1.,1.,1.,1.,1.,1.,1.,1.,1.,1.,1.,1.,1.,1.,1.,1.,1.,1.,1.,
1.,1.,1.,1.,1.,1.,1.,1.,1.,1.,1.,1.,1.,1.,1.,1.,1.,1.,1.,1.,1.,1.,1.,1.,
1.,1.,1.,1.,1.,1.))
REPRESENTATION_ITEM('')
);
#307=(
BOUNDED_CURVE()
B_SPLINE_CURVE(5,(#39683,#39684,#39685,#39686,#39687,#39688,#39689,#39690,
#39691,#39692,#39693,#39694,#39695,#39696,#39697,#39698,#39699,#39700,#39701,
#39702,#39703,#39704,#39705,#39706,#39707,#39708,#39709,#39710,#39711,#39712,
#39713,#39714,#39715,#39716,#39717,#39718,#39719,#39720,#39721,#39722,#39723,
#39724,#39725,#39726,#39727,#39728,#39729,#39730,#39731,#39732,#39733,#39734,
#39735,#39736,#39737,#39738,#39739,#39740,#39741,#39742,#39743,#39744,#39745,
#39746,#39747,#39748,#39749,#39750,#39751,#39752),.UNSPECIFIED.,.F.,.F.)
B_SPLINE_CURVE_WITH_KNOTS((6,1,1,1,1,1,1,1,1,1,1,1,1,1,1,1,1,1,1,1,1,1,
1,1,1,1,1,1,1,1,1,1,1,1,1,1,1,1,1,1,1,1,1,1,1,1,1,1,1,1,1,1,1,1,1,1,1,1,
1,1,1,1,1,1,1,6),(-1.,-0.984615384615383,-0.969230769230768,-0.953846153846152,
-0.938461538461537,-0.923076923076922,-0.907692307692306,-0.892307692307691,
-0.876923076923076,-0.86153846153846,-0.846153846153845,-0.83076923076923,
-0.815384615384614,-0.799999999999999,-0.784615384615384,-0.769230769230768,
-0.753846153846153,-0.738461538461538,-0.723076923076922,-0.707692307692307,
-0.692307692307692,-0.676923076923076,-0.661538461538461,-0.646153846153846,
-0.63076923076923,-0.615384615384615,-0.6,-0.584615384615384,-0.569230769230769,
-0.553846153846154,-0.538461538461538,-0.523076923076923,-0.507692307692308,
-0.492307692307692,-0.476923076923077,-0.461538461538462,-0.446153846153846,
-0.430769230769231,-0.415384615384615,-0.4,-0.384615384615385,-0.369230769230769,
-0.353846153846154,-0.338461538461538,-0.323076923076923,-0.307692307692308,
-0.292307692307692,-0.276923076923077,-0.261538461538462,-0.246153846153846,
-0.230769230769231,-0.215384615384615,-0.2,-0.184615384615385,-0.169230769230769,
-0.153846153846154,-0.138461538461538,-0.123076923076923,-0.107692307692308,
-0.0923076923076923,-0.0769230769230769,-0.0615384615384615,-0.0461538461538462,
-0.0307692307692308,-0.0153846153846154,-0.00577184337451766),
 .UNSPECIFIED.)
CURVE()
GEOMETRIC_REPRESENTATION_ITEM()
RATIONAL_B_SPLINE_CURVE((1.,1.,1.,1.,1.,1.,1.,1.,1.,1.,1.,1.,1.,1.,1.,1.,
1.,1.,1.,1.,1.,1.,1.,1.,1.,1.,1.,1.,1.,1.,1.,1.,1.,1.,1.,1.,1.,1.,1.,1.,
1.,1.,1.,1.,1.,1.,1.,1.,1.,1.,1.,1.,1.,1.,1.,1.,1.,1.,1.,1.,1.,1.,1.,1.,
1.,1.,1.,1.,1.,1.))
REPRESENTATION_ITEM('')
);
#308=(
BOUNDED_CURVE()
B_SPLINE_CURVE(5,(#39903,#39904,#39905,#39906,#39907,#39908,#39909,#39910,
#39911,#39912,#39913,#39914,#39915,#39916,#39917,#39918,#39919,#39920,#39921,
#39922,#39923,#39924,#39925,#39926,#39927,#39928,#39929,#39930,#39931,#39932,
#39933,#39934,#39935,#39936,#39937,#39938,#39939,#39940,#39941,#39942,#39943,
#39944,#39945,#39946,#39947,#39948,#39949,#39950,#39951,#39952,#39953,#39954,
#39955,#39956,#39957,#39958,#39959,#39960,#39961,#39962,#39963,#39964,#39965,
#39966,#39967,#39968,#39969,#39970,#39971,#39972),.UNSPECIFIED.,.F.,.F.)
B_SPLINE_CURVE_WITH_KNOTS((6,1,1,1,1,1,1,1,1,1,1,1,1,1,1,1,1,1,1,1,1,1,
1,1,1,1,1,1,1,1,1,1,1,1,1,1,1,1,1,1,1,1,1,1,1,1,1,1,1,1,1,1,1,1,1,1,1,1,
1,1,1,1,1,1,1,6),(-0.994228156739687,-0.984615384615383,-0.969230769230768,
-0.953846153846152,-0.938461538461537,-0.923076923076922,-0.907692307692306,
-0.892307692307691,-0.876923076923076,-0.86153846153846,-0.846153846153845,
-0.83076923076923,-0.815384615384614,-0.799999999999999,-0.784615384615384,
-0.769230769230768,-0.753846153846153,-0.738461538461538,-0.723076923076922,
-0.707692307692307,-0.692307692307692,-0.676923076923076,-0.661538461538461,
-0.646153846153846,-0.63076923076923,-0.615384615384615,-0.6,-0.584615384615384,
-0.569230769230769,-0.553846153846154,-0.538461538461538,-0.523076923076923,
-0.507692307692308,-0.492307692307692,-0.476923076923077,-0.461538461538462,
-0.446153846153846,-0.430769230769231,-0.415384615384615,-0.4,-0.384615384615385,
-0.369230769230769,-0.353846153846154,-0.338461538461538,-0.323076923076923,
-0.307692307692308,-0.292307692307692,-0.276923076923077,-0.261538461538462,
-0.246153846153846,-0.230769230769231,-0.215384615384615,-0.2,-0.184615384615385,
-0.169230769230769,-0.153846153846154,-0.138461538461538,-0.123076923076923,
-0.107692307692308,-0.0923076923076923,-0.0769230769230769,-0.0615384615384615,
-0.0461538461538462,-0.0307692307692308,-0.0153846153846154,0.),
 .UNSPECIFIED.)
CURVE()
GEOMETRIC_REPRESENTATION_ITEM()
RATIONAL_B_SPLINE_CURVE((1.,1.,1.,1.,1.,1.,1.,1.,1.,1.,1.,1.,1.,1.,1.,1.,
1.,1.,1.,1.,1.,1.,1.,1.,1.,1.,1.,1.,1.,1.,1.,1.,1.,1.,1.,1.,1.,1.,1.,1.,
1.,1.,1.,1.,1.,1.,1.,1.,1.,1.,1.,1.,1.,1.,1.,1.,1.,1.,1.,1.,1.,1.,1.,1.,
1.,1.,1.,1.,1.,1.))
REPRESENTATION_ITEM('')
);
#309=(
BOUNDED_CURVE()
B_SPLINE_CURVE(5,(#40125,#40126,#40127,#40128,#40129,#40130,#40131,#40132,
#40133,#40134,#40135,#40136,#40137,#40138,#40139,#40140,#40141,#40142,#40143,
#40144,#40145,#40146,#40147,#40148,#40149,#40150,#40151,#40152,#40153,#40154,
#40155,#40156,#40157,#40158,#40159,#40160,#40161,#40162,#40163,#40164,#40165,
#40166,#40167,#40168,#40169,#40170,#40171,#40172,#40173,#40174,#40175,#40176,
#40177,#40178,#40179,#40180,#40181,#40182,#40183,#40184,#40185,#40186,#40187,
#40188,#40189,#40190,#40191,#40192,#40193,#40194),.UNSPECIFIED.,.F.,.F.)
B_SPLINE_CURVE_WITH_KNOTS((6,1,1,1,1,1,1,1,1,1,1,1,1,1,1,1,1,1,1,1,1,1,
1,1,1,1,1,1,1,1,1,1,1,1,1,1,1,1,1,1,1,1,1,1,1,1,1,1,1,1,1,1,1,1,1,1,1,1,
1,1,1,1,1,1,1,6),(-1.,-0.984615384615383,-0.969230769230768,-0.953846153846152,
-0.938461538461537,-0.923076923076922,-0.907692307692306,-0.892307692307691,
-0.876923076923076,-0.86153846153846,-0.846153846153845,-0.83076923076923,
-0.815384615384614,-0.799999999999999,-0.784615384615384,-0.769230769230768,
-0.753846153846153,-0.738461538461538,-0.723076923076922,-0.707692307692307,
-0.692307692307692,-0.676923076923076,-0.661538461538461,-0.646153846153846,
-0.63076923076923,-0.615384615384615,-0.6,-0.584615384615384,-0.569230769230769,
-0.553846153846154,-0.538461538461538,-0.523076923076923,-0.507692307692308,
-0.492307692307692,-0.476923076923077,-0.461538461538462,-0.446153846153846,
-0.430769230769231,-0.415384615384615,-0.4,-0.384615384615385,-0.369230769230769,
-0.353846153846154,-0.338461538461538,-0.323076923076923,-0.307692307692308,
-0.292307692307692,-0.276923076923077,-0.261538461538462,-0.246153846153846,
-0.230769230769231,-0.215384615384615,-0.2,-0.184615384615385,-0.169230769230769,
-0.153846153846154,-0.138461538461538,-0.123076923076923,-0.107692307692308,
-0.0923076923076923,-0.0769230769230769,-0.0615384615384615,-0.0461538461538462,
-0.0307692307692308,-0.0153846153846154,-0.00577184337452512),
 .UNSPECIFIED.)
CURVE()
GEOMETRIC_REPRESENTATION_ITEM()
RATIONAL_B_SPLINE_CURVE((1.,1.,1.,1.,1.,1.,1.,1.,1.,1.,1.,1.,1.,1.,1.,1.,
1.,1.,1.,1.,1.,1.,1.,1.,1.,1.,1.,1.,1.,1.,1.,1.,1.,1.,1.,1.,1.,1.,1.,1.,
1.,1.,1.,1.,1.,1.,1.,1.,1.,1.,1.,1.,1.,1.,1.,1.,1.,1.,1.,1.,1.,1.,1.,1.,
1.,1.,1.,1.,1.,1.))
REPRESENTATION_ITEM('')
);
#310=(
BOUNDED_CURVE()
B_SPLINE_CURVE(5,(#40345,#40346,#40347,#40348,#40349,#40350,#40351,#40352,
#40353,#40354,#40355,#40356,#40357,#40358,#40359,#40360,#40361,#40362,#40363,
#40364,#40365,#40366,#40367,#40368,#40369,#40370,#40371,#40372,#40373,#40374,
#40375,#40376,#40377,#40378,#40379,#40380,#40381,#40382,#40383,#40384,#40385,
#40386,#40387,#40388,#40389,#40390,#40391,#40392,#40393,#40394,#40395,#40396,
#40397,#40398,#40399,#40400,#40401,#40402,#40403,#40404,#40405,#40406,#40407,
#40408,#40409,#40410,#40411,#40412,#40413,#40414),.UNSPECIFIED.,.F.,.F.)
B_SPLINE_CURVE_WITH_KNOTS((6,1,1,1,1,1,1,1,1,1,1,1,1,1,1,1,1,1,1,1,1,1,
1,1,1,1,1,1,1,1,1,1,1,1,1,1,1,1,1,1,1,1,1,1,1,1,1,1,1,1,1,1,1,1,1,1,1,1,
1,1,1,1,1,1,1,6),(-0.994228156739691,-0.984615384615383,-0.969230769230768,
-0.953846153846152,-0.938461538461537,-0.923076923076922,-0.907692307692306,
-0.892307692307691,-0.876923076923076,-0.86153846153846,-0.846153846153845,
-0.83076923076923,-0.815384615384614,-0.799999999999999,-0.784615384615384,
-0.769230769230768,-0.753846153846153,-0.738461538461538,-0.723076923076922,
-0.707692307692307,-0.692307692307692,-0.676923076923076,-0.661538461538461,
-0.646153846153846,-0.63076923076923,-0.615384615384615,-0.6,-0.584615384615384,
-0.569230769230769,-0.553846153846154,-0.538461538461538,-0.523076923076923,
-0.507692307692308,-0.492307692307692,-0.476923076923077,-0.461538461538462,
-0.446153846153846,-0.430769230769231,-0.415384615384615,-0.4,-0.384615384615385,
-0.369230769230769,-0.353846153846154,-0.338461538461538,-0.323076923076923,
-0.307692307692308,-0.292307692307692,-0.276923076923077,-0.261538461538462,
-0.246153846153846,-0.230769230769231,-0.215384615384615,-0.2,-0.184615384615385,
-0.169230769230769,-0.153846153846154,-0.138461538461538,-0.123076923076923,
-0.107692307692308,-0.0923076923076923,-0.0769230769230769,-0.0615384615384615,
-0.0461538461538462,-0.0307692307692308,-0.0153846153846154,0.),
 .UNSPECIFIED.)
CURVE()
GEOMETRIC_REPRESENTATION_ITEM()
RATIONAL_B_SPLINE_CURVE((1.,1.,1.,1.,1.,1.,1.,1.,1.,1.,1.,1.,1.,1.,1.,1.,
1.,1.,1.,1.,1.,1.,1.,1.,1.,1.,1.,1.,1.,1.,1.,1.,1.,1.,1.,1.,1.,1.,1.,1.,
1.,1.,1.,1.,1.,1.,1.,1.,1.,1.,1.,1.,1.,1.,1.,1.,1.,1.,1.,1.,1.,1.,1.,1.,
1.,1.,1.,1.,1.,1.))
REPRESENTATION_ITEM('')
);
#311=(
BOUNDED_CURVE()
B_SPLINE_CURVE(5,(#40567,#40568,#40569,#40570,#40571,#40572,#40573,#40574,
#40575,#40576,#40577,#40578,#40579,#40580,#40581,#40582,#40583,#40584,#40585,
#40586,#40587,#40588,#40589,#40590,#40591,#40592,#40593,#40594,#40595,#40596,
#40597,#40598,#40599,#40600,#40601,#40602,#40603,#40604,#40605,#40606,#40607,
#40608,#40609,#40610,#40611,#40612,#40613,#40614,#40615,#40616,#40617,#40618,
#40619,#40620,#40621,#40622,#40623,#40624,#40625,#40626,#40627,#40628,#40629,
#40630,#40631,#40632,#40633,#40634,#40635,#40636),.UNSPECIFIED.,.F.,.F.)
B_SPLINE_CURVE_WITH_KNOTS((6,1,1,1,1,1,1,1,1,1,1,1,1,1,1,1,1,1,1,1,1,1,
1,1,1,1,1,1,1,1,1,1,1,1,1,1,1,1,1,1,1,1,1,1,1,1,1,1,1,1,1,1,1,1,1,1,1,1,
1,1,1,1,1,1,1,6),(-1.,-0.984615384615383,-0.969230769230768,-0.953846153846152,
-0.938461538461537,-0.923076923076922,-0.907692307692306,-0.892307692307691,
-0.876923076923076,-0.86153846153846,-0.846153846153845,-0.83076923076923,
-0.815384615384614,-0.799999999999999,-0.784615384615384,-0.769230769230768,
-0.753846153846153,-0.738461538461538,-0.723076923076922,-0.707692307692307,
-0.692307692307692,-0.676923076923076,-0.661538461538461,-0.646153846153846,
-0.63076923076923,-0.615384615384615,-0.6,-0.584615384615384,-0.569230769230769,
-0.553846153846154,-0.538461538461538,-0.523076923076923,-0.507692307692308,
-0.492307692307692,-0.476923076923077,-0.461538461538462,-0.446153846153846,
-0.430769230769231,-0.415384615384615,-0.4,-0.384615384615385,-0.369230769230769,
-0.353846153846154,-0.338461538461538,-0.323076923076923,-0.307692307692308,
-0.292307692307692,-0.276923076923077,-0.261538461538462,-0.246153846153846,
-0.230769230769231,-0.215384615384615,-0.2,-0.184615384615385,-0.169230769230769,
-0.153846153846154,-0.138461538461538,-0.123076923076923,-0.107692307692308,
-0.0923076923076923,-0.0769230769230769,-0.0615384615384615,-0.0461538461538462,
-0.0307692307692308,-0.0153846153846154,-0.00577184337448448),
 .UNSPECIFIED.)
CURVE()
GEOMETRIC_REPRESENTATION_ITEM()
RATIONAL_B_SPLINE_CURVE((1.,1.,1.,1.,1.,1.,1.,1.,1.,1.,1.,1.,1.,1.,1.,1.,
1.,1.,1.,1.,1.,1.,1.,1.,1.,1.,1.,1.,1.,1.,1.,1.,1.,1.,1.,1.,1.,1.,1.,1.,
1.,1.,1.,1.,1.,1.,1.,1.,1.,1.,1.,1.,1.,1.,1.,1.,1.,1.,1.,1.,1.,1.,1.,1.,
1.,1.,1.,1.,1.,1.))
REPRESENTATION_ITEM('')
);
#312=(
BOUNDED_CURVE()
B_SPLINE_CURVE(5,(#40787,#40788,#40789,#40790,#40791,#40792,#40793,#40794,
#40795,#40796,#40797,#40798,#40799,#40800,#40801,#40802,#40803,#40804,#40805,
#40806,#40807,#40808,#40809,#40810,#40811,#40812,#40813,#40814,#40815,#40816,
#40817,#40818,#40819,#40820,#40821,#40822,#40823,#40824,#40825,#40826,#40827,
#40828,#40829,#40830,#40831,#40832,#40833,#40834,#40835,#40836,#40837,#40838,
#40839,#40840,#40841,#40842,#40843,#40844,#40845,#40846,#40847,#40848,#40849,
#40850,#40851,#40852,#40853,#40854,#40855,#40856),.UNSPECIFIED.,.F.,.F.)
B_SPLINE_CURVE_WITH_KNOTS((6,1,1,1,1,1,1,1,1,1,1,1,1,1,1,1,1,1,1,1,1,1,
1,1,1,1,1,1,1,1,1,1,1,1,1,1,1,1,1,1,1,1,1,1,1,1,1,1,1,1,1,1,1,1,1,1,1,1,
1,1,1,1,1,1,1,6),(-0.99422815673972,-0.984615384615383,-0.969230769230768,
-0.953846153846152,-0.938461538461537,-0.923076923076922,-0.907692307692306,
-0.892307692307691,-0.876923076923076,-0.86153846153846,-0.846153846153845,
-0.83076923076923,-0.815384615384614,-0.799999999999999,-0.784615384615384,
-0.769230769230768,-0.753846153846153,-0.738461538461538,-0.723076923076922,
-0.707692307692307,-0.692307692307692,-0.676923076923076,-0.661538461538461,
-0.646153846153846,-0.63076923076923,-0.615384615384615,-0.6,-0.584615384615384,
-0.569230769230769,-0.553846153846154,-0.538461538461538,-0.523076923076923,
-0.507692307692308,-0.492307692307692,-0.476923076923077,-0.461538461538462,
-0.446153846153846,-0.430769230769231,-0.415384615384615,-0.4,-0.384615384615385,
-0.369230769230769,-0.353846153846154,-0.338461538461538,-0.323076923076923,
-0.307692307692308,-0.292307692307692,-0.276923076923077,-0.261538461538462,
-0.246153846153846,-0.230769230769231,-0.215384615384615,-0.2,-0.184615384615385,
-0.169230769230769,-0.153846153846154,-0.138461538461538,-0.123076923076923,
-0.107692307692308,-0.0923076923076923,-0.0769230769230769,-0.0615384615384615,
-0.0461538461538462,-0.0307692307692308,-0.0153846153846154,0.),
 .UNSPECIFIED.)
CURVE()
GEOMETRIC_REPRESENTATION_ITEM()
RATIONAL_B_SPLINE_CURVE((1.,1.,1.,1.,1.,1.,1.,1.,1.,1.,1.,1.,1.,1.,1.,1.,
1.,1.,1.,1.,1.,1.,1.,1.,1.,1.,1.,1.,1.,1.,1.,1.,1.,1.,1.,1.,1.,1.,1.,1.,
1.,1.,1.,1.,1.,1.,1.,1.,1.,1.,1.,1.,1.,1.,1.,1.,1.,1.,1.,1.,1.,1.,1.,1.,
1.,1.,1.,1.,1.,1.))
REPRESENTATION_ITEM('')
);
#313=(
BOUNDED_CURVE()
B_SPLINE_CURVE(5,(#41009,#41010,#41011,#41012,#41013,#41014,#41015,#41016,
#41017,#41018,#41019,#41020,#41021,#41022,#41023,#41024,#41025,#41026,#41027,
#41028,#41029,#41030,#41031,#41032,#41033,#41034,#41035,#41036,#41037,#41038,
#41039,#41040,#41041,#41042,#41043,#41044,#41045,#41046,#41047,#41048,#41049,
#41050,#41051,#41052,#41053,#41054,#41055,#41056,#41057,#41058,#41059,#41060,
#41061,#41062,#41063,#41064,#41065,#41066,#41067,#41068,#41069,#41070,#41071,
#41072,#41073,#41074,#41075,#41076,#41077,#41078),.UNSPECIFIED.,.F.,.F.)
B_SPLINE_CURVE_WITH_KNOTS((6,1,1,1,1,1,1,1,1,1,1,1,1,1,1,1,1,1,1,1,1,1,
1,1,1,1,1,1,1,1,1,1,1,1,1,1,1,1,1,1,1,1,1,1,1,1,1,1,1,1,1,1,1,1,1,1,1,1,
1,1,1,1,1,1,1,6),(-1.,-0.984615384615383,-0.969230769230768,-0.953846153846152,
-0.938461538461537,-0.923076923076922,-0.907692307692306,-0.892307692307691,
-0.876923076923076,-0.86153846153846,-0.846153846153845,-0.83076923076923,
-0.815384615384614,-0.799999999999999,-0.784615384615384,-0.769230769230768,
-0.753846153846153,-0.738461538461538,-0.723076923076922,-0.707692307692307,
-0.692307692307692,-0.676923076923076,-0.661538461538461,-0.646153846153846,
-0.63076923076923,-0.615384615384615,-0.6,-0.584615384615384,-0.569230769230769,
-0.553846153846154,-0.538461538461538,-0.523076923076923,-0.507692307692308,
-0.492307692307692,-0.476923076923077,-0.461538461538462,-0.446153846153846,
-0.430769230769231,-0.415384615384615,-0.4,-0.384615384615385,-0.369230769230769,
-0.353846153846154,-0.338461538461538,-0.323076923076923,-0.307692307692308,
-0.292307692307692,-0.276923076923077,-0.261538461538462,-0.246153846153846,
-0.230769230769231,-0.215384615384615,-0.2,-0.184615384615385,-0.169230769230769,
-0.153846153846154,-0.138461538461538,-0.123076923076923,-0.107692307692308,
-0.0923076923076923,-0.0769230769230769,-0.0615384615384615,-0.0461538461538462,
-0.0307692307692308,-0.0153846153846154,-0.00577184337448251),
 .UNSPECIFIED.)
CURVE()
GEOMETRIC_REPRESENTATION_ITEM()
RATIONAL_B_SPLINE_CURVE((1.,1.,1.,1.,1.,1.,1.,1.,1.,1.,1.,1.,1.,1.,1.,1.,
1.,1.,1.,1.,1.,1.,1.,1.,1.,1.,1.,1.,1.,1.,1.,1.,1.,1.,1.,1.,1.,1.,1.,1.,
1.,1.,1.,1.,1.,1.,1.,1.,1.,1.,1.,1.,1.,1.,1.,1.,1.,1.,1.,1.,1.,1.,1.,1.,
1.,1.,1.,1.,1.,1.))
REPRESENTATION_ITEM('')
);
#314=(
BOUNDED_CURVE()
B_SPLINE_CURVE(5,(#41229,#41230,#41231,#41232,#41233,#41234,#41235,#41236,
#41237,#41238,#41239,#41240,#41241,#41242,#41243,#41244,#41245,#41246,#41247,
#41248,#41249,#41250,#41251,#41252,#41253,#41254,#41255,#41256,#41257,#41258,
#41259,#41260,#41261,#41262,#41263,#41264,#41265,#41266,#41267,#41268,#41269,
#41270,#41271,#41272,#41273,#41274,#41275,#41276,#41277,#41278,#41279,#41280,
#41281,#41282,#41283,#41284,#41285,#41286,#41287,#41288,#41289,#41290,#41291,
#41292,#41293,#41294,#41295,#41296,#41297,#41298),.UNSPECIFIED.,.F.,.F.)
B_SPLINE_CURVE_WITH_KNOTS((6,1,1,1,1,1,1,1,1,1,1,1,1,1,1,1,1,1,1,1,1,1,
1,1,1,1,1,1,1,1,1,1,1,1,1,1,1,1,1,1,1,1,1,1,1,1,1,1,1,1,1,1,1,1,1,1,1,1,
1,1,1,1,1,1,1,6),(-0.994228156739703,-0.984615384615383,-0.969230769230768,
-0.953846153846152,-0.938461538461537,-0.923076923076922,-0.907692307692306,
-0.892307692307691,-0.876923076923076,-0.86153846153846,-0.846153846153845,
-0.83076923076923,-0.815384615384614,-0.799999999999999,-0.784615384615384,
-0.769230769230768,-0.753846153846153,-0.738461538461538,-0.723076923076922,
-0.707692307692307,-0.692307692307692,-0.676923076923076,-0.661538461538461,
-0.646153846153846,-0.63076923076923,-0.615384615384615,-0.6,-0.584615384615384,
-0.569230769230769,-0.553846153846154,-0.538461538461538,-0.523076923076923,
-0.507692307692308,-0.492307692307692,-0.476923076923077,-0.461538461538462,
-0.446153846153846,-0.430769230769231,-0.415384615384615,-0.4,-0.384615384615385,
-0.369230769230769,-0.353846153846154,-0.338461538461538,-0.323076923076923,
-0.307692307692308,-0.292307692307692,-0.276923076923077,-0.261538461538462,
-0.246153846153846,-0.230769230769231,-0.215384615384615,-0.2,-0.184615384615385,
-0.169230769230769,-0.153846153846154,-0.138461538461538,-0.123076923076923,
-0.107692307692308,-0.0923076923076923,-0.0769230769230769,-0.0615384615384615,
-0.0461538461538462,-0.0307692307692308,-0.0153846153846154,0.),
 .UNSPECIFIED.)
CURVE()
GEOMETRIC_REPRESENTATION_ITEM()
RATIONAL_B_SPLINE_CURVE((1.,1.,1.,1.,1.,1.,1.,1.,1.,1.,1.,1.,1.,1.,1.,1.,
1.,1.,1.,1.,1.,1.,1.,1.,1.,1.,1.,1.,1.,1.,1.,1.,1.,1.,1.,1.,1.,1.,1.,1.,
1.,1.,1.,1.,1.,1.,1.,1.,1.,1.,1.,1.,1.,1.,1.,1.,1.,1.,1.,1.,1.,1.,1.,1.,
1.,1.,1.,1.,1.,1.))
REPRESENTATION_ITEM('')
);
#315=(
BOUNDED_CURVE()
B_SPLINE_CURVE(5,(#41451,#41452,#41453,#41454,#41455,#41456,#41457,#41458,
#41459,#41460,#41461,#41462,#41463,#41464,#41465,#41466,#41467,#41468,#41469,
#41470,#41471,#41472,#41473,#41474,#41475,#41476,#41477,#41478,#41479,#41480,
#41481,#41482,#41483,#41484,#41485,#41486,#41487,#41488,#41489,#41490,#41491,
#41492,#41493,#41494,#41495,#41496,#41497,#41498,#41499,#41500,#41501,#41502,
#41503,#41504,#41505,#41506,#41507,#41508,#41509,#41510,#41511,#41512,#41513,
#41514,#41515,#41516,#41517,#41518,#41519,#41520),.UNSPECIFIED.,.F.,.F.)
B_SPLINE_CURVE_WITH_KNOTS((6,1,1,1,1,1,1,1,1,1,1,1,1,1,1,1,1,1,1,1,1,1,
1,1,1,1,1,1,1,1,1,1,1,1,1,1,1,1,1,1,1,1,1,1,1,1,1,1,1,1,1,1,1,1,1,1,1,1,
1,1,1,1,1,1,1,6),(-1.,-0.984615384615383,-0.969230769230768,-0.953846153846152,
-0.938461538461537,-0.923076923076922,-0.907692307692306,-0.892307692307691,
-0.876923076923076,-0.86153846153846,-0.846153846153845,-0.83076923076923,
-0.815384615384614,-0.799999999999999,-0.784615384615384,-0.769230769230768,
-0.753846153846153,-0.738461538461538,-0.723076923076922,-0.707692307692307,
-0.692307692307692,-0.676923076923076,-0.661538461538461,-0.646153846153846,
-0.63076923076923,-0.615384615384615,-0.6,-0.584615384615384,-0.569230769230769,
-0.553846153846154,-0.538461538461538,-0.523076923076923,-0.507692307692308,
-0.492307692307692,-0.476923076923077,-0.461538461538462,-0.446153846153846,
-0.430769230769231,-0.415384615384615,-0.4,-0.384615384615385,-0.369230769230769,
-0.353846153846154,-0.338461538461538,-0.323076923076923,-0.307692307692308,
-0.292307692307692,-0.276923076923077,-0.261538461538462,-0.246153846153846,
-0.230769230769231,-0.215384615384615,-0.2,-0.184615384615385,-0.169230769230769,
-0.153846153846154,-0.138461538461538,-0.123076923076923,-0.107692307692308,
-0.0923076923076923,-0.0769230769230769,-0.0615384615384615,-0.0461538461538462,
-0.0307692307692308,-0.0153846153846154,-0.00577184337449602),
 .UNSPECIFIED.)
CURVE()
GEOMETRIC_REPRESENTATION_ITEM()
RATIONAL_B_SPLINE_CURVE((1.,1.,1.,1.,1.,1.,1.,1.,1.,1.,1.,1.,1.,1.,1.,1.,
1.,1.,1.,1.,1.,1.,1.,1.,1.,1.,1.,1.,1.,1.,1.,1.,1.,1.,1.,1.,1.,1.,1.,1.,
1.,1.,1.,1.,1.,1.,1.,1.,1.,1.,1.,1.,1.,1.,1.,1.,1.,1.,1.,1.,1.,1.,1.,1.,
1.,1.,1.,1.,1.,1.))
REPRESENTATION_ITEM('')
);
#316=(
BOUNDED_CURVE()
B_SPLINE_CURVE(5,(#41671,#41672,#41673,#41674,#41675,#41676,#41677,#41678,
#41679,#41680,#41681,#41682,#41683,#41684,#41685,#41686,#41687,#41688,#41689,
#41690,#41691,#41692,#41693,#41694,#41695,#41696,#41697,#41698,#41699,#41700,
#41701,#41702,#41703,#41704,#41705,#41706,#41707,#41708,#41709,#41710,#41711,
#41712,#41713,#41714,#41715,#41716,#41717,#41718,#41719,#41720,#41721,#41722,
#41723,#41724,#41725,#41726,#41727,#41728,#41729,#41730,#41731,#41732,#41733,
#41734,#41735,#41736,#41737,#41738,#41739,#41740),.UNSPECIFIED.,.F.,.F.)
B_SPLINE_CURVE_WITH_KNOTS((6,1,1,1,1,1,1,1,1,1,1,1,1,1,1,1,1,1,1,1,1,1,
1,1,1,1,1,1,1,1,1,1,1,1,1,1,1,1,1,1,1,1,1,1,1,1,1,1,1,1,1,1,1,1,1,1,1,1,
1,1,1,1,1,1,1,6),(-0.994228156739695,-0.984615384615383,-0.969230769230768,
-0.953846153846152,-0.938461538461537,-0.923076923076922,-0.907692307692306,
-0.892307692307691,-0.876923076923076,-0.86153846153846,-0.846153846153845,
-0.83076923076923,-0.815384615384614,-0.799999999999999,-0.784615384615384,
-0.769230769230768,-0.753846153846153,-0.738461538461538,-0.723076923076922,
-0.707692307692307,-0.692307692307692,-0.676923076923076,-0.661538461538461,
-0.646153846153846,-0.63076923076923,-0.615384615384615,-0.6,-0.584615384615384,
-0.569230769230769,-0.553846153846154,-0.538461538461538,-0.523076923076923,
-0.507692307692308,-0.492307692307692,-0.476923076923077,-0.461538461538462,
-0.446153846153846,-0.430769230769231,-0.415384615384615,-0.4,-0.384615384615385,
-0.369230769230769,-0.353846153846154,-0.338461538461538,-0.323076923076923,
-0.307692307692308,-0.292307692307692,-0.276923076923077,-0.261538461538462,
-0.246153846153846,-0.230769230769231,-0.215384615384615,-0.2,-0.184615384615385,
-0.169230769230769,-0.153846153846154,-0.138461538461538,-0.123076923076923,
-0.107692307692308,-0.0923076923076923,-0.0769230769230769,-0.0615384615384615,
-0.0461538461538462,-0.0307692307692308,-0.0153846153846154,0.),
 .UNSPECIFIED.)
CURVE()
GEOMETRIC_REPRESENTATION_ITEM()
RATIONAL_B_SPLINE_CURVE((1.,1.,1.,1.,1.,1.,1.,1.,1.,1.,1.,1.,1.,1.,1.,1.,
1.,1.,1.,1.,1.,1.,1.,1.,1.,1.,1.,1.,1.,1.,1.,1.,1.,1.,1.,1.,1.,1.,1.,1.,
1.,1.,1.,1.,1.,1.,1.,1.,1.,1.,1.,1.,1.,1.,1.,1.,1.,1.,1.,1.,1.,1.,1.,1.,
1.,1.,1.,1.,1.,1.))
REPRESENTATION_ITEM('')
);
#317=(
BOUNDED_CURVE()
B_SPLINE_CURVE(5,(#41893,#41894,#41895,#41896,#41897,#41898,#41899,#41900,
#41901,#41902,#41903,#41904,#41905,#41906,#41907,#41908,#41909,#41910,#41911,
#41912,#41913,#41914,#41915,#41916,#41917,#41918,#41919,#41920,#41921,#41922,
#41923,#41924,#41925,#41926,#41927,#41928,#41929,#41930,#41931,#41932,#41933,
#41934,#41935,#41936,#41937,#41938,#41939,#41940,#41941,#41942,#41943,#41944,
#41945,#41946,#41947,#41948,#41949,#41950,#41951,#41952,#41953,#41954,#41955,
#41956,#41957,#41958,#41959,#41960,#41961,#41962),.UNSPECIFIED.,.F.,.F.)
B_SPLINE_CURVE_WITH_KNOTS((6,1,1,1,1,1,1,1,1,1,1,1,1,1,1,1,1,1,1,1,1,1,
1,1,1,1,1,1,1,1,1,1,1,1,1,1,1,1,1,1,1,1,1,1,1,1,1,1,1,1,1,1,1,1,1,1,1,1,
1,1,1,1,1,1,1,6),(-1.,-0.984615384615383,-0.969230769230768,-0.953846153846152,
-0.938461538461537,-0.923076923076922,-0.907692307692306,-0.892307692307691,
-0.876923076923076,-0.86153846153846,-0.846153846153845,-0.83076923076923,
-0.815384615384614,-0.799999999999999,-0.784615384615384,-0.769230769230768,
-0.753846153846153,-0.738461538461538,-0.723076923076922,-0.707692307692307,
-0.692307692307692,-0.676923076923076,-0.661538461538461,-0.646153846153846,
-0.63076923076923,-0.615384615384615,-0.6,-0.584615384615384,-0.569230769230769,
-0.553846153846154,-0.538461538461538,-0.523076923076923,-0.507692307692308,
-0.492307692307692,-0.476923076923077,-0.461538461538462,-0.446153846153846,
-0.430769230769231,-0.415384615384615,-0.4,-0.384615384615385,-0.369230769230769,
-0.353846153846154,-0.338461538461538,-0.323076923076923,-0.307692307692308,
-0.292307692307692,-0.276923076923077,-0.261538461538462,-0.246153846153846,
-0.230769230769231,-0.215384615384615,-0.2,-0.184615384615385,-0.169230769230769,
-0.153846153846154,-0.138461538461538,-0.123076923076923,-0.107692307692308,
-0.0923076923076923,-0.0769230769230769,-0.0615384615384615,-0.0461538461538462,
-0.0307692307692308,-0.0153846153846154,-0.00577184337450911),
 .UNSPECIFIED.)
CURVE()
GEOMETRIC_REPRESENTATION_ITEM()
RATIONAL_B_SPLINE_CURVE((1.,1.,1.,1.,1.,1.,1.,1.,1.,1.,1.,1.,1.,1.,1.,1.,
1.,1.,1.,1.,1.,1.,1.,1.,1.,1.,1.,1.,1.,1.,1.,1.,1.,1.,1.,1.,1.,1.,1.,1.,
1.,1.,1.,1.,1.,1.,1.,1.,1.,1.,1.,1.,1.,1.,1.,1.,1.,1.,1.,1.,1.,1.,1.,1.,
1.,1.,1.,1.,1.,1.))
REPRESENTATION_ITEM('')
);
#318=(
BOUNDED_CURVE()
B_SPLINE_CURVE(5,(#42113,#42114,#42115,#42116,#42117,#42118,#42119,#42120,
#42121,#42122,#42123,#42124,#42125,#42126,#42127,#42128,#42129,#42130,#42131,
#42132,#42133,#42134,#42135,#42136,#42137,#42138,#42139,#42140,#42141,#42142,
#42143,#42144,#42145,#42146,#42147,#42148,#42149,#42150,#42151,#42152,#42153,
#42154,#42155,#42156,#42157,#42158,#42159,#42160,#42161,#42162,#42163,#42164,
#42165,#42166,#42167,#42168,#42169,#42170,#42171,#42172,#42173,#42174,#42175,
#42176,#42177,#42178,#42179,#42180,#42181,#42182),.UNSPECIFIED.,.F.,.F.)
B_SPLINE_CURVE_WITH_KNOTS((6,1,1,1,1,1,1,1,1,1,1,1,1,1,1,1,1,1,1,1,1,1,
1,1,1,1,1,1,1,1,1,1,1,1,1,1,1,1,1,1,1,1,1,1,1,1,1,1,1,1,1,1,1,1,1,1,1,1,
1,1,1,1,1,1,1,6),(-0.994228156739712,-0.984615384615383,-0.969230769230768,
-0.953846153846152,-0.938461538461537,-0.923076923076922,-0.907692307692306,
-0.892307692307691,-0.876923076923076,-0.86153846153846,-0.846153846153845,
-0.83076923076923,-0.815384615384614,-0.799999999999999,-0.784615384615384,
-0.769230769230768,-0.753846153846153,-0.738461538461538,-0.723076923076922,
-0.707692307692307,-0.692307692307692,-0.676923076923076,-0.661538461538461,
-0.646153846153846,-0.63076923076923,-0.615384615384615,-0.6,-0.584615384615384,
-0.569230769230769,-0.553846153846154,-0.538461538461538,-0.523076923076923,
-0.507692307692308,-0.492307692307692,-0.476923076923077,-0.461538461538462,
-0.446153846153846,-0.430769230769231,-0.415384615384615,-0.4,-0.384615384615385,
-0.369230769230769,-0.353846153846154,-0.338461538461538,-0.323076923076923,
-0.307692307692308,-0.292307692307692,-0.276923076923077,-0.261538461538462,
-0.246153846153846,-0.230769230769231,-0.215384615384615,-0.2,-0.184615384615385,
-0.169230769230769,-0.153846153846154,-0.138461538461538,-0.123076923076923,
-0.107692307692308,-0.0923076923076923,-0.0769230769230769,-0.0615384615384615,
-0.0461538461538462,-0.0307692307692308,-0.0153846153846154,0.),
 .UNSPECIFIED.)
CURVE()
GEOMETRIC_REPRESENTATION_ITEM()
RATIONAL_B_SPLINE_CURVE((1.,1.,1.,1.,1.,1.,1.,1.,1.,1.,1.,1.,1.,1.,1.,1.,
1.,1.,1.,1.,1.,1.,1.,1.,1.,1.,1.,1.,1.,1.,1.,1.,1.,1.,1.,1.,1.,1.,1.,1.,
1.,1.,1.,1.,1.,1.,1.,1.,1.,1.,1.,1.,1.,1.,1.,1.,1.,1.,1.,1.,1.,1.,1.,1.,
1.,1.,1.,1.,1.,1.))
REPRESENTATION_ITEM('')
);
#319=(
BOUNDED_CURVE()
B_SPLINE_CURVE(5,(#42335,#42336,#42337,#42338,#42339,#42340,#42341,#42342,
#42343,#42344,#42345,#42346,#42347,#42348,#42349,#42350,#42351,#42352,#42353,
#42354,#42355,#42356,#42357,#42358,#42359,#42360,#42361,#42362,#42363,#42364,
#42365,#42366,#42367,#42368,#42369,#42370,#42371,#42372,#42373,#42374,#42375,
#42376,#42377,#42378,#42379,#42380,#42381,#42382,#42383,#42384,#42385,#42386,
#42387,#42388,#42389,#42390,#42391,#42392,#42393,#42394,#42395,#42396,#42397,
#42398,#42399,#42400,#42401,#42402,#42403,#42404),.UNSPECIFIED.,.F.,.F.)
B_SPLINE_CURVE_WITH_KNOTS((6,1,1,1,1,1,1,1,1,1,1,1,1,1,1,1,1,1,1,1,1,1,
1,1,1,1,1,1,1,1,1,1,1,1,1,1,1,1,1,1,1,1,1,1,1,1,1,1,1,1,1,1,1,1,1,1,1,1,
1,1,1,1,1,1,1,6),(-1.,-0.984615384615383,-0.969230769230768,-0.953846153846152,
-0.938461538461537,-0.923076923076922,-0.907692307692306,-0.892307692307691,
-0.876923076923076,-0.86153846153846,-0.846153846153845,-0.83076923076923,
-0.815384615384614,-0.799999999999999,-0.784615384615384,-0.769230769230768,
-0.753846153846153,-0.738461538461538,-0.723076923076922,-0.707692307692307,
-0.692307692307692,-0.676923076923076,-0.661538461538461,-0.646153846153846,
-0.63076923076923,-0.615384615384615,-0.6,-0.584615384615384,-0.569230769230769,
-0.553846153846154,-0.538461538461538,-0.523076923076923,-0.507692307692308,
-0.492307692307692,-0.476923076923077,-0.461538461538462,-0.446153846153846,
-0.430769230769231,-0.415384615384615,-0.4,-0.384615384615385,-0.369230769230769,
-0.353846153846154,-0.338461538461538,-0.323076923076923,-0.307692307692308,
-0.292307692307692,-0.276923076923077,-0.261538461538462,-0.246153846153846,
-0.230769230769231,-0.215384615384615,-0.2,-0.184615384615385,-0.169230769230769,
-0.153846153846154,-0.138461538461538,-0.123076923076923,-0.107692307692308,
-0.0923076923076923,-0.0769230769230769,-0.0615384615384615,-0.0461538461538462,
-0.0307692307692308,-0.0153846153846154,-0.00577184337451206),
 .UNSPECIFIED.)
CURVE()
GEOMETRIC_REPRESENTATION_ITEM()
RATIONAL_B_SPLINE_CURVE((1.,1.,1.,1.,1.,1.,1.,1.,1.,1.,1.,1.,1.,1.,1.,1.,
1.,1.,1.,1.,1.,1.,1.,1.,1.,1.,1.,1.,1.,1.,1.,1.,1.,1.,1.,1.,1.,1.,1.,1.,
1.,1.,1.,1.,1.,1.,1.,1.,1.,1.,1.,1.,1.,1.,1.,1.,1.,1.,1.,1.,1.,1.,1.,1.,
1.,1.,1.,1.,1.,1.))
REPRESENTATION_ITEM('')
);
#320=(
BOUNDED_CURVE()
B_SPLINE_CURVE(5,(#42555,#42556,#42557,#42558,#42559,#42560,#42561,#42562,
#42563,#42564,#42565,#42566,#42567,#42568,#42569,#42570,#42571,#42572,#42573,
#42574,#42575,#42576,#42577,#42578,#42579,#42580,#42581,#42582,#42583,#42584,
#42585,#42586,#42587,#42588,#42589,#42590,#42591,#42592,#42593,#42594,#42595,
#42596,#42597,#42598,#42599,#42600,#42601,#42602,#42603,#42604,#42605,#42606,
#42607,#42608,#42609,#42610,#42611,#42612,#42613,#42614,#42615,#42616,#42617,
#42618,#42619,#42620,#42621,#42622,#42623,#42624),.UNSPECIFIED.,.F.,.F.)
B_SPLINE_CURVE_WITH_KNOTS((6,1,1,1,1,1,1,1,1,1,1,1,1,1,1,1,1,1,1,1,1,1,
1,1,1,1,1,1,1,1,1,1,1,1,1,1,1,1,1,1,1,1,1,1,1,1,1,1,1,1,1,1,1,1,1,1,1,1,
1,1,1,1,1,1,1,6),(-0.994228156739717,-0.984615384615383,-0.969230769230768,
-0.953846153846152,-0.938461538461537,-0.923076923076922,-0.907692307692306,
-0.892307692307691,-0.876923076923076,-0.86153846153846,-0.846153846153845,
-0.83076923076923,-0.815384615384614,-0.799999999999999,-0.784615384615384,
-0.769230769230768,-0.753846153846153,-0.738461538461538,-0.723076923076922,
-0.707692307692307,-0.692307692307692,-0.676923076923076,-0.661538461538461,
-0.646153846153846,-0.63076923076923,-0.615384615384615,-0.6,-0.584615384615384,
-0.569230769230769,-0.553846153846154,-0.538461538461538,-0.523076923076923,
-0.507692307692308,-0.492307692307692,-0.476923076923077,-0.461538461538462,
-0.446153846153846,-0.430769230769231,-0.415384615384615,-0.4,-0.384615384615385,
-0.369230769230769,-0.353846153846154,-0.338461538461538,-0.323076923076923,
-0.307692307692308,-0.292307692307692,-0.276923076923077,-0.261538461538462,
-0.246153846153846,-0.230769230769231,-0.215384615384615,-0.2,-0.184615384615385,
-0.169230769230769,-0.153846153846154,-0.138461538461538,-0.123076923076923,
-0.107692307692308,-0.0923076923076923,-0.0769230769230769,-0.0615384615384615,
-0.0461538461538462,-0.0307692307692308,-0.0153846153846154,0.),
 .UNSPECIFIED.)
CURVE()
GEOMETRIC_REPRESENTATION_ITEM()
RATIONAL_B_SPLINE_CURVE((1.,1.,1.,1.,1.,1.,1.,1.,1.,1.,1.,1.,1.,1.,1.,1.,
1.,1.,1.,1.,1.,1.,1.,1.,1.,1.,1.,1.,1.,1.,1.,1.,1.,1.,1.,1.,1.,1.,1.,1.,
1.,1.,1.,1.,1.,1.,1.,1.,1.,1.,1.,1.,1.,1.,1.,1.,1.,1.,1.,1.,1.,1.,1.,1.,
1.,1.,1.,1.,1.,1.))
REPRESENTATION_ITEM('')
);
#321=(
BOUNDED_CURVE()
B_SPLINE_CURVE(5,(#42777,#42778,#42779,#42780,#42781,#42782,#42783,#42784,
#42785,#42786,#42787,#42788,#42789,#42790,#42791,#42792,#42793,#42794,#42795,
#42796,#42797,#42798,#42799,#42800,#42801,#42802,#42803,#42804,#42805,#42806,
#42807,#42808,#42809,#42810,#42811,#42812,#42813,#42814,#42815,#42816,#42817,
#42818,#42819,#42820,#42821,#42822,#42823,#42824,#42825,#42826,#42827,#42828,
#42829,#42830,#42831,#42832,#42833,#42834,#42835,#42836,#42837,#42838,#42839,
#42840,#42841,#42842,#42843,#42844,#42845,#42846),.UNSPECIFIED.,.F.,.F.)
B_SPLINE_CURVE_WITH_KNOTS((6,1,1,1,1,1,1,1,1,1,1,1,1,1,1,1,1,1,1,1,1,1,
1,1,1,1,1,1,1,1,1,1,1,1,1,1,1,1,1,1,1,1,1,1,1,1,1,1,1,1,1,1,1,1,1,1,1,1,
1,1,1,1,1,1,1,6),(-1.,-0.984615384615383,-0.969230769230768,-0.953846153846152,
-0.938461538461537,-0.923076923076922,-0.907692307692306,-0.892307692307691,
-0.876923076923076,-0.86153846153846,-0.846153846153845,-0.83076923076923,
-0.815384615384614,-0.799999999999999,-0.784615384615384,-0.769230769230768,
-0.753846153846153,-0.738461538461538,-0.723076923076922,-0.707692307692307,
-0.692307692307692,-0.676923076923076,-0.661538461538461,-0.646153846153846,
-0.63076923076923,-0.615384615384615,-0.6,-0.584615384615384,-0.569230769230769,
-0.553846153846154,-0.538461538461538,-0.523076923076923,-0.507692307692308,
-0.492307692307692,-0.476923076923077,-0.461538461538462,-0.446153846153846,
-0.430769230769231,-0.415384615384615,-0.4,-0.384615384615385,-0.369230769230769,
-0.353846153846154,-0.338461538461538,-0.323076923076923,-0.307692307692308,
-0.292307692307692,-0.276923076923077,-0.261538461538462,-0.246153846153846,
-0.230769230769231,-0.215384615384615,-0.2,-0.184615384615385,-0.169230769230769,
-0.153846153846154,-0.138461538461538,-0.123076923076923,-0.107692307692308,
-0.0923076923076923,-0.0769230769230769,-0.0615384615384615,-0.0461538461538462,
-0.0307692307692308,-0.0153846153846154,-0.00577184337448646),
 .UNSPECIFIED.)
CURVE()
GEOMETRIC_REPRESENTATION_ITEM()
RATIONAL_B_SPLINE_CURVE((1.,1.,1.,1.,1.,1.,1.,1.,1.,1.,1.,1.,1.,1.,1.,1.,
1.,1.,1.,1.,1.,1.,1.,1.,1.,1.,1.,1.,1.,1.,1.,1.,1.,1.,1.,1.,1.,1.,1.,1.,
1.,1.,1.,1.,1.,1.,1.,1.,1.,1.,1.,1.,1.,1.,1.,1.,1.,1.,1.,1.,1.,1.,1.,1.,
1.,1.,1.,1.,1.,1.))
REPRESENTATION_ITEM('')
);
#322=(
BOUNDED_CURVE()
B_SPLINE_CURVE(5,(#42997,#42998,#42999,#43000,#43001,#43002,#43003,#43004,
#43005,#43006,#43007,#43008,#43009,#43010,#43011,#43012,#43013,#43014,#43015,
#43016,#43017,#43018,#43019,#43020,#43021,#43022,#43023,#43024,#43025,#43026,
#43027,#43028,#43029,#43030,#43031,#43032,#43033,#43034,#43035,#43036,#43037,
#43038,#43039,#43040,#43041,#43042,#43043,#43044,#43045,#43046,#43047,#43048,
#43049,#43050,#43051,#43052,#43053,#43054,#43055,#43056,#43057,#43058,#43059,
#43060,#43061,#43062,#43063,#43064,#43065,#43066),.UNSPECIFIED.,.F.,.F.)
B_SPLINE_CURVE_WITH_KNOTS((6,1,1,1,1,1,1,1,1,1,1,1,1,1,1,1,1,1,1,1,1,1,
1,1,1,1,1,1,1,1,1,1,1,1,1,1,1,1,1,1,1,1,1,1,1,1,1,1,1,1,1,1,1,1,1,1,1,1,
1,1,1,1,1,1,1,6),(-0.994228156739708,-0.984615384615383,-0.969230769230768,
-0.953846153846152,-0.938461538461537,-0.923076923076922,-0.907692307692306,
-0.892307692307691,-0.876923076923076,-0.86153846153846,-0.846153846153845,
-0.83076923076923,-0.815384615384614,-0.799999999999999,-0.784615384615384,
-0.769230769230768,-0.753846153846153,-0.738461538461538,-0.723076923076922,
-0.707692307692307,-0.692307692307692,-0.676923076923076,-0.661538461538461,
-0.646153846153846,-0.63076923076923,-0.615384615384615,-0.6,-0.584615384615384,
-0.569230769230769,-0.553846153846154,-0.538461538461538,-0.523076923076923,
-0.507692307692308,-0.492307692307692,-0.476923076923077,-0.461538461538462,
-0.446153846153846,-0.430769230769231,-0.415384615384615,-0.4,-0.384615384615385,
-0.369230769230769,-0.353846153846154,-0.338461538461538,-0.323076923076923,
-0.307692307692308,-0.292307692307692,-0.276923076923077,-0.261538461538462,
-0.246153846153846,-0.230769230769231,-0.215384615384615,-0.2,-0.184615384615385,
-0.169230769230769,-0.153846153846154,-0.138461538461538,-0.123076923076923,
-0.107692307692308,-0.0923076923076923,-0.0769230769230769,-0.0615384615384615,
-0.0461538461538462,-0.0307692307692308,-0.0153846153846154,0.),
 .UNSPECIFIED.)
CURVE()
GEOMETRIC_REPRESENTATION_ITEM()
RATIONAL_B_SPLINE_CURVE((1.,1.,1.,1.,1.,1.,1.,1.,1.,1.,1.,1.,1.,1.,1.,1.,
1.,1.,1.,1.,1.,1.,1.,1.,1.,1.,1.,1.,1.,1.,1.,1.,1.,1.,1.,1.,1.,1.,1.,1.,
1.,1.,1.,1.,1.,1.,1.,1.,1.,1.,1.,1.,1.,1.,1.,1.,1.,1.,1.,1.,1.,1.,1.,1.,
1.,1.,1.,1.,1.,1.))
REPRESENTATION_ITEM('')
);
#323=(
BOUNDED_CURVE()
B_SPLINE_CURVE(5,(#43219,#43220,#43221,#43222,#43223,#43224,#43225,#43226,
#43227,#43228,#43229,#43230,#43231,#43232,#43233,#43234,#43235,#43236,#43237,
#43238,#43239,#43240,#43241,#43242,#43243,#43244,#43245,#43246,#43247,#43248,
#43249,#43250,#43251,#43252,#43253,#43254,#43255,#43256,#43257,#43258,#43259,
#43260,#43261,#43262,#43263,#43264,#43265,#43266,#43267,#43268,#43269,#43270,
#43271,#43272,#43273,#43274,#43275,#43276,#43277,#43278,#43279,#43280,#43281,
#43282,#43283,#43284,#43285,#43286,#43287,#43288),.UNSPECIFIED.,.F.,.F.)
B_SPLINE_CURVE_WITH_KNOTS((6,1,1,1,1,1,1,1,1,1,1,1,1,1,1,1,1,1,1,1,1,1,
1,1,1,1,1,1,1,1,1,1,1,1,1,1,1,1,1,1,1,1,1,1,1,1,1,1,1,1,1,1,1,1,1,1,1,1,
1,1,1,1,1,1,1,6),(-1.,-0.984615384615383,-0.969230769230768,-0.953846153846152,
-0.938461538461537,-0.923076923076922,-0.907692307692306,-0.892307692307691,
-0.876923076923076,-0.86153846153846,-0.846153846153845,-0.83076923076923,
-0.815384615384614,-0.799999999999999,-0.784615384615384,-0.769230769230768,
-0.753846153846153,-0.738461538461538,-0.723076923076922,-0.707692307692307,
-0.692307692307692,-0.676923076923076,-0.661538461538461,-0.646153846153846,
-0.63076923076923,-0.615384615384615,-0.6,-0.584615384615384,-0.569230769230769,
-0.553846153846154,-0.538461538461538,-0.523076923076923,-0.507692307692308,
-0.492307692307692,-0.476923076923077,-0.461538461538462,-0.446153846153846,
-0.430769230769231,-0.415384615384615,-0.4,-0.384615384615385,-0.369230769230769,
-0.353846153846154,-0.338461538461538,-0.323076923076923,-0.307692307692308,
-0.292307692307692,-0.276923076923077,-0.261538461538462,-0.246153846153846,
-0.230769230769231,-0.215384615384615,-0.2,-0.184615384615385,-0.169230769230769,
-0.153846153846154,-0.138461538461538,-0.123076923076923,-0.107692307692308,
-0.0923076923076923,-0.0769230769230769,-0.0615384615384615,-0.0461538461538462,
-0.0307692307692308,-0.0153846153846154,-0.00577184337451626),
 .UNSPECIFIED.)
CURVE()
GEOMETRIC_REPRESENTATION_ITEM()
RATIONAL_B_SPLINE_CURVE((1.,1.,1.,1.,1.,1.,1.,1.,1.,1.,1.,1.,1.,1.,1.,1.,
1.,1.,1.,1.,1.,1.,1.,1.,1.,1.,1.,1.,1.,1.,1.,1.,1.,1.,1.,1.,1.,1.,1.,1.,
1.,1.,1.,1.,1.,1.,1.,1.,1.,1.,1.,1.,1.,1.,1.,1.,1.,1.,1.,1.,1.,1.,1.,1.,
1.,1.,1.,1.,1.,1.))
REPRESENTATION_ITEM('')
);
#324=(
BOUNDED_CURVE()
B_SPLINE_CURVE(5,(#43439,#43440,#43441,#43442,#43443,#43444,#43445,#43446,
#43447,#43448,#43449,#43450,#43451,#43452,#43453,#43454,#43455,#43456,#43457,
#43458,#43459,#43460,#43461,#43462,#43463,#43464,#43465,#43466,#43467,#43468,
#43469,#43470,#43471,#43472,#43473,#43474,#43475,#43476,#43477,#43478,#43479,
#43480,#43481,#43482,#43483,#43484,#43485,#43486,#43487,#43488,#43489,#43490,
#43491,#43492,#43493,#43494,#43495,#43496,#43497,#43498,#43499,#43500,#43501,
#43502,#43503,#43504,#43505,#43506,#43507,#43508),.UNSPECIFIED.,.F.,.F.)
B_SPLINE_CURVE_WITH_KNOTS((6,1,1,1,1,1,1,1,1,1,1,1,1,1,1,1,1,1,1,1,1,1,
1,1,1,1,1,1,1,1,1,1,1,1,1,1,1,1,1,1,1,1,1,1,1,1,1,1,1,1,1,1,1,1,1,1,1,1,
1,1,1,1,1,1,1,6),(-0.994228156739708,-0.984615384615383,-0.969230769230768,
-0.953846153846152,-0.938461538461537,-0.923076923076922,-0.907692307692306,
-0.892307692307691,-0.876923076923076,-0.86153846153846,-0.846153846153845,
-0.83076923076923,-0.815384615384614,-0.799999999999999,-0.784615384615384,
-0.769230769230768,-0.753846153846153,-0.738461538461538,-0.723076923076922,
-0.707692307692307,-0.692307692307692,-0.676923076923076,-0.661538461538461,
-0.646153846153846,-0.63076923076923,-0.615384615384615,-0.6,-0.584615384615384,
-0.569230769230769,-0.553846153846154,-0.538461538461538,-0.523076923076923,
-0.507692307692308,-0.492307692307692,-0.476923076923077,-0.461538461538462,
-0.446153846153846,-0.430769230769231,-0.415384615384615,-0.4,-0.384615384615385,
-0.369230769230769,-0.353846153846154,-0.338461538461538,-0.323076923076923,
-0.307692307692308,-0.292307692307692,-0.276923076923077,-0.261538461538462,
-0.246153846153846,-0.230769230769231,-0.215384615384615,-0.2,-0.184615384615385,
-0.169230769230769,-0.153846153846154,-0.138461538461538,-0.123076923076923,
-0.107692307692308,-0.0923076923076923,-0.0769230769230769,-0.0615384615384615,
-0.0461538461538462,-0.0307692307692308,-0.0153846153846154,0.),
 .UNSPECIFIED.)
CURVE()
GEOMETRIC_REPRESENTATION_ITEM()
RATIONAL_B_SPLINE_CURVE((1.,1.,1.,1.,1.,1.,1.,1.,1.,1.,1.,1.,1.,1.,1.,1.,
1.,1.,1.,1.,1.,1.,1.,1.,1.,1.,1.,1.,1.,1.,1.,1.,1.,1.,1.,1.,1.,1.,1.,1.,
1.,1.,1.,1.,1.,1.,1.,1.,1.,1.,1.,1.,1.,1.,1.,1.,1.,1.,1.,1.,1.,1.,1.,1.,
1.,1.,1.,1.,1.,1.))
REPRESENTATION_ITEM('')
);
#325=(
BOUNDED_CURVE()
B_SPLINE_CURVE(5,(#43661,#43662,#43663,#43664,#43665,#43666,#43667,#43668,
#43669,#43670,#43671,#43672,#43673,#43674,#43675,#43676,#43677,#43678,#43679,
#43680,#43681,#43682,#43683,#43684,#43685,#43686,#43687,#43688,#43689,#43690,
#43691,#43692,#43693,#43694,#43695,#43696,#43697,#43698,#43699,#43700,#43701,
#43702,#43703,#43704,#43705,#43706,#43707,#43708,#43709,#43710,#43711,#43712,
#43713,#43714,#43715,#43716,#43717,#43718,#43719,#43720,#43721,#43722,#43723,
#43724,#43725,#43726,#43727,#43728,#43729,#43730),.UNSPECIFIED.,.F.,.F.)
B_SPLINE_CURVE_WITH_KNOTS((6,1,1,1,1,1,1,1,1,1,1,1,1,1,1,1,1,1,1,1,1,1,
1,1,1,1,1,1,1,1,1,1,1,1,1,1,1,1,1,1,1,1,1,1,1,1,1,1,1,1,1,1,1,1,1,1,1,1,
1,1,1,1,1,1,1,6),(-1.,-0.984615384615383,-0.969230769230768,-0.953846153846152,
-0.938461538461537,-0.923076923076922,-0.907692307692306,-0.892307692307691,
-0.876923076923076,-0.86153846153846,-0.846153846153845,-0.83076923076923,
-0.815384615384614,-0.799999999999999,-0.784615384615384,-0.769230769230768,
-0.753846153846153,-0.738461538461538,-0.723076923076922,-0.707692307692307,
-0.692307692307692,-0.676923076923076,-0.661538461538461,-0.646153846153846,
-0.63076923076923,-0.615384615384615,-0.6,-0.584615384615384,-0.569230769230769,
-0.553846153846154,-0.538461538461538,-0.523076923076923,-0.507692307692308,
-0.492307692307692,-0.476923076923077,-0.461538461538462,-0.446153846153846,
-0.430769230769231,-0.415384615384615,-0.4,-0.384615384615385,-0.369230769230769,
-0.353846153846154,-0.338461538461538,-0.323076923076923,-0.307692307692308,
-0.292307692307692,-0.276923076923077,-0.261538461538462,-0.246153846153846,
-0.230769230769231,-0.215384615384615,-0.2,-0.184615384615385,-0.169230769230769,
-0.153846153846154,-0.138461538461538,-0.123076923076923,-0.107692307692308,
-0.0923076923076923,-0.0769230769230769,-0.0615384615384615,-0.0461538461538462,
-0.0307692307692308,-0.0153846153846154,-0.00577184337451372),
 .UNSPECIFIED.)
CURVE()
GEOMETRIC_REPRESENTATION_ITEM()
RATIONAL_B_SPLINE_CURVE((1.,1.,1.,1.,1.,1.,1.,1.,1.,1.,1.,1.,1.,1.,1.,1.,
1.,1.,1.,1.,1.,1.,1.,1.,1.,1.,1.,1.,1.,1.,1.,1.,1.,1.,1.,1.,1.,1.,1.,1.,
1.,1.,1.,1.,1.,1.,1.,1.,1.,1.,1.,1.,1.,1.,1.,1.,1.,1.,1.,1.,1.,1.,1.,1.,
1.,1.,1.,1.,1.,1.))
REPRESENTATION_ITEM('')
);
#326=(
BOUNDED_CURVE()
B_SPLINE_CURVE(5,(#43881,#43882,#43883,#43884,#43885,#43886,#43887,#43888,
#43889,#43890,#43891,#43892,#43893,#43894,#43895,#43896,#43897,#43898,#43899,
#43900,#43901,#43902,#43903,#43904,#43905,#43906,#43907,#43908,#43909,#43910,
#43911,#43912,#43913,#43914,#43915,#43916,#43917,#43918,#43919,#43920,#43921,
#43922,#43923,#43924,#43925,#43926,#43927,#43928,#43929,#43930,#43931,#43932,
#43933,#43934,#43935,#43936,#43937,#43938,#43939,#43940,#43941,#43942,#43943,
#43944,#43945,#43946,#43947,#43948,#43949,#43950),.UNSPECIFIED.,.F.,.F.)
B_SPLINE_CURVE_WITH_KNOTS((6,1,1,1,1,1,1,1,1,1,1,1,1,1,1,1,1,1,1,1,1,1,
1,1,1,1,1,1,1,1,1,1,1,1,1,1,1,1,1,1,1,1,1,1,1,1,1,1,1,1,1,1,1,1,1,1,1,1,
1,1,1,1,1,1,1,6),(-0.994228156739703,-0.984615384615383,-0.969230769230768,
-0.953846153846152,-0.938461538461537,-0.923076923076922,-0.907692307692306,
-0.892307692307691,-0.876923076923076,-0.86153846153846,-0.846153846153845,
-0.83076923076923,-0.815384615384614,-0.799999999999999,-0.784615384615384,
-0.769230769230768,-0.753846153846153,-0.738461538461538,-0.723076923076922,
-0.707692307692307,-0.692307692307692,-0.676923076923076,-0.661538461538461,
-0.646153846153846,-0.63076923076923,-0.615384615384615,-0.6,-0.584615384615384,
-0.569230769230769,-0.553846153846154,-0.538461538461538,-0.523076923076923,
-0.507692307692308,-0.492307692307692,-0.476923076923077,-0.461538461538462,
-0.446153846153846,-0.430769230769231,-0.415384615384615,-0.4,-0.384615384615385,
-0.369230769230769,-0.353846153846154,-0.338461538461538,-0.323076923076923,
-0.307692307692308,-0.292307692307692,-0.276923076923077,-0.261538461538462,
-0.246153846153846,-0.230769230769231,-0.215384615384615,-0.2,-0.184615384615385,
-0.169230769230769,-0.153846153846154,-0.138461538461538,-0.123076923076923,
-0.107692307692308,-0.0923076923076923,-0.0769230769230769,-0.0615384615384615,
-0.0461538461538462,-0.0307692307692308,-0.0153846153846154,0.),
 .UNSPECIFIED.)
CURVE()
GEOMETRIC_REPRESENTATION_ITEM()
RATIONAL_B_SPLINE_CURVE((1.,1.,1.,1.,1.,1.,1.,1.,1.,1.,1.,1.,1.,1.,1.,1.,
1.,1.,1.,1.,1.,1.,1.,1.,1.,1.,1.,1.,1.,1.,1.,1.,1.,1.,1.,1.,1.,1.,1.,1.,
1.,1.,1.,1.,1.,1.,1.,1.,1.,1.,1.,1.,1.,1.,1.,1.,1.,1.,1.,1.,1.,1.,1.,1.,
1.,1.,1.,1.,1.,1.))
REPRESENTATION_ITEM('')
);
#327=(
BOUNDED_CURVE()
B_SPLINE_CURVE(5,(#44103,#44104,#44105,#44106,#44107,#44108,#44109,#44110,
#44111,#44112,#44113,#44114,#44115,#44116,#44117,#44118,#44119,#44120,#44121,
#44122,#44123,#44124,#44125,#44126,#44127,#44128,#44129,#44130,#44131,#44132,
#44133,#44134,#44135,#44136,#44137,#44138,#44139,#44140,#44141,#44142,#44143,
#44144,#44145,#44146,#44147,#44148,#44149,#44150,#44151,#44152,#44153,#44154,
#44155,#44156,#44157,#44158,#44159,#44160,#44161,#44162,#44163,#44164,#44165,
#44166,#44167,#44168,#44169,#44170,#44171,#44172),.UNSPECIFIED.,.F.,.F.)
B_SPLINE_CURVE_WITH_KNOTS((6,1,1,1,1,1,1,1,1,1,1,1,1,1,1,1,1,1,1,1,1,1,
1,1,1,1,1,1,1,1,1,1,1,1,1,1,1,1,1,1,1,1,1,1,1,1,1,1,1,1,1,1,1,1,1,1,1,1,
1,1,1,1,1,1,1,6),(-1.,-0.984615384615383,-0.969230769230768,-0.953846153846152,
-0.938461538461537,-0.923076923076922,-0.907692307692306,-0.892307692307691,
-0.876923076923076,-0.86153846153846,-0.846153846153845,-0.83076923076923,
-0.815384615384614,-0.799999999999999,-0.784615384615384,-0.769230769230768,
-0.753846153846153,-0.738461538461538,-0.723076923076922,-0.707692307692307,
-0.692307692307692,-0.676923076923076,-0.661538461538461,-0.646153846153846,
-0.63076923076923,-0.615384615384615,-0.6,-0.584615384615384,-0.569230769230769,
-0.553846153846154,-0.538461538461538,-0.523076923076923,-0.507692307692308,
-0.492307692307692,-0.476923076923077,-0.461538461538462,-0.446153846153846,
-0.430769230769231,-0.415384615384615,-0.4,-0.384615384615385,-0.369230769230769,
-0.353846153846154,-0.338461538461538,-0.323076923076923,-0.307692307692308,
-0.292307692307692,-0.276923076923077,-0.261538461538462,-0.246153846153846,
-0.230769230769231,-0.215384615384615,-0.2,-0.184615384615385,-0.169230769230769,
-0.153846153846154,-0.138461538461538,-0.123076923076923,-0.107692307692308,
-0.0923076923076923,-0.0769230769230769,-0.0615384615384615,-0.0461538461538462,
-0.0307692307692308,-0.0153846153846154,-0.00577184337451698),
 .UNSPECIFIED.)
CURVE()
GEOMETRIC_REPRESENTATION_ITEM()
RATIONAL_B_SPLINE_CURVE((1.,1.,1.,1.,1.,1.,1.,1.,1.,1.,1.,1.,1.,1.,1.,1.,
1.,1.,1.,1.,1.,1.,1.,1.,1.,1.,1.,1.,1.,1.,1.,1.,1.,1.,1.,1.,1.,1.,1.,1.,
1.,1.,1.,1.,1.,1.,1.,1.,1.,1.,1.,1.,1.,1.,1.,1.,1.,1.,1.,1.,1.,1.,1.,1.,
1.,1.,1.,1.,1.,1.))
REPRESENTATION_ITEM('')
);
#328=(
BOUNDED_CURVE()
B_SPLINE_CURVE(5,(#44323,#44324,#44325,#44326,#44327,#44328,#44329,#44330,
#44331,#44332,#44333,#44334,#44335,#44336,#44337,#44338,#44339,#44340,#44341,
#44342,#44343,#44344,#44345,#44346,#44347,#44348,#44349,#44350,#44351,#44352,
#44353,#44354,#44355,#44356,#44357,#44358,#44359,#44360,#44361,#44362,#44363,
#44364,#44365,#44366,#44367,#44368,#44369,#44370,#44371,#44372,#44373,#44374,
#44375,#44376,#44377,#44378,#44379,#44380,#44381,#44382,#44383,#44384,#44385,
#44386,#44387,#44388,#44389,#44390,#44391,#44392),.UNSPECIFIED.,.F.,.F.)
B_SPLINE_CURVE_WITH_KNOTS((6,1,1,1,1,1,1,1,1,1,1,1,1,1,1,1,1,1,1,1,1,1,
1,1,1,1,1,1,1,1,1,1,1,1,1,1,1,1,1,1,1,1,1,1,1,1,1,1,1,1,1,1,1,1,1,1,1,1,
1,1,1,1,1,1,1,6),(-0.994228156739706,-0.984615384615383,-0.969230769230768,
-0.953846153846152,-0.938461538461537,-0.923076923076922,-0.907692307692306,
-0.892307692307691,-0.876923076923076,-0.86153846153846,-0.846153846153845,
-0.83076923076923,-0.815384615384614,-0.799999999999999,-0.784615384615384,
-0.769230769230768,-0.753846153846153,-0.738461538461538,-0.723076923076922,
-0.707692307692307,-0.692307692307692,-0.676923076923076,-0.661538461538461,
-0.646153846153846,-0.63076923076923,-0.615384615384615,-0.6,-0.584615384615384,
-0.569230769230769,-0.553846153846154,-0.538461538461538,-0.523076923076923,
-0.507692307692308,-0.492307692307692,-0.476923076923077,-0.461538461538462,
-0.446153846153846,-0.430769230769231,-0.415384615384615,-0.4,-0.384615384615385,
-0.369230769230769,-0.353846153846154,-0.338461538461538,-0.323076923076923,
-0.307692307692308,-0.292307692307692,-0.276923076923077,-0.261538461538462,
-0.246153846153846,-0.230769230769231,-0.215384615384615,-0.2,-0.184615384615385,
-0.169230769230769,-0.153846153846154,-0.138461538461538,-0.123076923076923,
-0.107692307692308,-0.0923076923076923,-0.0769230769230769,-0.0615384615384615,
-0.0461538461538462,-0.0307692307692308,-0.0153846153846154,0.),
 .UNSPECIFIED.)
CURVE()
GEOMETRIC_REPRESENTATION_ITEM()
RATIONAL_B_SPLINE_CURVE((1.,1.,1.,1.,1.,1.,1.,1.,1.,1.,1.,1.,1.,1.,1.,1.,
1.,1.,1.,1.,1.,1.,1.,1.,1.,1.,1.,1.,1.,1.,1.,1.,1.,1.,1.,1.,1.,1.,1.,1.,
1.,1.,1.,1.,1.,1.,1.,1.,1.,1.,1.,1.,1.,1.,1.,1.,1.,1.,1.,1.,1.,1.,1.,1.,
1.,1.,1.,1.,1.,1.))
REPRESENTATION_ITEM('')
);
#329=(
BOUNDED_CURVE()
B_SPLINE_CURVE(5,(#44545,#44546,#44547,#44548,#44549,#44550,#44551,#44552,
#44553,#44554,#44555,#44556,#44557,#44558,#44559,#44560,#44561,#44562,#44563,
#44564,#44565,#44566,#44567,#44568,#44569,#44570,#44571,#44572,#44573,#44574,
#44575,#44576,#44577,#44578,#44579,#44580,#44581,#44582,#44583,#44584,#44585,
#44586,#44587,#44588,#44589,#44590,#44591,#44592,#44593,#44594,#44595,#44596,
#44597,#44598,#44599,#44600,#44601,#44602,#44603,#44604,#44605,#44606,#44607,
#44608,#44609,#44610,#44611,#44612,#44613,#44614),.UNSPECIFIED.,.F.,.F.)
B_SPLINE_CURVE_WITH_KNOTS((6,1,1,1,1,1,1,1,1,1,1,1,1,1,1,1,1,1,1,1,1,1,
1,1,1,1,1,1,1,1,1,1,1,1,1,1,1,1,1,1,1,1,1,1,1,1,1,1,1,1,1,1,1,1,1,1,1,1,
1,1,1,1,1,1,1,6),(-1.,-0.984615384615383,-0.969230769230768,-0.953846153846152,
-0.938461538461537,-0.923076923076922,-0.907692307692306,-0.892307692307691,
-0.876923076923076,-0.86153846153846,-0.846153846153845,-0.83076923076923,
-0.815384615384614,-0.799999999999999,-0.784615384615384,-0.769230769230768,
-0.753846153846153,-0.738461538461538,-0.723076923076922,-0.707692307692307,
-0.692307692307692,-0.676923076923076,-0.661538461538461,-0.646153846153846,
-0.63076923076923,-0.615384615384615,-0.6,-0.584615384615384,-0.569230769230769,
-0.553846153846154,-0.538461538461538,-0.523076923076923,-0.507692307692308,
-0.492307692307692,-0.476923076923077,-0.461538461538462,-0.446153846153846,
-0.430769230769231,-0.415384615384615,-0.4,-0.384615384615385,-0.369230769230769,
-0.353846153846154,-0.338461538461538,-0.323076923076923,-0.307692307692308,
-0.292307692307692,-0.276923076923077,-0.261538461538462,-0.246153846153846,
-0.230769230769231,-0.215384615384615,-0.2,-0.184615384615385,-0.169230769230769,
-0.153846153846154,-0.138461538461538,-0.123076923076923,-0.107692307692308,
-0.0923076923076923,-0.0769230769230769,-0.0615384615384615,-0.0461538461538462,
-0.0307692307692308,-0.0153846153846154,-0.00577184337452512),
 .UNSPECIFIED.)
CURVE()
GEOMETRIC_REPRESENTATION_ITEM()
RATIONAL_B_SPLINE_CURVE((1.,1.,1.,1.,1.,1.,1.,1.,1.,1.,1.,1.,1.,1.,1.,1.,
1.,1.,1.,1.,1.,1.,1.,1.,1.,1.,1.,1.,1.,1.,1.,1.,1.,1.,1.,1.,1.,1.,1.,1.,
1.,1.,1.,1.,1.,1.,1.,1.,1.,1.,1.,1.,1.,1.,1.,1.,1.,1.,1.,1.,1.,1.,1.,1.,
1.,1.,1.,1.,1.,1.))
REPRESENTATION_ITEM('')
);
#330=(
BOUNDED_CURVE()
B_SPLINE_CURVE(5,(#44765,#44766,#44767,#44768,#44769,#44770,#44771,#44772,
#44773,#44774,#44775,#44776,#44777,#44778,#44779,#44780,#44781,#44782,#44783,
#44784,#44785,#44786,#44787,#44788,#44789,#44790,#44791,#44792,#44793,#44794,
#44795,#44796,#44797,#44798,#44799,#44800,#44801,#44802,#44803,#44804,#44805,
#44806,#44807,#44808,#44809,#44810,#44811,#44812,#44813,#44814,#44815,#44816,
#44817,#44818,#44819,#44820,#44821,#44822,#44823,#44824,#44825,#44826,#44827,
#44828,#44829,#44830,#44831,#44832,#44833,#44834),.UNSPECIFIED.,.F.,.F.)
B_SPLINE_CURVE_WITH_KNOTS((6,1,1,1,1,1,1,1,1,1,1,1,1,1,1,1,1,1,1,1,1,1,
1,1,1,1,1,1,1,1,1,1,1,1,1,1,1,1,1,1,1,1,1,1,1,1,1,1,1,1,1,1,1,1,1,1,1,1,
1,1,1,1,1,1,1,6),(-0.994228156739713,-0.984615384615383,-0.969230769230768,
-0.953846153846152,-0.938461538461537,-0.923076923076922,-0.907692307692306,
-0.892307692307691,-0.876923076923076,-0.86153846153846,-0.846153846153845,
-0.83076923076923,-0.815384615384614,-0.799999999999999,-0.784615384615384,
-0.769230769230768,-0.753846153846153,-0.738461538461538,-0.723076923076922,
-0.707692307692307,-0.692307692307692,-0.676923076923076,-0.661538461538461,
-0.646153846153846,-0.63076923076923,-0.615384615384615,-0.6,-0.584615384615384,
-0.569230769230769,-0.553846153846154,-0.538461538461538,-0.523076923076923,
-0.507692307692308,-0.492307692307692,-0.476923076923077,-0.461538461538462,
-0.446153846153846,-0.430769230769231,-0.415384615384615,-0.4,-0.384615384615385,
-0.369230769230769,-0.353846153846154,-0.338461538461538,-0.323076923076923,
-0.307692307692308,-0.292307692307692,-0.276923076923077,-0.261538461538462,
-0.246153846153846,-0.230769230769231,-0.215384615384615,-0.2,-0.184615384615385,
-0.169230769230769,-0.153846153846154,-0.138461538461538,-0.123076923076923,
-0.107692307692308,-0.0923076923076923,-0.0769230769230769,-0.0615384615384615,
-0.0461538461538462,-0.0307692307692308,-0.0153846153846154,0.),
 .UNSPECIFIED.)
CURVE()
GEOMETRIC_REPRESENTATION_ITEM()
RATIONAL_B_SPLINE_CURVE((1.,1.,1.,1.,1.,1.,1.,1.,1.,1.,1.,1.,1.,1.,1.,1.,
1.,1.,1.,1.,1.,1.,1.,1.,1.,1.,1.,1.,1.,1.,1.,1.,1.,1.,1.,1.,1.,1.,1.,1.,
1.,1.,1.,1.,1.,1.,1.,1.,1.,1.,1.,1.,1.,1.,1.,1.,1.,1.,1.,1.,1.,1.,1.,1.,
1.,1.,1.,1.,1.,1.))
REPRESENTATION_ITEM('')
);
#331=(
BOUNDED_CURVE()
B_SPLINE_CURVE(5,(#44987,#44988,#44989,#44990,#44991,#44992,#44993,#44994,
#44995,#44996,#44997,#44998,#44999,#45000,#45001,#45002,#45003,#45004,#45005,
#45006,#45007,#45008,#45009,#45010,#45011,#45012,#45013,#45014,#45015,#45016,
#45017,#45018,#45019,#45020,#45021,#45022,#45023,#45024,#45025,#45026,#45027,
#45028,#45029,#45030,#45031,#45032,#45033,#45034,#45035,#45036,#45037,#45038,
#45039,#45040,#45041,#45042,#45043,#45044,#45045,#45046,#45047,#45048,#45049,
#45050,#45051,#45052,#45053,#45054,#45055,#45056),.UNSPECIFIED.,.F.,.F.)
B_SPLINE_CURVE_WITH_KNOTS((6,1,1,1,1,1,1,1,1,1,1,1,1,1,1,1,1,1,1,1,1,1,
1,1,1,1,1,1,1,1,1,1,1,1,1,1,1,1,1,1,1,1,1,1,1,1,1,1,1,1,1,1,1,1,1,1,1,1,
1,1,1,1,1,1,1,6),(-1.,-0.984615384615383,-0.969230769230768,-0.953846153846152,
-0.938461538461537,-0.923076923076922,-0.907692307692306,-0.892307692307691,
-0.876923076923076,-0.86153846153846,-0.846153846153845,-0.83076923076923,
-0.815384615384614,-0.799999999999999,-0.784615384615384,-0.769230769230768,
-0.753846153846153,-0.738461538461538,-0.723076923076922,-0.707692307692307,
-0.692307692307692,-0.676923076923076,-0.661538461538461,-0.646153846153846,
-0.63076923076923,-0.615384615384615,-0.6,-0.584615384615384,-0.569230769230769,
-0.553846153846154,-0.538461538461538,-0.523076923076923,-0.507692307692308,
-0.492307692307692,-0.476923076923077,-0.461538461538462,-0.446153846153846,
-0.430769230769231,-0.415384615384615,-0.4,-0.384615384615385,-0.369230769230769,
-0.353846153846154,-0.338461538461538,-0.323076923076923,-0.307692307692308,
-0.292307692307692,-0.276923076923077,-0.261538461538462,-0.246153846153846,
-0.230769230769231,-0.215384615384615,-0.2,-0.184615384615385,-0.169230769230769,
-0.153846153846154,-0.138461538461538,-0.123076923076923,-0.107692307692308,
-0.0923076923076923,-0.0769230769230769,-0.0615384615384615,-0.0461538461538462,
-0.0307692307692308,-0.0153846153846154,-0.00577184337450204),
 .UNSPECIFIED.)
CURVE()
GEOMETRIC_REPRESENTATION_ITEM()
RATIONAL_B_SPLINE_CURVE((1.,1.,1.,1.,1.,1.,1.,1.,1.,1.,1.,1.,1.,1.,1.,1.,
1.,1.,1.,1.,1.,1.,1.,1.,1.,1.,1.,1.,1.,1.,1.,1.,1.,1.,1.,1.,1.,1.,1.,1.,
1.,1.,1.,1.,1.,1.,1.,1.,1.,1.,1.,1.,1.,1.,1.,1.,1.,1.,1.,1.,1.,1.,1.,1.,
1.,1.,1.,1.,1.,1.))
REPRESENTATION_ITEM('')
);
#332=(
BOUNDED_CURVE()
B_SPLINE_CURVE(5,(#45207,#45208,#45209,#45210,#45211,#45212,#45213,#45214,
#45215,#45216,#45217,#45218,#45219,#45220,#45221,#45222,#45223,#45224,#45225,
#45226,#45227,#45228,#45229,#45230,#45231,#45232,#45233,#45234,#45235,#45236,
#45237,#45238,#45239,#45240,#45241,#45242,#45243,#45244,#45245,#45246,#45247,
#45248,#45249,#45250,#45251,#45252,#45253,#45254,#45255,#45256,#45257,#45258,
#45259,#45260,#45261,#45262,#45263,#45264,#45265,#45266,#45267,#45268,#45269,
#45270,#45271,#45272,#45273,#45274,#45275,#45276),.UNSPECIFIED.,.F.,.F.)
B_SPLINE_CURVE_WITH_KNOTS((6,1,1,1,1,1,1,1,1,1,1,1,1,1,1,1,1,1,1,1,1,1,
1,1,1,1,1,1,1,1,1,1,1,1,1,1,1,1,1,1,1,1,1,1,1,1,1,1,1,1,1,1,1,1,1,1,1,1,
1,1,1,1,1,1,1,6),(-0.99422815673972,-0.984615384615383,-0.969230769230768,
-0.953846153846152,-0.938461538461537,-0.923076923076922,-0.907692307692306,
-0.892307692307691,-0.876923076923076,-0.86153846153846,-0.846153846153845,
-0.83076923076923,-0.815384615384614,-0.799999999999999,-0.784615384615384,
-0.769230769230768,-0.753846153846153,-0.738461538461538,-0.723076923076922,
-0.707692307692307,-0.692307692307692,-0.676923076923076,-0.661538461538461,
-0.646153846153846,-0.63076923076923,-0.615384615384615,-0.6,-0.584615384615384,
-0.569230769230769,-0.553846153846154,-0.538461538461538,-0.523076923076923,
-0.507692307692308,-0.492307692307692,-0.476923076923077,-0.461538461538462,
-0.446153846153846,-0.430769230769231,-0.415384615384615,-0.4,-0.384615384615385,
-0.369230769230769,-0.353846153846154,-0.338461538461538,-0.323076923076923,
-0.307692307692308,-0.292307692307692,-0.276923076923077,-0.261538461538462,
-0.246153846153846,-0.230769230769231,-0.215384615384615,-0.2,-0.184615384615385,
-0.169230769230769,-0.153846153846154,-0.138461538461538,-0.123076923076923,
-0.107692307692308,-0.0923076923076923,-0.0769230769230769,-0.0615384615384615,
-0.0461538461538462,-0.0307692307692308,-0.0153846153846154,0.),
 .UNSPECIFIED.)
CURVE()
GEOMETRIC_REPRESENTATION_ITEM()
RATIONAL_B_SPLINE_CURVE((1.,1.,1.,1.,1.,1.,1.,1.,1.,1.,1.,1.,1.,1.,1.,1.,
1.,1.,1.,1.,1.,1.,1.,1.,1.,1.,1.,1.,1.,1.,1.,1.,1.,1.,1.,1.,1.,1.,1.,1.,
1.,1.,1.,1.,1.,1.,1.,1.,1.,1.,1.,1.,1.,1.,1.,1.,1.,1.,1.,1.,1.,1.,1.,1.,
1.,1.,1.,1.,1.,1.))
REPRESENTATION_ITEM('')
);
#333=(
BOUNDED_CURVE()
B_SPLINE_CURVE(5,(#45429,#45430,#45431,#45432,#45433,#45434,#45435,#45436,
#45437,#45438,#45439,#45440,#45441,#45442,#45443,#45444,#45445,#45446,#45447,
#45448,#45449,#45450,#45451,#45452,#45453,#45454,#45455,#45456,#45457,#45458,
#45459,#45460,#45461,#45462,#45463,#45464,#45465,#45466,#45467,#45468,#45469,
#45470,#45471,#45472,#45473,#45474,#45475,#45476,#45477,#45478,#45479,#45480,
#45481,#45482,#45483,#45484,#45485,#45486,#45487,#45488,#45489,#45490,#45491,
#45492,#45493,#45494,#45495,#45496,#45497,#45498),.UNSPECIFIED.,.F.,.F.)
B_SPLINE_CURVE_WITH_KNOTS((6,1,1,1,1,1,1,1,1,1,1,1,1,1,1,1,1,1,1,1,1,1,
1,1,1,1,1,1,1,1,1,1,1,1,1,1,1,1,1,1,1,1,1,1,1,1,1,1,1,1,1,1,1,1,1,1,1,1,
1,1,1,1,1,1,1,6),(-1.,-0.984615384615383,-0.969230769230768,-0.953846153846152,
-0.938461538461537,-0.923076923076922,-0.907692307692306,-0.892307692307691,
-0.876923076923076,-0.86153846153846,-0.846153846153845,-0.83076923076923,
-0.815384615384614,-0.799999999999999,-0.784615384615384,-0.769230769230768,
-0.753846153846153,-0.738461538461538,-0.723076923076922,-0.707692307692307,
-0.692307692307692,-0.676923076923076,-0.661538461538461,-0.646153846153846,
-0.63076923076923,-0.615384615384615,-0.6,-0.584615384615384,-0.569230769230769,
-0.553846153846154,-0.538461538461538,-0.523076923076923,-0.507692307692308,
-0.492307692307692,-0.476923076923077,-0.461538461538462,-0.446153846153846,
-0.430769230769231,-0.415384615384615,-0.4,-0.384615384615385,-0.369230769230769,
-0.353846153846154,-0.338461538461538,-0.323076923076923,-0.307692307692308,
-0.292307692307692,-0.276923076923077,-0.261538461538462,-0.246153846153846,
-0.230769230769231,-0.215384615384615,-0.2,-0.184615384615385,-0.169230769230769,
-0.153846153846154,-0.138461538461538,-0.123076923076923,-0.107692307692308,
-0.0923076923076923,-0.0769230769230769,-0.0615384615384615,-0.0461538461538462,
-0.0307692307692308,-0.0153846153846154,-0.0057718433745107),
 .UNSPECIFIED.)
CURVE()
GEOMETRIC_REPRESENTATION_ITEM()
RATIONAL_B_SPLINE_CURVE((1.,1.,1.,1.,1.,1.,1.,1.,1.,1.,1.,1.,1.,1.,1.,1.,
1.,1.,1.,1.,1.,1.,1.,1.,1.,1.,1.,1.,1.,1.,1.,1.,1.,1.,1.,1.,1.,1.,1.,1.,
1.,1.,1.,1.,1.,1.,1.,1.,1.,1.,1.,1.,1.,1.,1.,1.,1.,1.,1.,1.,1.,1.,1.,1.,
1.,1.,1.,1.,1.,1.))
REPRESENTATION_ITEM('')
);
#334=(
BOUNDED_CURVE()
B_SPLINE_CURVE(5,(#45649,#45650,#45651,#45652,#45653,#45654,#45655,#45656,
#45657,#45658,#45659,#45660,#45661,#45662,#45663,#45664,#45665,#45666,#45667,
#45668,#45669,#45670,#45671,#45672,#45673,#45674,#45675,#45676,#45677,#45678,
#45679,#45680,#45681,#45682,#45683,#45684,#45685,#45686,#45687,#45688,#45689,
#45690,#45691,#45692,#45693,#45694,#45695,#45696,#45697,#45698,#45699,#45700,
#45701,#45702,#45703,#45704,#45705,#45706,#45707,#45708,#45709,#45710,#45711,
#45712,#45713,#45714,#45715,#45716,#45717,#45718),.UNSPECIFIED.,.F.,.F.)
B_SPLINE_CURVE_WITH_KNOTS((6,1,1,1,1,1,1,1,1,1,1,1,1,1,1,1,1,1,1,1,1,1,
1,1,1,1,1,1,1,1,1,1,1,1,1,1,1,1,1,1,1,1,1,1,1,1,1,1,1,1,1,1,1,1,1,1,1,1,
1,1,1,1,1,1,1,6),(-0.994228156739708,-0.984615384615383,-0.969230769230768,
-0.953846153846152,-0.938461538461537,-0.923076923076922,-0.907692307692306,
-0.892307692307691,-0.876923076923076,-0.86153846153846,-0.846153846153845,
-0.83076923076923,-0.815384615384614,-0.799999999999999,-0.784615384615384,
-0.769230769230768,-0.753846153846153,-0.738461538461538,-0.723076923076922,
-0.707692307692307,-0.692307692307692,-0.676923076923076,-0.661538461538461,
-0.646153846153846,-0.63076923076923,-0.615384615384615,-0.6,-0.584615384615384,
-0.569230769230769,-0.553846153846154,-0.538461538461538,-0.523076923076923,
-0.507692307692308,-0.492307692307692,-0.476923076923077,-0.461538461538462,
-0.446153846153846,-0.430769230769231,-0.415384615384615,-0.4,-0.384615384615385,
-0.369230769230769,-0.353846153846154,-0.338461538461538,-0.323076923076923,
-0.307692307692308,-0.292307692307692,-0.276923076923077,-0.261538461538462,
-0.246153846153846,-0.230769230769231,-0.215384615384615,-0.2,-0.184615384615385,
-0.169230769230769,-0.153846153846154,-0.138461538461538,-0.123076923076923,
-0.107692307692308,-0.0923076923076923,-0.0769230769230769,-0.0615384615384615,
-0.0461538461538462,-0.0307692307692308,-0.0153846153846154,0.),
 .UNSPECIFIED.)
CURVE()
GEOMETRIC_REPRESENTATION_ITEM()
RATIONAL_B_SPLINE_CURVE((1.,1.,1.,1.,1.,1.,1.,1.,1.,1.,1.,1.,1.,1.,1.,1.,
1.,1.,1.,1.,1.,1.,1.,1.,1.,1.,1.,1.,1.,1.,1.,1.,1.,1.,1.,1.,1.,1.,1.,1.,
1.,1.,1.,1.,1.,1.,1.,1.,1.,1.,1.,1.,1.,1.,1.,1.,1.,1.,1.,1.,1.,1.,1.,1.,
1.,1.,1.,1.,1.,1.))
REPRESENTATION_ITEM('')
);
#335=(
BOUNDED_CURVE()
B_SPLINE_CURVE(5,(#45871,#45872,#45873,#45874,#45875,#45876,#45877,#45878,
#45879,#45880,#45881,#45882,#45883,#45884,#45885,#45886,#45887,#45888,#45889,
#45890,#45891,#45892,#45893,#45894,#45895,#45896,#45897,#45898,#45899,#45900,
#45901,#45902,#45903,#45904,#45905,#45906,#45907,#45908,#45909,#45910,#45911,
#45912,#45913,#45914,#45915,#45916,#45917,#45918,#45919,#45920,#45921,#45922,
#45923,#45924,#45925,#45926,#45927,#45928,#45929,#45930,#45931,#45932,#45933,
#45934,#45935,#45936,#45937,#45938,#45939,#45940),.UNSPECIFIED.,.F.,.F.)
B_SPLINE_CURVE_WITH_KNOTS((6,1,1,1,1,1,1,1,1,1,1,1,1,1,1,1,1,1,1,1,1,1,
1,1,1,1,1,1,1,1,1,1,1,1,1,1,1,1,1,1,1,1,1,1,1,1,1,1,1,1,1,1,1,1,1,1,1,1,
1,1,1,1,1,1,1,6),(-1.,-0.984615384615383,-0.969230769230768,-0.953846153846152,
-0.938461538461537,-0.923076923076922,-0.907692307692306,-0.892307692307691,
-0.876923076923076,-0.86153846153846,-0.846153846153845,-0.83076923076923,
-0.815384615384614,-0.799999999999999,-0.784615384615384,-0.769230769230768,
-0.753846153846153,-0.738461538461538,-0.723076923076922,-0.707692307692307,
-0.692307692307692,-0.676923076923076,-0.661538461538461,-0.646153846153846,
-0.63076923076923,-0.615384615384615,-0.6,-0.584615384615384,-0.569230769230769,
-0.553846153846154,-0.538461538461538,-0.523076923076923,-0.507692307692308,
-0.492307692307692,-0.476923076923077,-0.461538461538462,-0.446153846153846,
-0.430769230769231,-0.415384615384615,-0.4,-0.384615384615385,-0.369230769230769,
-0.353846153846154,-0.338461538461538,-0.323076923076923,-0.307692307692308,
-0.292307692307692,-0.276923076923077,-0.261538461538462,-0.246153846153846,
-0.230769230769231,-0.215384615384615,-0.2,-0.184615384615385,-0.169230769230769,
-0.153846153846154,-0.138461538461538,-0.123076923076923,-0.107692307692308,
-0.0923076923076923,-0.0769230769230769,-0.0615384615384615,-0.0461538461538462,
-0.0307692307692308,-0.0153846153846154,-0.00577184337451708),
 .UNSPECIFIED.)
CURVE()
GEOMETRIC_REPRESENTATION_ITEM()
RATIONAL_B_SPLINE_CURVE((1.,1.,1.,1.,1.,1.,1.,1.,1.,1.,1.,1.,1.,1.,1.,1.,
1.,1.,1.,1.,1.,1.,1.,1.,1.,1.,1.,1.,1.,1.,1.,1.,1.,1.,1.,1.,1.,1.,1.,1.,
1.,1.,1.,1.,1.,1.,1.,1.,1.,1.,1.,1.,1.,1.,1.,1.,1.,1.,1.,1.,1.,1.,1.,1.,
1.,1.,1.,1.,1.,1.))
REPRESENTATION_ITEM('')
);
#336=(
BOUNDED_CURVE()
B_SPLINE_CURVE(5,(#46091,#46092,#46093,#46094,#46095,#46096,#46097,#46098,
#46099,#46100,#46101,#46102,#46103,#46104,#46105,#46106,#46107,#46108,#46109,
#46110,#46111,#46112,#46113,#46114,#46115,#46116,#46117,#46118,#46119,#46120,
#46121,#46122,#46123,#46124,#46125,#46126,#46127,#46128,#46129,#46130,#46131,
#46132,#46133,#46134,#46135,#46136,#46137,#46138,#46139,#46140,#46141,#46142,
#46143,#46144,#46145,#46146,#46147,#46148,#46149,#46150,#46151,#46152,#46153,
#46154,#46155,#46156,#46157,#46158,#46159,#46160),.UNSPECIFIED.,.F.,.F.)
B_SPLINE_CURVE_WITH_KNOTS((6,1,1,1,1,1,1,1,1,1,1,1,1,1,1,1,1,1,1,1,1,1,
1,1,1,1,1,1,1,1,1,1,1,1,1,1,1,1,1,1,1,1,1,1,1,1,1,1,1,1,1,1,1,1,1,1,1,1,
1,1,1,1,1,1,1,6),(-0.994228156739669,-0.984615384615383,-0.969230769230768,
-0.953846153846152,-0.938461538461537,-0.923076923076922,-0.907692307692306,
-0.892307692307691,-0.876923076923076,-0.86153846153846,-0.846153846153845,
-0.83076923076923,-0.815384615384614,-0.799999999999999,-0.784615384615384,
-0.769230769230768,-0.753846153846153,-0.738461538461538,-0.723076923076922,
-0.707692307692307,-0.692307692307692,-0.676923076923076,-0.661538461538461,
-0.646153846153846,-0.63076923076923,-0.615384615384615,-0.6,-0.584615384615384,
-0.569230769230769,-0.553846153846154,-0.538461538461538,-0.523076923076923,
-0.507692307692308,-0.492307692307692,-0.476923076923077,-0.461538461538462,
-0.446153846153846,-0.430769230769231,-0.415384615384615,-0.4,-0.384615384615385,
-0.369230769230769,-0.353846153846154,-0.338461538461538,-0.323076923076923,
-0.307692307692308,-0.292307692307692,-0.276923076923077,-0.261538461538462,
-0.246153846153846,-0.230769230769231,-0.215384615384615,-0.2,-0.184615384615385,
-0.169230769230769,-0.153846153846154,-0.138461538461538,-0.123076923076923,
-0.107692307692308,-0.0923076923076923,-0.0769230769230769,-0.0615384615384615,
-0.0461538461538462,-0.0307692307692308,-0.0153846153846154,0.),
 .UNSPECIFIED.)
CURVE()
GEOMETRIC_REPRESENTATION_ITEM()
RATIONAL_B_SPLINE_CURVE((1.,1.,1.,1.,1.,1.,1.,1.,1.,1.,1.,1.,1.,1.,1.,1.,
1.,1.,1.,1.,1.,1.,1.,1.,1.,1.,1.,1.,1.,1.,1.,1.,1.,1.,1.,1.,1.,1.,1.,1.,
1.,1.,1.,1.,1.,1.,1.,1.,1.,1.,1.,1.,1.,1.,1.,1.,1.,1.,1.,1.,1.,1.,1.,1.,
1.,1.,1.,1.,1.,1.))
REPRESENTATION_ITEM('')
);
#337=(
BOUNDED_CURVE()
B_SPLINE_CURVE(5,(#46313,#46314,#46315,#46316,#46317,#46318,#46319,#46320,
#46321,#46322,#46323,#46324,#46325,#46326,#46327,#46328,#46329,#46330,#46331,
#46332,#46333,#46334,#46335,#46336,#46337,#46338,#46339,#46340,#46341,#46342,
#46343,#46344,#46345,#46346,#46347,#46348,#46349,#46350,#46351,#46352,#46353,
#46354,#46355,#46356,#46357,#46358,#46359,#46360,#46361,#46362,#46363,#46364,
#46365,#46366,#46367,#46368,#46369,#46370,#46371,#46372,#46373,#46374,#46375,
#46376,#46377,#46378,#46379,#46380,#46381,#46382),.UNSPECIFIED.,.F.,.F.)
B_SPLINE_CURVE_WITH_KNOTS((6,1,1,1,1,1,1,1,1,1,1,1,1,1,1,1,1,1,1,1,1,1,
1,1,1,1,1,1,1,1,1,1,1,1,1,1,1,1,1,1,1,1,1,1,1,1,1,1,1,1,1,1,1,1,1,1,1,1,
1,1,1,1,1,1,1,6),(-1.,-0.984615384615383,-0.969230769230768,-0.953846153846152,
-0.938461538461537,-0.923076923076922,-0.907692307692306,-0.892307692307691,
-0.876923076923076,-0.86153846153846,-0.846153846153845,-0.83076923076923,
-0.815384615384614,-0.799999999999999,-0.784615384615384,-0.769230769230768,
-0.753846153846153,-0.738461538461538,-0.723076923076922,-0.707692307692307,
-0.692307692307692,-0.676923076923076,-0.661538461538461,-0.646153846153846,
-0.63076923076923,-0.615384615384615,-0.6,-0.584615384615384,-0.569230769230769,
-0.553846153846154,-0.538461538461538,-0.523076923076923,-0.507692307692308,
-0.492307692307692,-0.476923076923077,-0.461538461538462,-0.446153846153846,
-0.430769230769231,-0.415384615384615,-0.4,-0.384615384615385,-0.369230769230769,
-0.353846153846154,-0.338461538461538,-0.323076923076923,-0.307692307692308,
-0.292307692307692,-0.276923076923077,-0.261538461538462,-0.246153846153846,
-0.230769230769231,-0.215384615384615,-0.2,-0.184615384615385,-0.169230769230769,
-0.153846153846154,-0.138461538461538,-0.123076923076923,-0.107692307692308,
-0.0923076923076923,-0.0769230769230769,-0.0615384615384615,-0.0461538461538462,
-0.0307692307692308,-0.0153846153846154,-0.0057718433744903),
 .UNSPECIFIED.)
CURVE()
GEOMETRIC_REPRESENTATION_ITEM()
RATIONAL_B_SPLINE_CURVE((1.,1.,1.,1.,1.,1.,1.,1.,1.,1.,1.,1.,1.,1.,1.,1.,
1.,1.,1.,1.,1.,1.,1.,1.,1.,1.,1.,1.,1.,1.,1.,1.,1.,1.,1.,1.,1.,1.,1.,1.,
1.,1.,1.,1.,1.,1.,1.,1.,1.,1.,1.,1.,1.,1.,1.,1.,1.,1.,1.,1.,1.,1.,1.,1.,
1.,1.,1.,1.,1.,1.))
REPRESENTATION_ITEM('')
);
#338=(
BOUNDED_CURVE()
B_SPLINE_CURVE(5,(#46533,#46534,#46535,#46536,#46537,#46538,#46539,#46540,
#46541,#46542,#46543,#46544,#46545,#46546,#46547,#46548,#46549,#46550,#46551,
#46552,#46553,#46554,#46555,#46556,#46557,#46558,#46559,#46560,#46561,#46562,
#46563,#46564,#46565,#46566,#46567,#46568,#46569,#46570,#46571,#46572,#46573,
#46574,#46575,#46576,#46577,#46578,#46579,#46580,#46581,#46582,#46583,#46584,
#46585,#46586,#46587,#46588,#46589,#46590,#46591,#46592,#46593,#46594,#46595,
#46596,#46597,#46598,#46599,#46600,#46601,#46602),.UNSPECIFIED.,.F.,.F.)
B_SPLINE_CURVE_WITH_KNOTS((6,1,1,1,1,1,1,1,1,1,1,1,1,1,1,1,1,1,1,1,1,1,
1,1,1,1,1,1,1,1,1,1,1,1,1,1,1,1,1,1,1,1,1,1,1,1,1,1,1,1,1,1,1,1,1,1,1,1,
1,1,1,1,1,1,1,6),(-0.994228156739712,-0.984615384615383,-0.969230769230768,
-0.953846153846152,-0.938461538461537,-0.923076923076922,-0.907692307692306,
-0.892307692307691,-0.876923076923076,-0.86153846153846,-0.846153846153845,
-0.83076923076923,-0.815384615384614,-0.799999999999999,-0.784615384615384,
-0.769230769230768,-0.753846153846153,-0.738461538461538,-0.723076923076922,
-0.707692307692307,-0.692307692307692,-0.676923076923076,-0.661538461538461,
-0.646153846153846,-0.63076923076923,-0.615384615384615,-0.6,-0.584615384615384,
-0.569230769230769,-0.553846153846154,-0.538461538461538,-0.523076923076923,
-0.507692307692308,-0.492307692307692,-0.476923076923077,-0.461538461538462,
-0.446153846153846,-0.430769230769231,-0.415384615384615,-0.4,-0.384615384615385,
-0.369230769230769,-0.353846153846154,-0.338461538461538,-0.323076923076923,
-0.307692307692308,-0.292307692307692,-0.276923076923077,-0.261538461538462,
-0.246153846153846,-0.230769230769231,-0.215384615384615,-0.2,-0.184615384615385,
-0.169230769230769,-0.153846153846154,-0.138461538461538,-0.123076923076923,
-0.107692307692308,-0.0923076923076923,-0.0769230769230769,-0.0615384615384615,
-0.0461538461538462,-0.0307692307692308,-0.0153846153846154,0.),
 .UNSPECIFIED.)
CURVE()
GEOMETRIC_REPRESENTATION_ITEM()
RATIONAL_B_SPLINE_CURVE((1.,1.,1.,1.,1.,1.,1.,1.,1.,1.,1.,1.,1.,1.,1.,1.,
1.,1.,1.,1.,1.,1.,1.,1.,1.,1.,1.,1.,1.,1.,1.,1.,1.,1.,1.,1.,1.,1.,1.,1.,
1.,1.,1.,1.,1.,1.,1.,1.,1.,1.,1.,1.,1.,1.,1.,1.,1.,1.,1.,1.,1.,1.,1.,1.,
1.,1.,1.,1.,1.,1.))
REPRESENTATION_ITEM('')
);
#339=(
BOUNDED_CURVE()
B_SPLINE_CURVE(5,(#46755,#46756,#46757,#46758,#46759,#46760,#46761,#46762,
#46763,#46764,#46765,#46766,#46767,#46768,#46769,#46770,#46771,#46772,#46773,
#46774,#46775,#46776,#46777,#46778,#46779,#46780,#46781,#46782,#46783,#46784,
#46785,#46786,#46787,#46788,#46789,#46790,#46791,#46792,#46793,#46794,#46795,
#46796,#46797,#46798,#46799,#46800,#46801,#46802,#46803,#46804,#46805,#46806,
#46807,#46808,#46809,#46810,#46811,#46812,#46813,#46814,#46815,#46816,#46817,
#46818,#46819,#46820,#46821,#46822,#46823,#46824),.UNSPECIFIED.,.F.,.F.)
B_SPLINE_CURVE_WITH_KNOTS((6,1,1,1,1,1,1,1,1,1,1,1,1,1,1,1,1,1,1,1,1,1,
1,1,1,1,1,1,1,1,1,1,1,1,1,1,1,1,1,1,1,1,1,1,1,1,1,1,1,1,1,1,1,1,1,1,1,1,
1,1,1,1,1,1,1,6),(-1.,-0.984615384615383,-0.969230769230768,-0.953846153846152,
-0.938461538461537,-0.923076923076922,-0.907692307692306,-0.892307692307691,
-0.876923076923076,-0.86153846153846,-0.846153846153845,-0.83076923076923,
-0.815384615384614,-0.799999999999999,-0.784615384615384,-0.769230769230768,
-0.753846153846153,-0.738461538461538,-0.723076923076922,-0.707692307692307,
-0.692307692307692,-0.676923076923076,-0.661538461538461,-0.646153846153846,
-0.63076923076923,-0.615384615384615,-0.6,-0.584615384615384,-0.569230769230769,
-0.553846153846154,-0.538461538461538,-0.523076923076923,-0.507692307692308,
-0.492307692307692,-0.476923076923077,-0.461538461538462,-0.446153846153846,
-0.430769230769231,-0.415384615384615,-0.4,-0.384615384615385,-0.369230769230769,
-0.353846153846154,-0.338461538461538,-0.323076923076923,-0.307692307692308,
-0.292307692307692,-0.276923076923077,-0.261538461538462,-0.246153846153846,
-0.230769230769231,-0.215384615384615,-0.2,-0.184615384615385,-0.169230769230769,
-0.153846153846154,-0.138461538461538,-0.123076923076923,-0.107692307692308,
-0.0923076923076923,-0.0769230769230769,-0.0615384615384615,-0.0461538461538462,
-0.0307692307692308,-0.0153846153846154,-0.0057718433745291),
 .UNSPECIFIED.)
CURVE()
GEOMETRIC_REPRESENTATION_ITEM()
RATIONAL_B_SPLINE_CURVE((1.,1.,1.,1.,1.,1.,1.,1.,1.,1.,1.,1.,1.,1.,1.,1.,
1.,1.,1.,1.,1.,1.,1.,1.,1.,1.,1.,1.,1.,1.,1.,1.,1.,1.,1.,1.,1.,1.,1.,1.,
1.,1.,1.,1.,1.,1.,1.,1.,1.,1.,1.,1.,1.,1.,1.,1.,1.,1.,1.,1.,1.,1.,1.,1.,
1.,1.,1.,1.,1.,1.))
REPRESENTATION_ITEM('')
);
#340=(
BOUNDED_CURVE()
B_SPLINE_CURVE(5,(#46975,#46976,#46977,#46978,#46979,#46980,#46981,#46982,
#46983,#46984,#46985,#46986,#46987,#46988,#46989,#46990,#46991,#46992,#46993,
#46994,#46995,#46996,#46997,#46998,#46999,#47000,#47001,#47002,#47003,#47004,
#47005,#47006,#47007,#47008,#47009,#47010,#47011,#47012,#47013,#47014,#47015,
#47016,#47017,#47018,#47019,#47020,#47021,#47022,#47023,#47024,#47025,#47026,
#47027,#47028,#47029,#47030,#47031,#47032,#47033,#47034,#47035,#47036,#47037,
#47038,#47039,#47040,#47041,#47042,#47043,#47044),.UNSPECIFIED.,.F.,.F.)
B_SPLINE_CURVE_WITH_KNOTS((6,1,1,1,1,1,1,1,1,1,1,1,1,1,1,1,1,1,1,1,1,1,
1,1,1,1,1,1,1,1,1,1,1,1,1,1,1,1,1,1,1,1,1,1,1,1,1,1,1,1,1,1,1,1,1,1,1,1,
1,1,1,1,1,1,1,6),(-0.994228156739695,-0.984615384615383,-0.969230769230768,
-0.953846153846152,-0.938461538461537,-0.923076923076922,-0.907692307692306,
-0.892307692307691,-0.876923076923076,-0.86153846153846,-0.846153846153845,
-0.83076923076923,-0.815384615384614,-0.799999999999999,-0.784615384615384,
-0.769230769230768,-0.753846153846153,-0.738461538461538,-0.723076923076922,
-0.707692307692307,-0.692307692307692,-0.676923076923076,-0.661538461538461,
-0.646153846153846,-0.63076923076923,-0.615384615384615,-0.6,-0.584615384615384,
-0.569230769230769,-0.553846153846154,-0.538461538461538,-0.523076923076923,
-0.507692307692308,-0.492307692307692,-0.476923076923077,-0.461538461538462,
-0.446153846153846,-0.430769230769231,-0.415384615384615,-0.4,-0.384615384615385,
-0.369230769230769,-0.353846153846154,-0.338461538461538,-0.323076923076923,
-0.307692307692308,-0.292307692307692,-0.276923076923077,-0.261538461538462,
-0.246153846153846,-0.230769230769231,-0.215384615384615,-0.2,-0.184615384615385,
-0.169230769230769,-0.153846153846154,-0.138461538461538,-0.123076923076923,
-0.107692307692308,-0.0923076923076923,-0.0769230769230769,-0.0615384615384615,
-0.0461538461538462,-0.0307692307692308,-0.0153846153846154,0.),
 .UNSPECIFIED.)
CURVE()
GEOMETRIC_REPRESENTATION_ITEM()
RATIONAL_B_SPLINE_CURVE((1.,1.,1.,1.,1.,1.,1.,1.,1.,1.,1.,1.,1.,1.,1.,1.,
1.,1.,1.,1.,1.,1.,1.,1.,1.,1.,1.,1.,1.,1.,1.,1.,1.,1.,1.,1.,1.,1.,1.,1.,
1.,1.,1.,1.,1.,1.,1.,1.,1.,1.,1.,1.,1.,1.,1.,1.,1.,1.,1.,1.,1.,1.,1.,1.,
1.,1.,1.,1.,1.,1.))
REPRESENTATION_ITEM('')
);
#341=(
BOUNDED_CURVE()
B_SPLINE_CURVE(5,(#47197,#47198,#47199,#47200,#47201,#47202,#47203,#47204,
#47205,#47206,#47207,#47208,#47209,#47210,#47211,#47212,#47213,#47214,#47215,
#47216,#47217,#47218,#47219,#47220,#47221,#47222,#47223,#47224,#47225,#47226,
#47227,#47228,#47229,#47230,#47231,#47232,#47233,#47234,#47235,#47236,#47237,
#47238,#47239,#47240,#47241,#47242,#47243,#47244,#47245,#47246,#47247,#47248,
#47249,#47250,#47251,#47252,#47253,#47254,#47255,#47256,#47257,#47258,#47259,
#47260,#47261,#47262,#47263,#47264,#47265,#47266),.UNSPECIFIED.,.F.,.F.)
B_SPLINE_CURVE_WITH_KNOTS((6,1,1,1,1,1,1,1,1,1,1,1,1,1,1,1,1,1,1,1,1,1,
1,1,1,1,1,1,1,1,1,1,1,1,1,1,1,1,1,1,1,1,1,1,1,1,1,1,1,1,1,1,1,1,1,1,1,1,
1,1,1,1,1,1,1,6),(-1.,-0.984615384615383,-0.969230769230768,-0.953846153846152,
-0.938461538461537,-0.923076923076922,-0.907692307692306,-0.892307692307691,
-0.876923076923076,-0.86153846153846,-0.846153846153845,-0.83076923076923,
-0.815384615384614,-0.799999999999999,-0.784615384615384,-0.769230769230768,
-0.753846153846153,-0.738461538461538,-0.723076923076922,-0.707692307692307,
-0.692307692307692,-0.676923076923076,-0.661538461538461,-0.646153846153846,
-0.63076923076923,-0.615384615384615,-0.6,-0.584615384615384,-0.569230769230769,
-0.553846153846154,-0.538461538461538,-0.523076923076923,-0.507692307692308,
-0.492307692307692,-0.476923076923077,-0.461538461538462,-0.446153846153846,
-0.430769230769231,-0.415384615384615,-0.4,-0.384615384615385,-0.369230769230769,
-0.353846153846154,-0.338461538461538,-0.323076923076923,-0.307692307692308,
-0.292307692307692,-0.276923076923077,-0.261538461538462,-0.246153846153846,
-0.230769230769231,-0.215384615384615,-0.2,-0.184615384615385,-0.169230769230769,
-0.153846153846154,-0.138461538461538,-0.123076923076923,-0.107692307692308,
-0.0923076923076923,-0.0769230769230769,-0.0615384615384615,-0.0461538461538462,
-0.0307692307692308,-0.0153846153846154,-0.00577184337450344),
 .UNSPECIFIED.)
CURVE()
GEOMETRIC_REPRESENTATION_ITEM()
RATIONAL_B_SPLINE_CURVE((1.,1.,1.,1.,1.,1.,1.,1.,1.,1.,1.,1.,1.,1.,1.,1.,
1.,1.,1.,1.,1.,1.,1.,1.,1.,1.,1.,1.,1.,1.,1.,1.,1.,1.,1.,1.,1.,1.,1.,1.,
1.,1.,1.,1.,1.,1.,1.,1.,1.,1.,1.,1.,1.,1.,1.,1.,1.,1.,1.,1.,1.,1.,1.,1.,
1.,1.,1.,1.,1.,1.))
REPRESENTATION_ITEM('')
);
#342=(
BOUNDED_CURVE()
B_SPLINE_CURVE(5,(#47417,#47418,#47419,#47420,#47421,#47422,#47423,#47424,
#47425,#47426,#47427,#47428,#47429,#47430,#47431,#47432,#47433,#47434,#47435,
#47436,#47437,#47438,#47439,#47440,#47441,#47442,#47443,#47444,#47445,#47446,
#47447,#47448,#47449,#47450,#47451,#47452,#47453,#47454,#47455,#47456,#47457,
#47458,#47459,#47460,#47461,#47462,#47463,#47464,#47465,#47466,#47467,#47468,
#47469,#47470,#47471,#47472,#47473,#47474,#47475,#47476,#47477,#47478,#47479,
#47480,#47481,#47482,#47483,#47484,#47485,#47486),.UNSPECIFIED.,.F.,.F.)
B_SPLINE_CURVE_WITH_KNOTS((6,1,1,1,1,1,1,1,1,1,1,1,1,1,1,1,1,1,1,1,1,1,
1,1,1,1,1,1,1,1,1,1,1,1,1,1,1,1,1,1,1,1,1,1,1,1,1,1,1,1,1,1,1,1,1,1,1,1,
1,1,1,1,1,1,1,6),(-0.994228156739669,-0.984615384615383,-0.969230769230768,
-0.953846153846152,-0.938461538461537,-0.923076923076922,-0.907692307692306,
-0.892307692307691,-0.876923076923076,-0.86153846153846,-0.846153846153845,
-0.83076923076923,-0.815384615384614,-0.799999999999999,-0.784615384615384,
-0.769230769230768,-0.753846153846153,-0.738461538461538,-0.723076923076922,
-0.707692307692307,-0.692307692307692,-0.676923076923076,-0.661538461538461,
-0.646153846153846,-0.63076923076923,-0.615384615384615,-0.6,-0.584615384615384,
-0.569230769230769,-0.553846153846154,-0.538461538461538,-0.523076923076923,
-0.507692307692308,-0.492307692307692,-0.476923076923077,-0.461538461538462,
-0.446153846153846,-0.430769230769231,-0.415384615384615,-0.4,-0.384615384615385,
-0.369230769230769,-0.353846153846154,-0.338461538461538,-0.323076923076923,
-0.307692307692308,-0.292307692307692,-0.276923076923077,-0.261538461538462,
-0.246153846153846,-0.230769230769231,-0.215384615384615,-0.2,-0.184615384615385,
-0.169230769230769,-0.153846153846154,-0.138461538461538,-0.123076923076923,
-0.107692307692308,-0.0923076923076923,-0.0769230769230769,-0.0615384615384615,
-0.0461538461538462,-0.0307692307692308,-0.0153846153846154,0.),
 .UNSPECIFIED.)
CURVE()
GEOMETRIC_REPRESENTATION_ITEM()
RATIONAL_B_SPLINE_CURVE((1.,1.,1.,1.,1.,1.,1.,1.,1.,1.,1.,1.,1.,1.,1.,1.,
1.,1.,1.,1.,1.,1.,1.,1.,1.,1.,1.,1.,1.,1.,1.,1.,1.,1.,1.,1.,1.,1.,1.,1.,
1.,1.,1.,1.,1.,1.,1.,1.,1.,1.,1.,1.,1.,1.,1.,1.,1.,1.,1.,1.,1.,1.,1.,1.,
1.,1.,1.,1.,1.,1.))
REPRESENTATION_ITEM('')
);
#343=(
BOUNDED_CURVE()
B_SPLINE_CURVE(5,(#47639,#47640,#47641,#47642,#47643,#47644,#47645,#47646,
#47647,#47648,#47649,#47650,#47651,#47652,#47653,#47654,#47655,#47656,#47657,
#47658,#47659,#47660,#47661,#47662,#47663,#47664,#47665,#47666,#47667,#47668,
#47669,#47670,#47671,#47672,#47673,#47674,#47675,#47676,#47677,#47678,#47679,
#47680,#47681,#47682,#47683,#47684,#47685,#47686,#47687,#47688,#47689,#47690,
#47691,#47692,#47693,#47694,#47695,#47696,#47697,#47698,#47699,#47700,#47701,
#47702,#47703,#47704,#47705,#47706,#47707,#47708),.UNSPECIFIED.,.F.,.F.)
B_SPLINE_CURVE_WITH_KNOTS((6,1,1,1,1,1,1,1,1,1,1,1,1,1,1,1,1,1,1,1,1,1,
1,1,1,1,1,1,1,1,1,1,1,1,1,1,1,1,1,1,1,1,1,1,1,1,1,1,1,1,1,1,1,1,1,1,1,1,
1,1,1,1,1,1,1,6),(-1.,-0.984615384615383,-0.969230769230768,-0.953846153846152,
-0.938461538461537,-0.923076923076922,-0.907692307692306,-0.892307692307691,
-0.876923076923076,-0.86153846153846,-0.846153846153845,-0.83076923076923,
-0.815384615384614,-0.799999999999999,-0.784615384615384,-0.769230769230768,
-0.753846153846153,-0.738461538461538,-0.723076923076922,-0.707692307692307,
-0.692307692307692,-0.676923076923076,-0.661538461538461,-0.646153846153846,
-0.63076923076923,-0.615384615384615,-0.6,-0.584615384615384,-0.569230769230769,
-0.553846153846154,-0.538461538461538,-0.523076923076923,-0.507692307692308,
-0.492307692307692,-0.476923076923077,-0.461538461538462,-0.446153846153846,
-0.430769230769231,-0.415384615384615,-0.4,-0.384615384615385,-0.369230769230769,
-0.353846153846154,-0.338461538461538,-0.323076923076923,-0.307692307692308,
-0.292307692307692,-0.276923076923077,-0.261538461538462,-0.246153846153846,
-0.230769230769231,-0.215384615384615,-0.2,-0.184615384615385,-0.169230769230769,
-0.153846153846154,-0.138461538461538,-0.123076923076923,-0.107692307692308,
-0.0923076923076923,-0.0769230769230769,-0.0615384615384615,-0.0461538461538462,
-0.0307692307692308,-0.0153846153846154,-0.00577184337450876),
 .UNSPECIFIED.)
CURVE()
GEOMETRIC_REPRESENTATION_ITEM()
RATIONAL_B_SPLINE_CURVE((1.,1.,1.,1.,1.,1.,1.,1.,1.,1.,1.,1.,1.,1.,1.,1.,
1.,1.,1.,1.,1.,1.,1.,1.,1.,1.,1.,1.,1.,1.,1.,1.,1.,1.,1.,1.,1.,1.,1.,1.,
1.,1.,1.,1.,1.,1.,1.,1.,1.,1.,1.,1.,1.,1.,1.,1.,1.,1.,1.,1.,1.,1.,1.,1.,
1.,1.,1.,1.,1.,1.))
REPRESENTATION_ITEM('')
);
#344=(
BOUNDED_CURVE()
B_SPLINE_CURVE(5,(#47859,#47860,#47861,#47862,#47863,#47864,#47865,#47866,
#47867,#47868,#47869,#47870,#47871,#47872,#47873,#47874,#47875,#47876,#47877,
#47878,#47879,#47880,#47881,#47882,#47883,#47884,#47885,#47886,#47887,#47888,
#47889,#47890,#47891,#47892,#47893,#47894,#47895,#47896,#47897,#47898,#47899,
#47900,#47901,#47902,#47903,#47904,#47905,#47906,#47907,#47908,#47909,#47910,
#47911,#47912,#47913,#47914,#47915,#47916,#47917,#47918,#47919,#47920,#47921,
#47922,#47923,#47924,#47925,#47926,#47927,#47928),.UNSPECIFIED.,.F.,.F.)
B_SPLINE_CURVE_WITH_KNOTS((6,1,1,1,1,1,1,1,1,1,1,1,1,1,1,1,1,1,1,1,1,1,
1,1,1,1,1,1,1,1,1,1,1,1,1,1,1,1,1,1,1,1,1,1,1,1,1,1,1,1,1,1,1,1,1,1,1,1,
1,1,1,1,1,1,1,6),(-0.99422815673966,-0.984615384615383,-0.969230769230768,
-0.953846153846152,-0.938461538461537,-0.923076923076922,-0.907692307692306,
-0.892307692307691,-0.876923076923076,-0.86153846153846,-0.846153846153845,
-0.83076923076923,-0.815384615384614,-0.799999999999999,-0.784615384615384,
-0.769230769230768,-0.753846153846153,-0.738461538461538,-0.723076923076922,
-0.707692307692307,-0.692307692307692,-0.676923076923076,-0.661538461538461,
-0.646153846153846,-0.63076923076923,-0.615384615384615,-0.6,-0.584615384615384,
-0.569230769230769,-0.553846153846154,-0.538461538461538,-0.523076923076923,
-0.507692307692308,-0.492307692307692,-0.476923076923077,-0.461538461538462,
-0.446153846153846,-0.430769230769231,-0.415384615384615,-0.4,-0.384615384615385,
-0.369230769230769,-0.353846153846154,-0.338461538461538,-0.323076923076923,
-0.307692307692308,-0.292307692307692,-0.276923076923077,-0.261538461538462,
-0.246153846153846,-0.230769230769231,-0.215384615384615,-0.2,-0.184615384615385,
-0.169230769230769,-0.153846153846154,-0.138461538461538,-0.123076923076923,
-0.107692307692308,-0.0923076923076923,-0.0769230769230769,-0.0615384615384615,
-0.0461538461538462,-0.0307692307692308,-0.0153846153846154,0.),
 .UNSPECIFIED.)
CURVE()
GEOMETRIC_REPRESENTATION_ITEM()
RATIONAL_B_SPLINE_CURVE((1.,1.,1.,1.,1.,1.,1.,1.,1.,1.,1.,1.,1.,1.,1.,1.,
1.,1.,1.,1.,1.,1.,1.,1.,1.,1.,1.,1.,1.,1.,1.,1.,1.,1.,1.,1.,1.,1.,1.,1.,
1.,1.,1.,1.,1.,1.,1.,1.,1.,1.,1.,1.,1.,1.,1.,1.,1.,1.,1.,1.,1.,1.,1.,1.,
1.,1.,1.,1.,1.,1.))
REPRESENTATION_ITEM('')
);
#345=(
BOUNDED_CURVE()
B_SPLINE_CURVE(5,(#48081,#48082,#48083,#48084,#48085,#48086,#48087,#48088,
#48089,#48090,#48091,#48092,#48093,#48094,#48095,#48096,#48097,#48098,#48099,
#48100,#48101,#48102,#48103,#48104,#48105,#48106,#48107,#48108,#48109,#48110,
#48111,#48112,#48113,#48114,#48115,#48116,#48117,#48118,#48119,#48120,#48121,
#48122,#48123,#48124,#48125,#48126,#48127,#48128,#48129,#48130,#48131,#48132,
#48133,#48134,#48135,#48136,#48137,#48138,#48139,#48140,#48141,#48142,#48143,
#48144,#48145,#48146,#48147,#48148,#48149,#48150),.UNSPECIFIED.,.F.,.F.)
B_SPLINE_CURVE_WITH_KNOTS((6,1,1,1,1,1,1,1,1,1,1,1,1,1,1,1,1,1,1,1,1,1,
1,1,1,1,1,1,1,1,1,1,1,1,1,1,1,1,1,1,1,1,1,1,1,1,1,1,1,1,1,1,1,1,1,1,1,1,
1,1,1,1,1,1,1,6),(-1.,-0.984615384615383,-0.969230769230768,-0.953846153846152,
-0.938461538461537,-0.923076923076922,-0.907692307692306,-0.892307692307691,
-0.876923076923076,-0.86153846153846,-0.846153846153845,-0.83076923076923,
-0.815384615384614,-0.799999999999999,-0.784615384615384,-0.769230769230768,
-0.753846153846153,-0.738461538461538,-0.723076923076922,-0.707692307692307,
-0.692307692307692,-0.676923076923076,-0.661538461538461,-0.646153846153846,
-0.63076923076923,-0.615384615384615,-0.6,-0.584615384615384,-0.569230769230769,
-0.553846153846154,-0.538461538461538,-0.523076923076923,-0.507692307692308,
-0.492307692307692,-0.476923076923077,-0.461538461538462,-0.446153846153846,
-0.430769230769231,-0.415384615384615,-0.4,-0.384615384615385,-0.369230769230769,
-0.353846153846154,-0.338461538461538,-0.323076923076923,-0.307692307692308,
-0.292307692307692,-0.276923076923077,-0.261538461538462,-0.246153846153846,
-0.230769230769231,-0.215384615384615,-0.2,-0.184615384615385,-0.169230769230769,
-0.153846153846154,-0.138461538461538,-0.123076923076923,-0.107692307692308,
-0.0923076923076923,-0.0769230769230769,-0.0615384615384615,-0.0461538461538462,
-0.0307692307692308,-0.0153846153846154,-0.00577184337451051),
 .UNSPECIFIED.)
CURVE()
GEOMETRIC_REPRESENTATION_ITEM()
RATIONAL_B_SPLINE_CURVE((1.,1.,1.,1.,1.,1.,1.,1.,1.,1.,1.,1.,1.,1.,1.,1.,
1.,1.,1.,1.,1.,1.,1.,1.,1.,1.,1.,1.,1.,1.,1.,1.,1.,1.,1.,1.,1.,1.,1.,1.,
1.,1.,1.,1.,1.,1.,1.,1.,1.,1.,1.,1.,1.,1.,1.,1.,1.,1.,1.,1.,1.,1.,1.,1.,
1.,1.,1.,1.,1.,1.))
REPRESENTATION_ITEM('')
);
#346=(
BOUNDED_CURVE()
B_SPLINE_CURVE(5,(#48301,#48302,#48303,#48304,#48305,#48306,#48307,#48308,
#48309,#48310,#48311,#48312,#48313,#48314,#48315,#48316,#48317,#48318,#48319,
#48320,#48321,#48322,#48323,#48324,#48325,#48326,#48327,#48328,#48329,#48330,
#48331,#48332,#48333,#48334,#48335,#48336,#48337,#48338,#48339,#48340,#48341,
#48342,#48343,#48344,#48345,#48346,#48347,#48348,#48349,#48350,#48351,#48352,
#48353,#48354,#48355,#48356,#48357,#48358,#48359,#48360,#48361,#48362,#48363,
#48364,#48365,#48366,#48367,#48368,#48369,#48370),.UNSPECIFIED.,.F.,.F.)
B_SPLINE_CURVE_WITH_KNOTS((6,1,1,1,1,1,1,1,1,1,1,1,1,1,1,1,1,1,1,1,1,1,
1,1,1,1,1,1,1,1,1,1,1,1,1,1,1,1,1,1,1,1,1,1,1,1,1,1,1,1,1,1,1,1,1,1,1,1,
1,1,1,1,1,1,1,6),(-0.994228156739678,-0.984615384615383,-0.969230769230768,
-0.953846153846152,-0.938461538461537,-0.923076923076922,-0.907692307692306,
-0.892307692307691,-0.876923076923076,-0.86153846153846,-0.846153846153845,
-0.83076923076923,-0.815384615384614,-0.799999999999999,-0.784615384615384,
-0.769230769230768,-0.753846153846153,-0.738461538461538,-0.723076923076922,
-0.707692307692307,-0.692307692307692,-0.676923076923076,-0.661538461538461,
-0.646153846153846,-0.63076923076923,-0.615384615384615,-0.6,-0.584615384615384,
-0.569230769230769,-0.553846153846154,-0.538461538461538,-0.523076923076923,
-0.507692307692308,-0.492307692307692,-0.476923076923077,-0.461538461538462,
-0.446153846153846,-0.430769230769231,-0.415384615384615,-0.4,-0.384615384615385,
-0.369230769230769,-0.353846153846154,-0.338461538461538,-0.323076923076923,
-0.307692307692308,-0.292307692307692,-0.276923076923077,-0.261538461538462,
-0.246153846153846,-0.230769230769231,-0.215384615384615,-0.2,-0.184615384615385,
-0.169230769230769,-0.153846153846154,-0.138461538461538,-0.123076923076923,
-0.107692307692308,-0.0923076923076923,-0.0769230769230769,-0.0615384615384615,
-0.0461538461538462,-0.0307692307692308,-0.0153846153846154,0.),
 .UNSPECIFIED.)
CURVE()
GEOMETRIC_REPRESENTATION_ITEM()
RATIONAL_B_SPLINE_CURVE((1.,1.,1.,1.,1.,1.,1.,1.,1.,1.,1.,1.,1.,1.,1.,1.,
1.,1.,1.,1.,1.,1.,1.,1.,1.,1.,1.,1.,1.,1.,1.,1.,1.,1.,1.,1.,1.,1.,1.,1.,
1.,1.,1.,1.,1.,1.,1.,1.,1.,1.,1.,1.,1.,1.,1.,1.,1.,1.,1.,1.,1.,1.,1.,1.,
1.,1.,1.,1.,1.,1.))
REPRESENTATION_ITEM('')
);
#347=(
BOUNDED_CURVE()
B_SPLINE_CURVE(5,(#48523,#48524,#48525,#48526,#48527,#48528,#48529,#48530,
#48531,#48532,#48533,#48534,#48535,#48536,#48537,#48538,#48539,#48540,#48541,
#48542,#48543,#48544,#48545,#48546,#48547,#48548,#48549,#48550,#48551,#48552,
#48553,#48554,#48555,#48556,#48557,#48558,#48559,#48560,#48561,#48562,#48563,
#48564,#48565,#48566,#48567,#48568,#48569,#48570,#48571,#48572,#48573,#48574,
#48575,#48576,#48577,#48578,#48579,#48580,#48581,#48582,#48583,#48584,#48585,
#48586,#48587,#48588,#48589,#48590,#48591,#48592),.UNSPECIFIED.,.F.,.F.)
B_SPLINE_CURVE_WITH_KNOTS((6,1,1,1,1,1,1,1,1,1,1,1,1,1,1,1,1,1,1,1,1,1,
1,1,1,1,1,1,1,1,1,1,1,1,1,1,1,1,1,1,1,1,1,1,1,1,1,1,1,1,1,1,1,1,1,1,1,1,
1,1,1,1,1,1,1,6),(-1.,-0.984615384615383,-0.969230769230768,-0.953846153846152,
-0.938461538461537,-0.923076923076922,-0.907692307692306,-0.892307692307691,
-0.876923076923076,-0.86153846153846,-0.846153846153845,-0.83076923076923,
-0.815384615384614,-0.799999999999999,-0.784615384615384,-0.769230769230768,
-0.753846153846153,-0.738461538461538,-0.723076923076922,-0.707692307692307,
-0.692307692307692,-0.676923076923076,-0.661538461538461,-0.646153846153846,
-0.63076923076923,-0.615384615384615,-0.6,-0.584615384615384,-0.569230769230769,
-0.553846153846154,-0.538461538461538,-0.523076923076923,-0.507692307692308,
-0.492307692307692,-0.476923076923077,-0.461538461538462,-0.446153846153846,
-0.430769230769231,-0.415384615384615,-0.4,-0.384615384615385,-0.369230769230769,
-0.353846153846154,-0.338461538461538,-0.323076923076923,-0.307692307692308,
-0.292307692307692,-0.276923076923077,-0.261538461538462,-0.246153846153846,
-0.230769230769231,-0.215384615384615,-0.2,-0.184615384615385,-0.169230769230769,
-0.153846153846154,-0.138461538461538,-0.123076923076923,-0.107692307692308,
-0.0923076923076923,-0.0769230769230769,-0.0615384615384615,-0.0461538461538462,
-0.0307692307692308,-0.0153846153846154,-0.0057718433745179),
 .UNSPECIFIED.)
CURVE()
GEOMETRIC_REPRESENTATION_ITEM()
RATIONAL_B_SPLINE_CURVE((1.,1.,1.,1.,1.,1.,1.,1.,1.,1.,1.,1.,1.,1.,1.,1.,
1.,1.,1.,1.,1.,1.,1.,1.,1.,1.,1.,1.,1.,1.,1.,1.,1.,1.,1.,1.,1.,1.,1.,1.,
1.,1.,1.,1.,1.,1.,1.,1.,1.,1.,1.,1.,1.,1.,1.,1.,1.,1.,1.,1.,1.,1.,1.,1.,
1.,1.,1.,1.,1.,1.))
REPRESENTATION_ITEM('')
);
#348=(
BOUNDED_CURVE()
B_SPLINE_CURVE(5,(#48743,#48744,#48745,#48746,#48747,#48748,#48749,#48750,
#48751,#48752,#48753,#48754,#48755,#48756,#48757,#48758,#48759,#48760,#48761,
#48762,#48763,#48764,#48765,#48766,#48767,#48768,#48769,#48770,#48771,#48772,
#48773,#48774,#48775,#48776,#48777,#48778,#48779,#48780,#48781,#48782,#48783,
#48784,#48785,#48786,#48787,#48788,#48789,#48790,#48791,#48792,#48793,#48794,
#48795,#48796,#48797,#48798,#48799,#48800,#48801,#48802,#48803,#48804,#48805,
#48806,#48807,#48808,#48809,#48810,#48811,#48812),.UNSPECIFIED.,.F.,.F.)
B_SPLINE_CURVE_WITH_KNOTS((6,1,1,1,1,1,1,1,1,1,1,1,1,1,1,1,1,1,1,1,1,1,
1,1,1,1,1,1,1,1,1,1,1,1,1,1,1,1,1,1,1,1,1,1,1,1,1,1,1,1,1,1,1,1,1,1,1,1,
1,1,1,1,1,1,1,6),(-0.99422815673967,-0.984615384615383,-0.969230769230768,
-0.953846153846152,-0.938461538461537,-0.923076923076922,-0.907692307692306,
-0.892307692307691,-0.876923076923076,-0.86153846153846,-0.846153846153845,
-0.83076923076923,-0.815384615384614,-0.799999999999999,-0.784615384615384,
-0.769230769230768,-0.753846153846153,-0.738461538461538,-0.723076923076922,
-0.707692307692307,-0.692307692307692,-0.676923076923076,-0.661538461538461,
-0.646153846153846,-0.63076923076923,-0.615384615384615,-0.6,-0.584615384615384,
-0.569230769230769,-0.553846153846154,-0.538461538461538,-0.523076923076923,
-0.507692307692308,-0.492307692307692,-0.476923076923077,-0.461538461538462,
-0.446153846153846,-0.430769230769231,-0.415384615384615,-0.4,-0.384615384615385,
-0.369230769230769,-0.353846153846154,-0.338461538461538,-0.323076923076923,
-0.307692307692308,-0.292307692307692,-0.276923076923077,-0.261538461538462,
-0.246153846153846,-0.230769230769231,-0.215384615384615,-0.2,-0.184615384615385,
-0.169230769230769,-0.153846153846154,-0.138461538461538,-0.123076923076923,
-0.107692307692308,-0.0923076923076923,-0.0769230769230769,-0.0615384615384615,
-0.0461538461538462,-0.0307692307692308,-0.0153846153846154,0.),
 .UNSPECIFIED.)
CURVE()
GEOMETRIC_REPRESENTATION_ITEM()
RATIONAL_B_SPLINE_CURVE((1.,1.,1.,1.,1.,1.,1.,1.,1.,1.,1.,1.,1.,1.,1.,1.,
1.,1.,1.,1.,1.,1.,1.,1.,1.,1.,1.,1.,1.,1.,1.,1.,1.,1.,1.,1.,1.,1.,1.,1.,
1.,1.,1.,1.,1.,1.,1.,1.,1.,1.,1.,1.,1.,1.,1.,1.,1.,1.,1.,1.,1.,1.,1.,1.,
1.,1.,1.,1.,1.,1.))
REPRESENTATION_ITEM('')
);
#349=(
BOUNDED_CURVE()
B_SPLINE_CURVE(5,(#48965,#48966,#48967,#48968,#48969,#48970,#48971,#48972,
#48973,#48974,#48975,#48976,#48977,#48978,#48979,#48980,#48981,#48982,#48983,
#48984,#48985,#48986,#48987,#48988,#48989,#48990,#48991,#48992,#48993,#48994,
#48995,#48996,#48997,#48998,#48999,#49000,#49001,#49002,#49003,#49004,#49005,
#49006,#49007,#49008,#49009,#49010,#49011,#49012,#49013,#49014,#49015,#49016,
#49017,#49018,#49019,#49020,#49021,#49022,#49023,#49024,#49025,#49026,#49027,
#49028,#49029,#49030,#49031,#49032,#49033,#49034),.UNSPECIFIED.,.F.,.F.)
B_SPLINE_CURVE_WITH_KNOTS((6,1,1,1,1,1,1,1,1,1,1,1,1,1,1,1,1,1,1,1,1,1,
1,1,1,1,1,1,1,1,1,1,1,1,1,1,1,1,1,1,1,1,1,1,1,1,1,1,1,1,1,1,1,1,1,1,1,1,
1,1,1,1,1,1,1,6),(-1.,-0.984615384615383,-0.969230769230768,-0.953846153846152,
-0.938461538461537,-0.923076923076922,-0.907692307692306,-0.892307692307691,
-0.876923076923076,-0.86153846153846,-0.846153846153845,-0.83076923076923,
-0.815384615384614,-0.799999999999999,-0.784615384615384,-0.769230769230768,
-0.753846153846153,-0.738461538461538,-0.723076923076922,-0.707692307692307,
-0.692307692307692,-0.676923076923076,-0.661538461538461,-0.646153846153846,
-0.63076923076923,-0.615384615384615,-0.6,-0.584615384615384,-0.569230769230769,
-0.553846153846154,-0.538461538461538,-0.523076923076923,-0.507692307692308,
-0.492307692307692,-0.476923076923077,-0.461538461538462,-0.446153846153846,
-0.430769230769231,-0.415384615384615,-0.4,-0.384615384615385,-0.369230769230769,
-0.353846153846154,-0.338461538461538,-0.323076923076923,-0.307692307692308,
-0.292307692307692,-0.276923076923077,-0.261538461538462,-0.246153846153846,
-0.230769230769231,-0.215384615384615,-0.2,-0.184615384615385,-0.169230769230769,
-0.153846153846154,-0.138461538461538,-0.123076923076923,-0.107692307692308,
-0.0923076923076923,-0.0769230769230769,-0.0615384615384615,-0.0461538461538462,
-0.0307692307692308,-0.0153846153846154,-0.00577184337452479),
 .UNSPECIFIED.)
CURVE()
GEOMETRIC_REPRESENTATION_ITEM()
RATIONAL_B_SPLINE_CURVE((1.,1.,1.,1.,1.,1.,1.,1.,1.,1.,1.,1.,1.,1.,1.,1.,
1.,1.,1.,1.,1.,1.,1.,1.,1.,1.,1.,1.,1.,1.,1.,1.,1.,1.,1.,1.,1.,1.,1.,1.,
1.,1.,1.,1.,1.,1.,1.,1.,1.,1.,1.,1.,1.,1.,1.,1.,1.,1.,1.,1.,1.,1.,1.,1.,
1.,1.,1.,1.,1.,1.))
REPRESENTATION_ITEM('')
);
#350=(
BOUNDED_CURVE()
B_SPLINE_CURVE(5,(#49185,#49186,#49187,#49188,#49189,#49190,#49191,#49192,
#49193,#49194,#49195,#49196,#49197,#49198,#49199,#49200,#49201,#49202,#49203,
#49204,#49205,#49206,#49207,#49208,#49209,#49210,#49211,#49212,#49213,#49214,
#49215,#49216,#49217,#49218,#49219,#49220,#49221,#49222,#49223,#49224,#49225,
#49226,#49227,#49228,#49229,#49230,#49231,#49232,#49233,#49234,#49235,#49236,
#49237,#49238,#49239,#49240,#49241,#49242,#49243,#49244,#49245,#49246,#49247,
#49248,#49249,#49250,#49251,#49252,#49253,#49254),.UNSPECIFIED.,.F.,.F.)
B_SPLINE_CURVE_WITH_KNOTS((6,1,1,1,1,1,1,1,1,1,1,1,1,1,1,1,1,1,1,1,1,1,
1,1,1,1,1,1,1,1,1,1,1,1,1,1,1,1,1,1,1,1,1,1,1,1,1,1,1,1,1,1,1,1,1,1,1,1,
1,1,1,1,1,1,1,6),(-0.99422815673967,-0.984615384615383,-0.969230769230768,
-0.953846153846152,-0.938461538461537,-0.923076923076922,-0.907692307692306,
-0.892307692307691,-0.876923076923076,-0.86153846153846,-0.846153846153845,
-0.83076923076923,-0.815384615384614,-0.799999999999999,-0.784615384615384,
-0.769230769230768,-0.753846153846153,-0.738461538461538,-0.723076923076922,
-0.707692307692307,-0.692307692307692,-0.676923076923076,-0.661538461538461,
-0.646153846153846,-0.63076923076923,-0.615384615384615,-0.6,-0.584615384615384,
-0.569230769230769,-0.553846153846154,-0.538461538461538,-0.523076923076923,
-0.507692307692308,-0.492307692307692,-0.476923076923077,-0.461538461538462,
-0.446153846153846,-0.430769230769231,-0.415384615384615,-0.4,-0.384615384615385,
-0.369230769230769,-0.353846153846154,-0.338461538461538,-0.323076923076923,
-0.307692307692308,-0.292307692307692,-0.276923076923077,-0.261538461538462,
-0.246153846153846,-0.230769230769231,-0.215384615384615,-0.2,-0.184615384615385,
-0.169230769230769,-0.153846153846154,-0.138461538461538,-0.123076923076923,
-0.107692307692308,-0.0923076923076923,-0.0769230769230769,-0.0615384615384615,
-0.0461538461538462,-0.0307692307692308,-0.0153846153846154,0.),
 .UNSPECIFIED.)
CURVE()
GEOMETRIC_REPRESENTATION_ITEM()
RATIONAL_B_SPLINE_CURVE((1.,1.,1.,1.,1.,1.,1.,1.,1.,1.,1.,1.,1.,1.,1.,1.,
1.,1.,1.,1.,1.,1.,1.,1.,1.,1.,1.,1.,1.,1.,1.,1.,1.,1.,1.,1.,1.,1.,1.,1.,
1.,1.,1.,1.,1.,1.,1.,1.,1.,1.,1.,1.,1.,1.,1.,1.,1.,1.,1.,1.,1.,1.,1.,1.,
1.,1.,1.,1.,1.,1.))
REPRESENTATION_ITEM('')
);
#351=(
BOUNDED_CURVE()
B_SPLINE_CURVE(5,(#49407,#49408,#49409,#49410,#49411,#49412,#49413,#49414,
#49415,#49416,#49417,#49418,#49419,#49420,#49421,#49422,#49423,#49424,#49425,
#49426,#49427,#49428,#49429,#49430,#49431,#49432,#49433,#49434,#49435,#49436,
#49437,#49438,#49439,#49440,#49441,#49442,#49443,#49444,#49445,#49446,#49447,
#49448,#49449,#49450,#49451,#49452,#49453,#49454,#49455,#49456,#49457,#49458,
#49459,#49460,#49461,#49462,#49463,#49464,#49465,#49466,#49467,#49468,#49469,
#49470,#49471,#49472,#49473,#49474,#49475,#49476),.UNSPECIFIED.,.F.,.F.)
B_SPLINE_CURVE_WITH_KNOTS((6,1,1,1,1,1,1,1,1,1,1,1,1,1,1,1,1,1,1,1,1,1,
1,1,1,1,1,1,1,1,1,1,1,1,1,1,1,1,1,1,1,1,1,1,1,1,1,1,1,1,1,1,1,1,1,1,1,1,
1,1,1,1,1,1,1,6),(-1.,-0.984615384615383,-0.969230769230768,-0.953846153846152,
-0.938461538461537,-0.923076923076922,-0.907692307692306,-0.892307692307691,
-0.876923076923076,-0.86153846153846,-0.846153846153845,-0.83076923076923,
-0.815384615384614,-0.799999999999999,-0.784615384615384,-0.769230769230768,
-0.753846153846153,-0.738461538461538,-0.723076923076922,-0.707692307692307,
-0.692307692307692,-0.676923076923076,-0.661538461538461,-0.646153846153846,
-0.63076923076923,-0.615384615384615,-0.6,-0.584615384615384,-0.569230769230769,
-0.553846153846154,-0.538461538461538,-0.523076923076923,-0.507692307692308,
-0.492307692307692,-0.476923076923077,-0.461538461538462,-0.446153846153846,
-0.430769230769231,-0.415384615384615,-0.4,-0.384615384615385,-0.369230769230769,
-0.353846153846154,-0.338461538461538,-0.323076923076923,-0.307692307692308,
-0.292307692307692,-0.276923076923077,-0.261538461538462,-0.246153846153846,
-0.230769230769231,-0.215384615384615,-0.2,-0.184615384615385,-0.169230769230769,
-0.153846153846154,-0.138461538461538,-0.123076923076923,-0.107692307692308,
-0.0923076923076923,-0.0769230769230769,-0.0615384615384615,-0.0461538461538462,
-0.0307692307692308,-0.0153846153846154,-0.0057718433745009),
 .UNSPECIFIED.)
CURVE()
GEOMETRIC_REPRESENTATION_ITEM()
RATIONAL_B_SPLINE_CURVE((1.,1.,1.,1.,1.,1.,1.,1.,1.,1.,1.,1.,1.,1.,1.,1.,
1.,1.,1.,1.,1.,1.,1.,1.,1.,1.,1.,1.,1.,1.,1.,1.,1.,1.,1.,1.,1.,1.,1.,1.,
1.,1.,1.,1.,1.,1.,1.,1.,1.,1.,1.,1.,1.,1.,1.,1.,1.,1.,1.,1.,1.,1.,1.,1.,
1.,1.,1.,1.,1.,1.))
REPRESENTATION_ITEM('')
);
#352=(
BOUNDED_CURVE()
B_SPLINE_CURVE(5,(#49627,#49628,#49629,#49630,#49631,#49632,#49633,#49634,
#49635,#49636,#49637,#49638,#49639,#49640,#49641,#49642,#49643,#49644,#49645,
#49646,#49647,#49648,#49649,#49650,#49651,#49652,#49653,#49654,#49655,#49656,
#49657,#49658,#49659,#49660,#49661,#49662,#49663,#49664,#49665,#49666,#49667,
#49668,#49669,#49670,#49671,#49672,#49673,#49674,#49675,#49676,#49677,#49678,
#49679,#49680,#49681,#49682,#49683,#49684,#49685,#49686,#49687,#49688,#49689,
#49690,#49691,#49692,#49693,#49694,#49695,#49696),.UNSPECIFIED.,.F.,.F.)
B_SPLINE_CURVE_WITH_KNOTS((6,1,1,1,1,1,1,1,1,1,1,1,1,1,1,1,1,1,1,1,1,1,
1,1,1,1,1,1,1,1,1,1,1,1,1,1,1,1,1,1,1,1,1,1,1,1,1,1,1,1,1,1,1,1,1,1,1,1,
1,1,1,1,1,1,1,6),(-0.99422815673967,-0.984615384615383,-0.969230769230768,
-0.953846153846152,-0.938461538461537,-0.923076923076922,-0.907692307692306,
-0.892307692307691,-0.876923076923076,-0.86153846153846,-0.846153846153845,
-0.83076923076923,-0.815384615384614,-0.799999999999999,-0.784615384615384,
-0.769230769230768,-0.753846153846153,-0.738461538461538,-0.723076923076922,
-0.707692307692307,-0.692307692307692,-0.676923076923076,-0.661538461538461,
-0.646153846153846,-0.63076923076923,-0.615384615384615,-0.6,-0.584615384615384,
-0.569230769230769,-0.553846153846154,-0.538461538461538,-0.523076923076923,
-0.507692307692308,-0.492307692307692,-0.476923076923077,-0.461538461538462,
-0.446153846153846,-0.430769230769231,-0.415384615384615,-0.4,-0.384615384615385,
-0.369230769230769,-0.353846153846154,-0.338461538461538,-0.323076923076923,
-0.307692307692308,-0.292307692307692,-0.276923076923077,-0.261538461538462,
-0.246153846153846,-0.230769230769231,-0.215384615384615,-0.2,-0.184615384615385,
-0.169230769230769,-0.153846153846154,-0.138461538461538,-0.123076923076923,
-0.107692307692308,-0.0923076923076923,-0.0769230769230769,-0.0615384615384615,
-0.0461538461538462,-0.0307692307692308,-0.0153846153846154,0.),
 .UNSPECIFIED.)
CURVE()
GEOMETRIC_REPRESENTATION_ITEM()
RATIONAL_B_SPLINE_CURVE((1.,1.,1.,1.,1.,1.,1.,1.,1.,1.,1.,1.,1.,1.,1.,1.,
1.,1.,1.,1.,1.,1.,1.,1.,1.,1.,1.,1.,1.,1.,1.,1.,1.,1.,1.,1.,1.,1.,1.,1.,
1.,1.,1.,1.,1.,1.,1.,1.,1.,1.,1.,1.,1.,1.,1.,1.,1.,1.,1.,1.,1.,1.,1.,1.,
1.,1.,1.,1.,1.,1.))
REPRESENTATION_ITEM('')
);
#353=(
BOUNDED_CURVE()
B_SPLINE_CURVE(5,(#49849,#49850,#49851,#49852,#49853,#49854,#49855,#49856,
#49857,#49858,#49859,#49860,#49861,#49862,#49863,#49864,#49865,#49866,#49867,
#49868,#49869,#49870,#49871,#49872,#49873,#49874,#49875,#49876,#49877,#49878,
#49879,#49880,#49881,#49882,#49883,#49884,#49885,#49886,#49887,#49888,#49889,
#49890,#49891,#49892,#49893,#49894,#49895,#49896,#49897,#49898,#49899,#49900,
#49901,#49902,#49903,#49904,#49905,#49906,#49907,#49908,#49909,#49910,#49911,
#49912,#49913,#49914,#49915,#49916,#49917,#49918),.UNSPECIFIED.,.F.,.F.)
B_SPLINE_CURVE_WITH_KNOTS((6,1,1,1,1,1,1,1,1,1,1,1,1,1,1,1,1,1,1,1,1,1,
1,1,1,1,1,1,1,1,1,1,1,1,1,1,1,1,1,1,1,1,1,1,1,1,1,1,1,1,1,1,1,1,1,1,1,1,
1,1,1,1,1,1,1,6),(-1.,-0.984615384615383,-0.969230769230768,-0.953846153846152,
-0.938461538461537,-0.923076923076922,-0.907692307692306,-0.892307692307691,
-0.876923076923076,-0.86153846153846,-0.846153846153845,-0.83076923076923,
-0.815384615384614,-0.799999999999999,-0.784615384615384,-0.769230769230768,
-0.753846153846153,-0.738461538461538,-0.723076923076922,-0.707692307692307,
-0.692307692307692,-0.676923076923076,-0.661538461538461,-0.646153846153846,
-0.63076923076923,-0.615384615384615,-0.6,-0.584615384615384,-0.569230769230769,
-0.553846153846154,-0.538461538461538,-0.523076923076923,-0.507692307692308,
-0.492307692307692,-0.476923076923077,-0.461538461538462,-0.446153846153846,
-0.430769230769231,-0.415384615384615,-0.4,-0.384615384615385,-0.369230769230769,
-0.353846153846154,-0.338461538461538,-0.323076923076923,-0.307692307692308,
-0.292307692307692,-0.276923076923077,-0.261538461538462,-0.246153846153846,
-0.230769230769231,-0.215384615384615,-0.2,-0.184615384615385,-0.169230769230769,
-0.153846153846154,-0.138461538461538,-0.123076923076923,-0.107692307692308,
-0.0923076923076923,-0.0769230769230769,-0.0615384615384615,-0.0461538461538462,
-0.0307692307692308,-0.0153846153846154,-0.00577184337450701),
 .UNSPECIFIED.)
CURVE()
GEOMETRIC_REPRESENTATION_ITEM()
RATIONAL_B_SPLINE_CURVE((1.,1.,1.,1.,1.,1.,1.,1.,1.,1.,1.,1.,1.,1.,1.,1.,
1.,1.,1.,1.,1.,1.,1.,1.,1.,1.,1.,1.,1.,1.,1.,1.,1.,1.,1.,1.,1.,1.,1.,1.,
1.,1.,1.,1.,1.,1.,1.,1.,1.,1.,1.,1.,1.,1.,1.,1.,1.,1.,1.,1.,1.,1.,1.,1.,
1.,1.,1.,1.,1.,1.))
REPRESENTATION_ITEM('')
);
#354=(
BOUNDED_CURVE()
B_SPLINE_CURVE(5,(#50069,#50070,#50071,#50072,#50073,#50074,#50075,#50076,
#50077,#50078,#50079,#50080,#50081,#50082,#50083,#50084,#50085,#50086,#50087,
#50088,#50089,#50090,#50091,#50092,#50093,#50094,#50095,#50096,#50097,#50098,
#50099,#50100,#50101,#50102,#50103,#50104,#50105,#50106,#50107,#50108,#50109,
#50110,#50111,#50112,#50113,#50114,#50115,#50116,#50117,#50118,#50119,#50120,
#50121,#50122,#50123,#50124,#50125,#50126,#50127,#50128,#50129,#50130,#50131,
#50132,#50133,#50134,#50135,#50136,#50137,#50138),.UNSPECIFIED.,.F.,.F.)
B_SPLINE_CURVE_WITH_KNOTS((6,1,1,1,1,1,1,1,1,1,1,1,1,1,1,1,1,1,1,1,1,1,
1,1,1,1,1,1,1,1,1,1,1,1,1,1,1,1,1,1,1,1,1,1,1,1,1,1,1,1,1,1,1,1,1,1,1,1,
1,1,1,1,1,1,1,6),(-0.994228156739689,-0.984615384615383,-0.969230769230768,
-0.953846153846152,-0.938461538461537,-0.923076923076922,-0.907692307692306,
-0.892307692307691,-0.876923076923076,-0.86153846153846,-0.846153846153845,
-0.83076923076923,-0.815384615384614,-0.799999999999999,-0.784615384615384,
-0.769230769230768,-0.753846153846153,-0.738461538461538,-0.723076923076922,
-0.707692307692307,-0.692307692307692,-0.676923076923076,-0.661538461538461,
-0.646153846153846,-0.63076923076923,-0.615384615384615,-0.6,-0.584615384615384,
-0.569230769230769,-0.553846153846154,-0.538461538461538,-0.523076923076923,
-0.507692307692308,-0.492307692307692,-0.476923076923077,-0.461538461538462,
-0.446153846153846,-0.430769230769231,-0.415384615384615,-0.4,-0.384615384615385,
-0.369230769230769,-0.353846153846154,-0.338461538461538,-0.323076923076923,
-0.307692307692308,-0.292307692307692,-0.276923076923077,-0.261538461538462,
-0.246153846153846,-0.230769230769231,-0.215384615384615,-0.2,-0.184615384615385,
-0.169230769230769,-0.153846153846154,-0.138461538461538,-0.123076923076923,
-0.107692307692308,-0.0923076923076923,-0.0769230769230769,-0.0615384615384615,
-0.0461538461538462,-0.0307692307692308,-0.0153846153846154,0.),
 .UNSPECIFIED.)
CURVE()
GEOMETRIC_REPRESENTATION_ITEM()
RATIONAL_B_SPLINE_CURVE((1.,1.,1.,1.,1.,1.,1.,1.,1.,1.,1.,1.,1.,1.,1.,1.,
1.,1.,1.,1.,1.,1.,1.,1.,1.,1.,1.,1.,1.,1.,1.,1.,1.,1.,1.,1.,1.,1.,1.,1.,
1.,1.,1.,1.,1.,1.,1.,1.,1.,1.,1.,1.,1.,1.,1.,1.,1.,1.,1.,1.,1.,1.,1.,1.,
1.,1.,1.,1.,1.,1.))
REPRESENTATION_ITEM('')
);
#355=(
BOUNDED_CURVE()
B_SPLINE_CURVE(5,(#50291,#50292,#50293,#50294,#50295,#50296,#50297,#50298,
#50299,#50300,#50301,#50302,#50303,#50304,#50305,#50306,#50307,#50308,#50309,
#50310,#50311,#50312,#50313,#50314,#50315,#50316,#50317,#50318,#50319,#50320,
#50321,#50322,#50323,#50324,#50325,#50326,#50327,#50328,#50329,#50330,#50331,
#50332,#50333,#50334,#50335,#50336,#50337,#50338,#50339,#50340,#50341,#50342,
#50343,#50344,#50345,#50346,#50347,#50348,#50349,#50350,#50351,#50352,#50353,
#50354,#50355,#50356,#50357,#50358,#50359,#50360),.UNSPECIFIED.,.F.,.F.)
B_SPLINE_CURVE_WITH_KNOTS((6,1,1,1,1,1,1,1,1,1,1,1,1,1,1,1,1,1,1,1,1,1,
1,1,1,1,1,1,1,1,1,1,1,1,1,1,1,1,1,1,1,1,1,1,1,1,1,1,1,1,1,1,1,1,1,1,1,1,
1,1,1,1,1,1,1,6),(-1.,-0.984615384615383,-0.969230769230768,-0.953846153846152,
-0.938461538461537,-0.923076923076922,-0.907692307692306,-0.892307692307691,
-0.876923076923076,-0.86153846153846,-0.846153846153845,-0.83076923076923,
-0.815384615384614,-0.799999999999999,-0.784615384615384,-0.769230769230768,
-0.753846153846153,-0.738461538461538,-0.723076923076922,-0.707692307692307,
-0.692307692307692,-0.676923076923076,-0.661538461538461,-0.646153846153846,
-0.63076923076923,-0.615384615384615,-0.6,-0.584615384615384,-0.569230769230769,
-0.553846153846154,-0.538461538461538,-0.523076923076923,-0.507692307692308,
-0.492307692307692,-0.476923076923077,-0.461538461538462,-0.446153846153846,
-0.430769230769231,-0.415384615384615,-0.4,-0.384615384615385,-0.369230769230769,
-0.353846153846154,-0.338461538461538,-0.323076923076923,-0.307692307692308,
-0.292307692307692,-0.276923076923077,-0.261538461538462,-0.246153846153846,
-0.230769230769231,-0.215384615384615,-0.2,-0.184615384615385,-0.169230769230769,
-0.153846153846154,-0.138461538461538,-0.123076923076923,-0.107692307692308,
-0.0923076923076923,-0.0769230769230769,-0.0615384615384615,-0.0461538461538462,
-0.0307692307692308,-0.0153846153846154,-0.00577184337452382),
 .UNSPECIFIED.)
CURVE()
GEOMETRIC_REPRESENTATION_ITEM()
RATIONAL_B_SPLINE_CURVE((1.,1.,1.,1.,1.,1.,1.,1.,1.,1.,1.,1.,1.,1.,1.,1.,
1.,1.,1.,1.,1.,1.,1.,1.,1.,1.,1.,1.,1.,1.,1.,1.,1.,1.,1.,1.,1.,1.,1.,1.,
1.,1.,1.,1.,1.,1.,1.,1.,1.,1.,1.,1.,1.,1.,1.,1.,1.,1.,1.,1.,1.,1.,1.,1.,
1.,1.,1.,1.,1.,1.))
REPRESENTATION_ITEM('')
);
#356=(
BOUNDED_CURVE()
B_SPLINE_CURVE(5,(#50511,#50512,#50513,#50514,#50515,#50516,#50517,#50518,
#50519,#50520,#50521,#50522,#50523,#50524,#50525,#50526,#50527,#50528,#50529,
#50530,#50531,#50532,#50533,#50534,#50535,#50536,#50537,#50538,#50539,#50540,
#50541,#50542,#50543,#50544,#50545,#50546,#50547,#50548,#50549,#50550,#50551,
#50552,#50553,#50554,#50555,#50556,#50557,#50558,#50559,#50560,#50561,#50562,
#50563,#50564,#50565,#50566,#50567,#50568,#50569,#50570,#50571,#50572,#50573,
#50574,#50575,#50576,#50577,#50578,#50579,#50580),.UNSPECIFIED.,.F.,.F.)
B_SPLINE_CURVE_WITH_KNOTS((6,1,1,1,1,1,1,1,1,1,1,1,1,1,1,1,1,1,1,1,1,1,
1,1,1,1,1,1,1,1,1,1,1,1,1,1,1,1,1,1,1,1,1,1,1,1,1,1,1,1,1,1,1,1,1,1,1,1,
1,1,1,1,1,1,1,6),(-0.994228156739677,-0.984615384615383,-0.969230769230768,
-0.953846153846152,-0.938461538461537,-0.923076923076922,-0.907692307692306,
-0.892307692307691,-0.876923076923076,-0.86153846153846,-0.846153846153845,
-0.83076923076923,-0.815384615384614,-0.799999999999999,-0.784615384615384,
-0.769230769230768,-0.753846153846153,-0.738461538461538,-0.723076923076922,
-0.707692307692307,-0.692307692307692,-0.676923076923076,-0.661538461538461,
-0.646153846153846,-0.63076923076923,-0.615384615384615,-0.6,-0.584615384615384,
-0.569230769230769,-0.553846153846154,-0.538461538461538,-0.523076923076923,
-0.507692307692308,-0.492307692307692,-0.476923076923077,-0.461538461538462,
-0.446153846153846,-0.430769230769231,-0.415384615384615,-0.4,-0.384615384615385,
-0.369230769230769,-0.353846153846154,-0.338461538461538,-0.323076923076923,
-0.307692307692308,-0.292307692307692,-0.276923076923077,-0.261538461538462,
-0.246153846153846,-0.230769230769231,-0.215384615384615,-0.2,-0.184615384615385,
-0.169230769230769,-0.153846153846154,-0.138461538461538,-0.123076923076923,
-0.107692307692308,-0.0923076923076923,-0.0769230769230769,-0.0615384615384615,
-0.0461538461538462,-0.0307692307692308,-0.0153846153846154,0.),
 .UNSPECIFIED.)
CURVE()
GEOMETRIC_REPRESENTATION_ITEM()
RATIONAL_B_SPLINE_CURVE((1.,1.,1.,1.,1.,1.,1.,1.,1.,1.,1.,1.,1.,1.,1.,1.,
1.,1.,1.,1.,1.,1.,1.,1.,1.,1.,1.,1.,1.,1.,1.,1.,1.,1.,1.,1.,1.,1.,1.,1.,
1.,1.,1.,1.,1.,1.,1.,1.,1.,1.,1.,1.,1.,1.,1.,1.,1.,1.,1.,1.,1.,1.,1.,1.,
1.,1.,1.,1.,1.,1.))
REPRESENTATION_ITEM('')
);
#357=(
BOUNDED_CURVE()
B_SPLINE_CURVE(5,(#50733,#50734,#50735,#50736,#50737,#50738,#50739,#50740,
#50741,#50742,#50743,#50744,#50745,#50746,#50747,#50748,#50749,#50750,#50751,
#50752,#50753,#50754,#50755,#50756,#50757,#50758,#50759,#50760,#50761,#50762,
#50763,#50764,#50765,#50766,#50767,#50768,#50769,#50770,#50771,#50772,#50773,
#50774,#50775,#50776,#50777,#50778,#50779,#50780,#50781,#50782,#50783,#50784,
#50785,#50786,#50787,#50788,#50789,#50790,#50791,#50792,#50793,#50794,#50795,
#50796,#50797,#50798,#50799,#50800,#50801,#50802),.UNSPECIFIED.,.F.,.F.)
B_SPLINE_CURVE_WITH_KNOTS((6,1,1,1,1,1,1,1,1,1,1,1,1,1,1,1,1,1,1,1,1,1,
1,1,1,1,1,1,1,1,1,1,1,1,1,1,1,1,1,1,1,1,1,1,1,1,1,1,1,1,1,1,1,1,1,1,1,1,
1,1,1,1,1,1,1,6),(-1.,-0.984615384615383,-0.969230769230768,-0.953846153846152,
-0.938461538461537,-0.923076923076922,-0.907692307692306,-0.892307692307691,
-0.876923076923076,-0.86153846153846,-0.846153846153845,-0.83076923076923,
-0.815384615384614,-0.799999999999999,-0.784615384615384,-0.769230769230768,
-0.753846153846153,-0.738461538461538,-0.723076923076922,-0.707692307692307,
-0.692307692307692,-0.676923076923076,-0.661538461538461,-0.646153846153846,
-0.63076923076923,-0.615384615384615,-0.6,-0.584615384615384,-0.569230769230769,
-0.553846153846154,-0.538461538461538,-0.523076923076923,-0.507692307692308,
-0.492307692307692,-0.476923076923077,-0.461538461538462,-0.446153846153846,
-0.430769230769231,-0.415384615384615,-0.4,-0.384615384615385,-0.369230769230769,
-0.353846153846154,-0.338461538461538,-0.323076923076923,-0.307692307692308,
-0.292307692307692,-0.276923076923077,-0.261538461538462,-0.246153846153846,
-0.230769230769231,-0.215384615384615,-0.2,-0.184615384615385,-0.169230769230769,
-0.153846153846154,-0.138461538461538,-0.123076923076923,-0.107692307692308,
-0.0923076923076923,-0.0769230769230769,-0.0615384615384615,-0.0461538461538462,
-0.0307692307692308,-0.0153846153846154,-0.0057718433744938),
 .UNSPECIFIED.)
CURVE()
GEOMETRIC_REPRESENTATION_ITEM()
RATIONAL_B_SPLINE_CURVE((1.,1.,1.,1.,1.,1.,1.,1.,1.,1.,1.,1.,1.,1.,1.,1.,
1.,1.,1.,1.,1.,1.,1.,1.,1.,1.,1.,1.,1.,1.,1.,1.,1.,1.,1.,1.,1.,1.,1.,1.,
1.,1.,1.,1.,1.,1.,1.,1.,1.,1.,1.,1.,1.,1.,1.,1.,1.,1.,1.,1.,1.,1.,1.,1.,
1.,1.,1.,1.,1.,1.))
REPRESENTATION_ITEM('')
);
#358=(
BOUNDED_CURVE()
B_SPLINE_CURVE(5,(#50953,#50954,#50955,#50956,#50957,#50958,#50959,#50960,
#50961,#50962,#50963,#50964,#50965,#50966,#50967,#50968,#50969,#50970,#50971,
#50972,#50973,#50974,#50975,#50976,#50977,#50978,#50979,#50980,#50981,#50982,
#50983,#50984,#50985,#50986,#50987,#50988,#50989,#50990,#50991,#50992,#50993,
#50994,#50995,#50996,#50997,#50998,#50999,#51000,#51001,#51002,#51003,#51004,
#51005,#51006,#51007,#51008,#51009,#51010,#51011,#51012,#51013,#51014,#51015,
#51016,#51017,#51018,#51019,#51020,#51021,#51022),.UNSPECIFIED.,.F.,.F.)
B_SPLINE_CURVE_WITH_KNOTS((6,1,1,1,1,1,1,1,1,1,1,1,1,1,1,1,1,1,1,1,1,1,
1,1,1,1,1,1,1,1,1,1,1,1,1,1,1,1,1,1,1,1,1,1,1,1,1,1,1,1,1,1,1,1,1,1,1,1,
1,1,1,1,1,1,1,6),(-0.994228156739743,-0.984615384615383,-0.969230769230768,
-0.953846153846152,-0.938461538461537,-0.923076923076922,-0.907692307692306,
-0.892307692307691,-0.876923076923076,-0.86153846153846,-0.846153846153845,
-0.83076923076923,-0.815384615384614,-0.799999999999999,-0.784615384615384,
-0.769230769230768,-0.753846153846153,-0.738461538461538,-0.723076923076922,
-0.707692307692307,-0.692307692307692,-0.676923076923076,-0.661538461538461,
-0.646153846153846,-0.63076923076923,-0.615384615384615,-0.6,-0.584615384615384,
-0.569230769230769,-0.553846153846154,-0.538461538461538,-0.523076923076923,
-0.507692307692308,-0.492307692307692,-0.476923076923077,-0.461538461538462,
-0.446153846153846,-0.430769230769231,-0.415384615384615,-0.4,-0.384615384615385,
-0.369230769230769,-0.353846153846154,-0.338461538461538,-0.323076923076923,
-0.307692307692308,-0.292307692307692,-0.276923076923077,-0.261538461538462,
-0.246153846153846,-0.230769230769231,-0.215384615384615,-0.2,-0.184615384615385,
-0.169230769230769,-0.153846153846154,-0.138461538461538,-0.123076923076923,
-0.107692307692308,-0.0923076923076923,-0.0769230769230769,-0.0615384615384615,
-0.0461538461538462,-0.0307692307692308,-0.0153846153846154,0.),
 .UNSPECIFIED.)
CURVE()
GEOMETRIC_REPRESENTATION_ITEM()
RATIONAL_B_SPLINE_CURVE((1.,1.,1.,1.,1.,1.,1.,1.,1.,1.,1.,1.,1.,1.,1.,1.,
1.,1.,1.,1.,1.,1.,1.,1.,1.,1.,1.,1.,1.,1.,1.,1.,1.,1.,1.,1.,1.,1.,1.,1.,
1.,1.,1.,1.,1.,1.,1.,1.,1.,1.,1.,1.,1.,1.,1.,1.,1.,1.,1.,1.,1.,1.,1.,1.,
1.,1.,1.,1.,1.,1.))
REPRESENTATION_ITEM('')
);
#359=(
BOUNDED_CURVE()
B_SPLINE_CURVE(5,(#51175,#51176,#51177,#51178,#51179,#51180,#51181,#51182,
#51183,#51184,#51185,#51186,#51187,#51188,#51189,#51190,#51191,#51192,#51193,
#51194,#51195,#51196,#51197,#51198,#51199,#51200,#51201,#51202,#51203,#51204,
#51205,#51206,#51207,#51208,#51209,#51210,#51211,#51212,#51213,#51214,#51215,
#51216,#51217,#51218,#51219,#51220,#51221,#51222,#51223,#51224,#51225,#51226,
#51227,#51228,#51229,#51230,#51231,#51232,#51233,#51234,#51235,#51236,#51237,
#51238,#51239,#51240,#51241,#51242,#51243,#51244),.UNSPECIFIED.,.F.,.F.)
B_SPLINE_CURVE_WITH_KNOTS((6,1,1,1,1,1,1,1,1,1,1,1,1,1,1,1,1,1,1,1,1,1,
1,1,1,1,1,1,1,1,1,1,1,1,1,1,1,1,1,1,1,1,1,1,1,1,1,1,1,1,1,1,1,1,1,1,1,1,
1,1,1,1,1,1,1,6),(-1.,-0.984615384615383,-0.969230769230768,-0.953846153846152,
-0.938461538461537,-0.923076923076922,-0.907692307692306,-0.892307692307691,
-0.876923076923076,-0.86153846153846,-0.846153846153845,-0.83076923076923,
-0.815384615384614,-0.799999999999999,-0.784615384615384,-0.769230769230768,
-0.753846153846153,-0.738461538461538,-0.723076923076922,-0.707692307692307,
-0.692307692307692,-0.676923076923076,-0.661538461538461,-0.646153846153846,
-0.63076923076923,-0.615384615384615,-0.6,-0.584615384615384,-0.569230769230769,
-0.553846153846154,-0.538461538461538,-0.523076923076923,-0.507692307692308,
-0.492307692307692,-0.476923076923077,-0.461538461538462,-0.446153846153846,
-0.430769230769231,-0.415384615384615,-0.4,-0.384615384615385,-0.369230769230769,
-0.353846153846154,-0.338461538461538,-0.323076923076923,-0.307692307692308,
-0.292307692307692,-0.276923076923077,-0.261538461538462,-0.246153846153846,
-0.230769230769231,-0.215384615384615,-0.2,-0.184615384615385,-0.169230769230769,
-0.153846153846154,-0.138461538461538,-0.123076923076923,-0.107692307692308,
-0.0923076923076923,-0.0769230769230769,-0.0615384615384615,-0.0461538461538462,
-0.0307692307692308,-0.0153846153846154,-0.0057718433745291),
 .UNSPECIFIED.)
CURVE()
GEOMETRIC_REPRESENTATION_ITEM()
RATIONAL_B_SPLINE_CURVE((1.,1.,1.,1.,1.,1.,1.,1.,1.,1.,1.,1.,1.,1.,1.,1.,
1.,1.,1.,1.,1.,1.,1.,1.,1.,1.,1.,1.,1.,1.,1.,1.,1.,1.,1.,1.,1.,1.,1.,1.,
1.,1.,1.,1.,1.,1.,1.,1.,1.,1.,1.,1.,1.,1.,1.,1.,1.,1.,1.,1.,1.,1.,1.,1.,
1.,1.,1.,1.,1.,1.))
REPRESENTATION_ITEM('')
);
#360=(
BOUNDED_CURVE()
B_SPLINE_CURVE(5,(#51395,#51396,#51397,#51398,#51399,#51400,#51401,#51402,
#51403,#51404,#51405,#51406,#51407,#51408,#51409,#51410,#51411,#51412,#51413,
#51414,#51415,#51416,#51417,#51418,#51419,#51420,#51421,#51422,#51423,#51424,
#51425,#51426,#51427,#51428,#51429,#51430,#51431,#51432,#51433,#51434,#51435,
#51436,#51437,#51438,#51439,#51440,#51441,#51442,#51443,#51444,#51445,#51446,
#51447,#51448,#51449,#51450,#51451,#51452,#51453,#51454,#51455,#51456,#51457,
#51458,#51459,#51460,#51461,#51462,#51463,#51464),.UNSPECIFIED.,.F.,.F.)
B_SPLINE_CURVE_WITH_KNOTS((6,1,1,1,1,1,1,1,1,1,1,1,1,1,1,1,1,1,1,1,1,1,
1,1,1,1,1,1,1,1,1,1,1,1,1,1,1,1,1,1,1,1,1,1,1,1,1,1,1,1,1,1,1,1,1,1,1,1,
1,1,1,1,1,1,1,6),(-0.994228156739665,-0.984615384615383,-0.969230769230768,
-0.953846153846152,-0.938461538461537,-0.923076923076922,-0.907692307692306,
-0.892307692307691,-0.876923076923076,-0.86153846153846,-0.846153846153845,
-0.83076923076923,-0.815384615384614,-0.799999999999999,-0.784615384615384,
-0.769230769230768,-0.753846153846153,-0.738461538461538,-0.723076923076922,
-0.707692307692307,-0.692307692307692,-0.676923076923076,-0.661538461538461,
-0.646153846153846,-0.63076923076923,-0.615384615384615,-0.6,-0.584615384615384,
-0.569230769230769,-0.553846153846154,-0.538461538461538,-0.523076923076923,
-0.507692307692308,-0.492307692307692,-0.476923076923077,-0.461538461538462,
-0.446153846153846,-0.430769230769231,-0.415384615384615,-0.4,-0.384615384615385,
-0.369230769230769,-0.353846153846154,-0.338461538461538,-0.323076923076923,
-0.307692307692308,-0.292307692307692,-0.276923076923077,-0.261538461538462,
-0.246153846153846,-0.230769230769231,-0.215384615384615,-0.2,-0.184615384615385,
-0.169230769230769,-0.153846153846154,-0.138461538461538,-0.123076923076923,
-0.107692307692308,-0.0923076923076923,-0.0769230769230769,-0.0615384615384615,
-0.0461538461538462,-0.0307692307692308,-0.0153846153846154,0.),
 .UNSPECIFIED.)
CURVE()
GEOMETRIC_REPRESENTATION_ITEM()
RATIONAL_B_SPLINE_CURVE((1.,1.,1.,1.,1.,1.,1.,1.,1.,1.,1.,1.,1.,1.,1.,1.,
1.,1.,1.,1.,1.,1.,1.,1.,1.,1.,1.,1.,1.,1.,1.,1.,1.,1.,1.,1.,1.,1.,1.,1.,
1.,1.,1.,1.,1.,1.,1.,1.,1.,1.,1.,1.,1.,1.,1.,1.,1.,1.,1.,1.,1.,1.,1.,1.,
1.,1.,1.,1.,1.,1.))
REPRESENTATION_ITEM('')
);
#361=(
BOUNDED_CURVE()
B_SPLINE_CURVE(5,(#51617,#51618,#51619,#51620,#51621,#51622,#51623,#51624,
#51625,#51626,#51627,#51628,#51629,#51630,#51631,#51632,#51633,#51634,#51635,
#51636,#51637,#51638,#51639,#51640,#51641,#51642,#51643,#51644,#51645,#51646,
#51647,#51648,#51649,#51650,#51651,#51652,#51653,#51654,#51655,#51656,#51657,
#51658,#51659,#51660,#51661,#51662,#51663,#51664,#51665,#51666,#51667,#51668,
#51669,#51670,#51671,#51672,#51673,#51674,#51675,#51676,#51677,#51678,#51679,
#51680,#51681,#51682,#51683,#51684,#51685,#51686),.UNSPECIFIED.,.F.,.F.)
B_SPLINE_CURVE_WITH_KNOTS((6,1,1,1,1,1,1,1,1,1,1,1,1,1,1,1,1,1,1,1,1,1,
1,1,1,1,1,1,1,1,1,1,1,1,1,1,1,1,1,1,1,1,1,1,1,1,1,1,1,1,1,1,1,1,1,1,1,1,
1,1,1,1,1,1,1,6),(-1.,-0.984615384615383,-0.969230769230768,-0.953846153846152,
-0.938461538461537,-0.923076923076922,-0.907692307692306,-0.892307692307691,
-0.876923076923076,-0.86153846153846,-0.846153846153845,-0.83076923076923,
-0.815384615384614,-0.799999999999999,-0.784615384615384,-0.769230769230768,
-0.753846153846153,-0.738461538461538,-0.723076923076922,-0.707692307692307,
-0.692307692307692,-0.676923076923076,-0.661538461538461,-0.646153846153846,
-0.63076923076923,-0.615384615384615,-0.6,-0.584615384615384,-0.569230769230769,
-0.553846153846154,-0.538461538461538,-0.523076923076923,-0.507692307692308,
-0.492307692307692,-0.476923076923077,-0.461538461538462,-0.446153846153846,
-0.430769230769231,-0.415384615384615,-0.4,-0.384615384615385,-0.369230769230769,
-0.353846153846154,-0.338461538461538,-0.323076923076923,-0.307692307692308,
-0.292307692307692,-0.276923076923077,-0.261538461538462,-0.246153846153846,
-0.230769230769231,-0.215384615384615,-0.2,-0.184615384615385,-0.169230769230769,
-0.153846153846154,-0.138461538461538,-0.123076923076923,-0.107692307692308,
-0.0923076923076923,-0.0769230769230769,-0.0615384615384615,-0.0461538461538462,
-0.0307692307692308,-0.0153846153846154,-0.00577184337450666),
 .UNSPECIFIED.)
CURVE()
GEOMETRIC_REPRESENTATION_ITEM()
RATIONAL_B_SPLINE_CURVE((1.,1.,1.,1.,1.,1.,1.,1.,1.,1.,1.,1.,1.,1.,1.,1.,
1.,1.,1.,1.,1.,1.,1.,1.,1.,1.,1.,1.,1.,1.,1.,1.,1.,1.,1.,1.,1.,1.,1.,1.,
1.,1.,1.,1.,1.,1.,1.,1.,1.,1.,1.,1.,1.,1.,1.,1.,1.,1.,1.,1.,1.,1.,1.,1.,
1.,1.,1.,1.,1.,1.))
REPRESENTATION_ITEM('')
);
#362=(
BOUNDED_CURVE()
B_SPLINE_CURVE(5,(#51837,#51838,#51839,#51840,#51841,#51842,#51843,#51844,
#51845,#51846,#51847,#51848,#51849,#51850,#51851,#51852,#51853,#51854,#51855,
#51856,#51857,#51858,#51859,#51860,#51861,#51862,#51863,#51864,#51865,#51866,
#51867,#51868,#51869,#51870,#51871,#51872,#51873,#51874,#51875,#51876,#51877,
#51878,#51879,#51880,#51881,#51882,#51883,#51884,#51885,#51886,#51887,#51888,
#51889,#51890,#51891,#51892,#51893,#51894,#51895,#51896,#51897,#51898,#51899,
#51900,#51901,#51902,#51903,#51904,#51905,#51906),.UNSPECIFIED.,.F.,.F.)
B_SPLINE_CURVE_WITH_KNOTS((6,1,1,1,1,1,1,1,1,1,1,1,1,1,1,1,1,1,1,1,1,1,
1,1,1,1,1,1,1,1,1,1,1,1,1,1,1,1,1,1,1,1,1,1,1,1,1,1,1,1,1,1,1,1,1,1,1,1,
1,1,1,1,1,1,1,6),(-0.994228156739758,-0.984615384615383,-0.969230769230768,
-0.953846153846152,-0.938461538461537,-0.923076923076922,-0.907692307692306,
-0.892307692307691,-0.876923076923076,-0.86153846153846,-0.846153846153845,
-0.83076923076923,-0.815384615384614,-0.799999999999999,-0.784615384615384,
-0.769230769230768,-0.753846153846153,-0.738461538461538,-0.723076923076922,
-0.707692307692307,-0.692307692307692,-0.676923076923076,-0.661538461538461,
-0.646153846153846,-0.63076923076923,-0.615384615384615,-0.6,-0.584615384615384,
-0.569230769230769,-0.553846153846154,-0.538461538461538,-0.523076923076923,
-0.507692307692308,-0.492307692307692,-0.476923076923077,-0.461538461538462,
-0.446153846153846,-0.430769230769231,-0.415384615384615,-0.4,-0.384615384615385,
-0.369230769230769,-0.353846153846154,-0.338461538461538,-0.323076923076923,
-0.307692307692308,-0.292307692307692,-0.276923076923077,-0.261538461538462,
-0.246153846153846,-0.230769230769231,-0.215384615384615,-0.2,-0.184615384615385,
-0.169230769230769,-0.153846153846154,-0.138461538461538,-0.123076923076923,
-0.107692307692308,-0.0923076923076923,-0.0769230769230769,-0.0615384615384615,
-0.0461538461538462,-0.0307692307692308,-0.0153846153846154,0.),
 .UNSPECIFIED.)
CURVE()
GEOMETRIC_REPRESENTATION_ITEM()
RATIONAL_B_SPLINE_CURVE((1.,1.,1.,1.,1.,1.,1.,1.,1.,1.,1.,1.,1.,1.,1.,1.,
1.,1.,1.,1.,1.,1.,1.,1.,1.,1.,1.,1.,1.,1.,1.,1.,1.,1.,1.,1.,1.,1.,1.,1.,
1.,1.,1.,1.,1.,1.,1.,1.,1.,1.,1.,1.,1.,1.,1.,1.,1.,1.,1.,1.,1.,1.,1.,1.,
1.,1.,1.,1.,1.,1.))
REPRESENTATION_ITEM('')
);
#363=(
BOUNDED_CURVE()
B_SPLINE_CURVE(5,(#52059,#52060,#52061,#52062,#52063,#52064,#52065,#52066,
#52067,#52068,#52069,#52070,#52071,#52072,#52073,#52074,#52075,#52076,#52077,
#52078,#52079,#52080,#52081,#52082,#52083,#52084,#52085,#52086,#52087,#52088,
#52089,#52090,#52091,#52092,#52093,#52094,#52095,#52096,#52097,#52098,#52099,
#52100,#52101,#52102,#52103,#52104,#52105,#52106,#52107,#52108,#52109,#52110,
#52111,#52112,#52113,#52114,#52115,#52116,#52117,#52118,#52119,#52120,#52121,
#52122,#52123,#52124,#52125,#52126,#52127,#52128),.UNSPECIFIED.,.F.,.F.)
B_SPLINE_CURVE_WITH_KNOTS((6,1,1,1,1,1,1,1,1,1,1,1,1,1,1,1,1,1,1,1,1,1,
1,1,1,1,1,1,1,1,1,1,1,1,1,1,1,1,1,1,1,1,1,1,1,1,1,1,1,1,1,1,1,1,1,1,1,1,
1,1,1,1,1,1,1,6),(-1.,-0.984615384615383,-0.969230769230768,-0.953846153846152,
-0.938461538461537,-0.923076923076922,-0.907692307692306,-0.892307692307691,
-0.876923076923076,-0.86153846153846,-0.846153846153845,-0.83076923076923,
-0.815384615384614,-0.799999999999999,-0.784615384615384,-0.769230769230768,
-0.753846153846153,-0.738461538461538,-0.723076923076922,-0.707692307692307,
-0.692307692307692,-0.676923076923076,-0.661538461538461,-0.646153846153846,
-0.63076923076923,-0.615384615384615,-0.6,-0.584615384615384,-0.569230769230769,
-0.553846153846154,-0.538461538461538,-0.523076923076923,-0.507692307692308,
-0.492307692307692,-0.476923076923077,-0.461538461538462,-0.446153846153846,
-0.430769230769231,-0.415384615384615,-0.4,-0.384615384615385,-0.369230769230769,
-0.353846153846154,-0.338461538461538,-0.323076923076923,-0.307692307692308,
-0.292307692307692,-0.276923076923077,-0.261538461538462,-0.246153846153846,
-0.230769230769231,-0.215384615384615,-0.2,-0.184615384615385,-0.169230769230769,
-0.153846153846154,-0.138461538461538,-0.123076923076923,-0.107692307692308,
-0.0923076923076923,-0.0769230769230769,-0.0615384615384615,-0.0461538461538462,
-0.0307692307692308,-0.0153846153846154,-0.00577184337451981),
 .UNSPECIFIED.)
CURVE()
GEOMETRIC_REPRESENTATION_ITEM()
RATIONAL_B_SPLINE_CURVE((1.,1.,1.,1.,1.,1.,1.,1.,1.,1.,1.,1.,1.,1.,1.,1.,
1.,1.,1.,1.,1.,1.,1.,1.,1.,1.,1.,1.,1.,1.,1.,1.,1.,1.,1.,1.,1.,1.,1.,1.,
1.,1.,1.,1.,1.,1.,1.,1.,1.,1.,1.,1.,1.,1.,1.,1.,1.,1.,1.,1.,1.,1.,1.,1.,
1.,1.,1.,1.,1.,1.))
REPRESENTATION_ITEM('')
);
#364=(
BOUNDED_CURVE()
B_SPLINE_CURVE(5,(#52279,#52280,#52281,#52282,#52283,#52284,#52285,#52286,
#52287,#52288,#52289,#52290,#52291,#52292,#52293,#52294,#52295,#52296,#52297,
#52298,#52299,#52300,#52301,#52302,#52303,#52304,#52305,#52306,#52307,#52308,
#52309,#52310,#52311,#52312,#52313,#52314,#52315,#52316,#52317,#52318,#52319,
#52320,#52321,#52322,#52323,#52324,#52325,#52326,#52327,#52328,#52329,#52330,
#52331,#52332,#52333,#52334,#52335,#52336,#52337,#52338,#52339,#52340,#52341,
#52342,#52343,#52344,#52345,#52346,#52347,#52348),.UNSPECIFIED.,.F.,.F.)
B_SPLINE_CURVE_WITH_KNOTS((6,1,1,1,1,1,1,1,1,1,1,1,1,1,1,1,1,1,1,1,1,1,
1,1,1,1,1,1,1,1,1,1,1,1,1,1,1,1,1,1,1,1,1,1,1,1,1,1,1,1,1,1,1,1,1,1,1,1,
1,1,1,1,1,1,1,6),(-0.994228156739659,-0.984615384615383,-0.969230769230768,
-0.953846153846152,-0.938461538461537,-0.923076923076922,-0.907692307692306,
-0.892307692307691,-0.876923076923076,-0.86153846153846,-0.846153846153845,
-0.83076923076923,-0.815384615384614,-0.799999999999999,-0.784615384615384,
-0.769230769230768,-0.753846153846153,-0.738461538461538,-0.723076923076922,
-0.707692307692307,-0.692307692307692,-0.676923076923076,-0.661538461538461,
-0.646153846153846,-0.63076923076923,-0.615384615384615,-0.6,-0.584615384615384,
-0.569230769230769,-0.553846153846154,-0.538461538461538,-0.523076923076923,
-0.507692307692308,-0.492307692307692,-0.476923076923077,-0.461538461538462,
-0.446153846153846,-0.430769230769231,-0.415384615384615,-0.4,-0.384615384615385,
-0.369230769230769,-0.353846153846154,-0.338461538461538,-0.323076923076923,
-0.307692307692308,-0.292307692307692,-0.276923076923077,-0.261538461538462,
-0.246153846153846,-0.230769230769231,-0.215384615384615,-0.2,-0.184615384615385,
-0.169230769230769,-0.153846153846154,-0.138461538461538,-0.123076923076923,
-0.107692307692308,-0.0923076923076923,-0.0769230769230769,-0.0615384615384615,
-0.0461538461538462,-0.0307692307692308,-0.0153846153846154,0.),
 .UNSPECIFIED.)
CURVE()
GEOMETRIC_REPRESENTATION_ITEM()
RATIONAL_B_SPLINE_CURVE((1.,1.,1.,1.,1.,1.,1.,1.,1.,1.,1.,1.,1.,1.,1.,1.,
1.,1.,1.,1.,1.,1.,1.,1.,1.,1.,1.,1.,1.,1.,1.,1.,1.,1.,1.,1.,1.,1.,1.,1.,
1.,1.,1.,1.,1.,1.,1.,1.,1.,1.,1.,1.,1.,1.,1.,1.,1.,1.,1.,1.,1.,1.,1.,1.,
1.,1.,1.,1.,1.,1.))
REPRESENTATION_ITEM('')
);
#365=(
BOUNDED_CURVE()
B_SPLINE_CURVE(5,(#52501,#52502,#52503,#52504,#52505,#52506,#52507,#52508,
#52509,#52510,#52511,#52512,#52513,#52514,#52515,#52516,#52517,#52518,#52519,
#52520,#52521,#52522,#52523,#52524,#52525,#52526,#52527,#52528,#52529,#52530,
#52531,#52532,#52533,#52534,#52535,#52536,#52537,#52538,#52539,#52540,#52541,
#52542,#52543,#52544,#52545,#52546,#52547,#52548,#52549,#52550,#52551,#52552,
#52553,#52554,#52555,#52556,#52557,#52558,#52559,#52560,#52561,#52562,#52563,
#52564,#52565,#52566,#52567,#52568,#52569,#52570),.UNSPECIFIED.,.F.,.F.)
B_SPLINE_CURVE_WITH_KNOTS((6,1,1,1,1,1,1,1,1,1,1,1,1,1,1,1,1,1,1,1,1,1,
1,1,1,1,1,1,1,1,1,1,1,1,1,1,1,1,1,1,1,1,1,1,1,1,1,1,1,1,1,1,1,1,1,1,1,1,
1,1,1,1,1,1,1,6),(-1.,-0.984615384615383,-0.969230769230768,-0.953846153846152,
-0.938461538461537,-0.923076923076922,-0.907692307692306,-0.892307692307691,
-0.876923076923076,-0.86153846153846,-0.846153846153845,-0.83076923076923,
-0.815384615384614,-0.799999999999999,-0.784615384615384,-0.769230769230768,
-0.753846153846153,-0.738461538461538,-0.723076923076922,-0.707692307692307,
-0.692307692307692,-0.676923076923076,-0.661538461538461,-0.646153846153846,
-0.63076923076923,-0.615384615384615,-0.6,-0.584615384615384,-0.569230769230769,
-0.553846153846154,-0.538461538461538,-0.523076923076923,-0.507692307692308,
-0.492307692307692,-0.476923076923077,-0.461538461538462,-0.446153846153846,
-0.430769230769231,-0.415384615384615,-0.4,-0.384615384615385,-0.369230769230769,
-0.353846153846154,-0.338461538461538,-0.323076923076923,-0.307692307692308,
-0.292307692307692,-0.276923076923077,-0.261538461538462,-0.246153846153846,
-0.230769230769231,-0.215384615384615,-0.2,-0.184615384615385,-0.169230769230769,
-0.153846153846154,-0.138461538461538,-0.123076923076923,-0.107692307692308,
-0.0923076923076923,-0.0769230769230769,-0.0615384615384615,-0.0461538461538462,
-0.0307692307692308,-0.0153846153846154,-0.00577184337450306),
 .UNSPECIFIED.)
CURVE()
GEOMETRIC_REPRESENTATION_ITEM()
RATIONAL_B_SPLINE_CURVE((1.,1.,1.,1.,1.,1.,1.,1.,1.,1.,1.,1.,1.,1.,1.,1.,
1.,1.,1.,1.,1.,1.,1.,1.,1.,1.,1.,1.,1.,1.,1.,1.,1.,1.,1.,1.,1.,1.,1.,1.,
1.,1.,1.,1.,1.,1.,1.,1.,1.,1.,1.,1.,1.,1.,1.,1.,1.,1.,1.,1.,1.,1.,1.,1.,
1.,1.,1.,1.,1.,1.))
REPRESENTATION_ITEM('')
);
#366=(
BOUNDED_CURVE()
B_SPLINE_CURVE(5,(#52721,#52722,#52723,#52724,#52725,#52726,#52727,#52728,
#52729,#52730,#52731,#52732,#52733,#52734,#52735,#52736,#52737,#52738,#52739,
#52740,#52741,#52742,#52743,#52744,#52745,#52746,#52747,#52748,#52749,#52750,
#52751,#52752,#52753,#52754,#52755,#52756,#52757,#52758,#52759,#52760,#52761,
#52762,#52763,#52764,#52765,#52766,#52767,#52768,#52769,#52770,#52771,#52772,
#52773,#52774,#52775,#52776,#52777,#52778,#52779,#52780,#52781,#52782,#52783,
#52784,#52785,#52786,#52787,#52788,#52789,#52790),.UNSPECIFIED.,.F.,.F.)
B_SPLINE_CURVE_WITH_KNOTS((6,1,1,1,1,1,1,1,1,1,1,1,1,1,1,1,1,1,1,1,1,1,
1,1,1,1,1,1,1,1,1,1,1,1,1,1,1,1,1,1,1,1,1,1,1,1,1,1,1,1,1,1,1,1,1,1,1,1,
1,1,1,1,1,1,1,6),(-0.994228156739675,-0.984615384615383,-0.969230769230768,
-0.953846153846152,-0.938461538461537,-0.923076923076922,-0.907692307692306,
-0.892307692307691,-0.876923076923076,-0.86153846153846,-0.846153846153845,
-0.83076923076923,-0.815384615384614,-0.799999999999999,-0.784615384615384,
-0.769230769230768,-0.753846153846153,-0.738461538461538,-0.723076923076922,
-0.707692307692307,-0.692307692307692,-0.676923076923076,-0.661538461538461,
-0.646153846153846,-0.63076923076923,-0.615384615384615,-0.6,-0.584615384615384,
-0.569230769230769,-0.553846153846154,-0.538461538461538,-0.523076923076923,
-0.507692307692308,-0.492307692307692,-0.476923076923077,-0.461538461538462,
-0.446153846153846,-0.430769230769231,-0.415384615384615,-0.4,-0.384615384615385,
-0.369230769230769,-0.353846153846154,-0.338461538461538,-0.323076923076923,
-0.307692307692308,-0.292307692307692,-0.276923076923077,-0.261538461538462,
-0.246153846153846,-0.230769230769231,-0.215384615384615,-0.2,-0.184615384615385,
-0.169230769230769,-0.153846153846154,-0.138461538461538,-0.123076923076923,
-0.107692307692308,-0.0923076923076923,-0.0769230769230769,-0.0615384615384615,
-0.0461538461538462,-0.0307692307692308,-0.0153846153846154,0.),
 .UNSPECIFIED.)
CURVE()
GEOMETRIC_REPRESENTATION_ITEM()
RATIONAL_B_SPLINE_CURVE((1.,1.,1.,1.,1.,1.,1.,1.,1.,1.,1.,1.,1.,1.,1.,1.,
1.,1.,1.,1.,1.,1.,1.,1.,1.,1.,1.,1.,1.,1.,1.,1.,1.,1.,1.,1.,1.,1.,1.,1.,
1.,1.,1.,1.,1.,1.,1.,1.,1.,1.,1.,1.,1.,1.,1.,1.,1.,1.,1.,1.,1.,1.,1.,1.,
1.,1.,1.,1.,1.,1.))
REPRESENTATION_ITEM('')
);
#367=(
BOUNDED_CURVE()
B_SPLINE_CURVE(5,(#52943,#52944,#52945,#52946,#52947,#52948,#52949,#52950,
#52951,#52952,#52953,#52954,#52955,#52956,#52957,#52958,#52959,#52960,#52961,
#52962,#52963,#52964,#52965,#52966,#52967,#52968,#52969,#52970,#52971,#52972,
#52973,#52974,#52975,#52976,#52977,#52978,#52979,#52980,#52981,#52982,#52983,
#52984,#52985,#52986,#52987,#52988,#52989,#52990,#52991,#52992,#52993,#52994,
#52995,#52996,#52997,#52998,#52999,#53000,#53001,#53002,#53003,#53004,#53005,
#53006,#53007,#53008,#53009,#53010,#53011,#53012),.UNSPECIFIED.,.F.,.F.)
B_SPLINE_CURVE_WITH_KNOTS((6,1,1,1,1,1,1,1,1,1,1,1,1,1,1,1,1,1,1,1,1,1,
1,1,1,1,1,1,1,1,1,1,1,1,1,1,1,1,1,1,1,1,1,1,1,1,1,1,1,1,1,1,1,1,1,1,1,1,
1,1,1,1,1,1,1,6),(-1.,-0.984615384615383,-0.969230769230768,-0.953846153846152,
-0.938461538461537,-0.923076923076922,-0.907692307692306,-0.892307692307691,
-0.876923076923076,-0.86153846153846,-0.846153846153845,-0.83076923076923,
-0.815384615384614,-0.799999999999999,-0.784615384615384,-0.769230769230768,
-0.753846153846153,-0.738461538461538,-0.723076923076922,-0.707692307692307,
-0.692307692307692,-0.676923076923076,-0.661538461538461,-0.646153846153846,
-0.63076923076923,-0.615384615384615,-0.6,-0.584615384615384,-0.569230769230769,
-0.553846153846154,-0.538461538461538,-0.523076923076923,-0.507692307692308,
-0.492307692307692,-0.476923076923077,-0.461538461538462,-0.446153846153846,
-0.430769230769231,-0.415384615384615,-0.4,-0.384615384615385,-0.369230769230769,
-0.353846153846154,-0.338461538461538,-0.323076923076923,-0.307692307692308,
-0.292307692307692,-0.276923076923077,-0.261538461538462,-0.246153846153846,
-0.230769230769231,-0.215384615384615,-0.2,-0.184615384615385,-0.169230769230769,
-0.153846153846154,-0.138461538461538,-0.123076923076923,-0.107692307692308,
-0.0923076923076923,-0.0769230769230769,-0.0615384615384615,-0.0461538461538462,
-0.0307692307692308,-0.0153846153846154,-0.00577184337450328),
 .UNSPECIFIED.)
CURVE()
GEOMETRIC_REPRESENTATION_ITEM()
RATIONAL_B_SPLINE_CURVE((1.,1.,1.,1.,1.,1.,1.,1.,1.,1.,1.,1.,1.,1.,1.,1.,
1.,1.,1.,1.,1.,1.,1.,1.,1.,1.,1.,1.,1.,1.,1.,1.,1.,1.,1.,1.,1.,1.,1.,1.,
1.,1.,1.,1.,1.,1.,1.,1.,1.,1.,1.,1.,1.,1.,1.,1.,1.,1.,1.,1.,1.,1.,1.,1.,
1.,1.,1.,1.,1.,1.))
REPRESENTATION_ITEM('')
);
#368=(
BOUNDED_CURVE()
B_SPLINE_CURVE(5,(#53165,#53166,#53167,#53168,#53169,#53170,#53171,#53172,
#53173,#53174,#53175,#53176,#53177,#53178,#53179,#53180,#53181,#53182,#53183,
#53184,#53185,#53186,#53187,#53188,#53189,#53190,#53191,#53192,#53193,#53194,
#53195,#53196,#53197,#53198,#53199,#53200,#53201,#53202,#53203,#53204,#53205,
#53206,#53207,#53208,#53209,#53210,#53211,#53212,#53213,#53214,#53215,#53216,
#53217,#53218,#53219,#53220,#53221,#53222,#53223,#53224,#53225,#53226,#53227,
#53228,#53229,#53230,#53231,#53232,#53233,#53234),.UNSPECIFIED.,.F.,.F.)
B_SPLINE_CURVE_WITH_KNOTS((6,1,1,1,1,1,1,1,1,1,1,1,1,1,1,1,1,1,1,1,1,1,
1,1,1,1,1,1,1,1,1,1,1,1,1,1,1,1,1,1,1,1,1,1,1,1,1,1,1,1,1,1,1,1,1,1,1,1,
1,1,1,1,1,1,1,6),(-0.994228156739672,-0.984615384615383,-0.969230769230768,
-0.953846153846152,-0.938461538461537,-0.923076923076922,-0.907692307692306,
-0.892307692307691,-0.876923076923076,-0.86153846153846,-0.846153846153845,
-0.83076923076923,-0.815384615384614,-0.799999999999999,-0.784615384615384,
-0.769230769230768,-0.753846153846153,-0.738461538461538,-0.723076923076922,
-0.707692307692307,-0.692307692307692,-0.676923076923076,-0.661538461538461,
-0.646153846153846,-0.63076923076923,-0.615384615384615,-0.6,-0.584615384615384,
-0.569230769230769,-0.553846153846154,-0.538461538461538,-0.523076923076923,
-0.507692307692308,-0.492307692307692,-0.476923076923077,-0.461538461538462,
-0.446153846153846,-0.430769230769231,-0.415384615384615,-0.4,-0.384615384615385,
-0.369230769230769,-0.353846153846154,-0.338461538461538,-0.323076923076923,
-0.307692307692308,-0.292307692307692,-0.276923076923077,-0.261538461538462,
-0.246153846153846,-0.230769230769231,-0.215384615384615,-0.2,-0.184615384615385,
-0.169230769230769,-0.153846153846154,-0.138461538461538,-0.123076923076923,
-0.107692307692308,-0.0923076923076923,-0.0769230769230769,-0.0615384615384615,
-0.0461538461538462,-0.0307692307692308,-0.0153846153846154,0.),
 .UNSPECIFIED.)
CURVE()
GEOMETRIC_REPRESENTATION_ITEM()
RATIONAL_B_SPLINE_CURVE((1.,1.,1.,1.,1.,1.,1.,1.,1.,1.,1.,1.,1.,1.,1.,1.,
1.,1.,1.,1.,1.,1.,1.,1.,1.,1.,1.,1.,1.,1.,1.,1.,1.,1.,1.,1.,1.,1.,1.,1.,
1.,1.,1.,1.,1.,1.,1.,1.,1.,1.,1.,1.,1.,1.,1.,1.,1.,1.,1.,1.,1.,1.,1.,1.,
1.,1.,1.,1.,1.,1.))
REPRESENTATION_ITEM('')
);
#369=(
BOUNDED_CURVE()
B_SPLINE_CURVE(5,(#53393,#53394,#53395,#53396,#53397,#53398,#53399,#53400,
#53401,#53402,#53403,#53404,#53405,#53406,#53407,#53408,#53409,#53410,#53411,
#53412,#53413,#53414,#53415,#53416,#53417,#53418,#53419,#53420,#53421,#53422,
#53423,#53424,#53425,#53426,#53427,#53428,#53429,#53430,#53431,#53432,#53433,
#53434,#53435,#53436,#53437,#53438,#53439,#53440,#53441,#53442,#53443,#53444,
#53445,#53446,#53447,#53448,#53449,#53450,#53451,#53452,#53453,#53454,#53455,
#53456,#53457,#53458,#53459,#53460,#53461,#53462),.UNSPECIFIED.,.F.,.F.)
B_SPLINE_CURVE_WITH_KNOTS((6,1,1,1,1,1,1,1,1,1,1,1,1,1,1,1,1,1,1,1,1,1,
1,1,1,1,1,1,1,1,1,1,1,1,1,1,1,1,1,1,1,1,1,1,1,1,1,1,1,1,1,1,1,1,1,1,1,1,
1,1,1,1,1,1,1,6),(-0.994228156739704,-0.984615384615383,-0.969230769230768,
-0.953846153846152,-0.938461538461537,-0.923076923076922,-0.907692307692306,
-0.892307692307691,-0.876923076923076,-0.86153846153846,-0.846153846153845,
-0.83076923076923,-0.815384615384614,-0.799999999999999,-0.784615384615384,
-0.769230769230768,-0.753846153846153,-0.738461538461538,-0.723076923076922,
-0.707692307692307,-0.692307692307692,-0.676923076923076,-0.661538461538461,
-0.646153846153846,-0.63076923076923,-0.615384615384615,-0.6,-0.584615384615384,
-0.569230769230769,-0.553846153846154,-0.538461538461538,-0.523076923076923,
-0.507692307692308,-0.492307692307692,-0.476923076923077,-0.461538461538462,
-0.446153846153846,-0.430769230769231,-0.415384615384615,-0.4,-0.384615384615385,
-0.369230769230769,-0.353846153846154,-0.338461538461538,-0.323076923076923,
-0.307692307692308,-0.292307692307692,-0.276923076923077,-0.261538461538462,
-0.246153846153846,-0.230769230769231,-0.215384615384615,-0.2,-0.184615384615385,
-0.169230769230769,-0.153846153846154,-0.138461538461538,-0.123076923076923,
-0.107692307692308,-0.0923076923076923,-0.0769230769230769,-0.0615384615384615,
-0.0461538461538462,-0.0307692307692308,-0.0153846153846154,0.),
 .UNSPECIFIED.)
CURVE()
GEOMETRIC_REPRESENTATION_ITEM()
RATIONAL_B_SPLINE_CURVE((1.,1.,1.,1.,1.,1.,1.,1.,1.,1.,1.,1.,1.,1.,1.,1.,
1.,1.,1.,1.,1.,1.,1.,1.,1.,1.,1.,1.,1.,1.,1.,1.,1.,1.,1.,1.,1.,1.,1.,1.,
1.,1.,1.,1.,1.,1.,1.,1.,1.,1.,1.,1.,1.,1.,1.,1.,1.,1.,1.,1.,1.,1.,1.,1.,
1.,1.,1.,1.,1.,1.))
REPRESENTATION_ITEM('')
);
#370=(
BOUNDED_CURVE()
B_SPLINE_CURVE(5,(#53604,#53605,#53606,#53607,#53608,#53609,#53610,#53611,
#53612,#53613,#53614,#53615,#53616,#53617,#53618,#53619,#53620,#53621,#53622,
#53623,#53624,#53625,#53626,#53627,#53628,#53629,#53630,#53631,#53632,#53633,
#53634,#53635,#53636,#53637,#53638,#53639,#53640,#53641,#53642,#53643,#53644,
#53645,#53646,#53647,#53648,#53649,#53650,#53651,#53652,#53653,#53654,#53655,
#53656,#53657,#53658,#53659,#53660,#53661,#53662,#53663,#53664,#53665,#53666,
#53667,#53668,#53669,#53670,#53671,#53672,#53673),.UNSPECIFIED.,.F.,.F.)
B_SPLINE_CURVE_WITH_KNOTS((6,1,1,1,1,1,1,1,1,1,1,1,1,1,1,1,1,1,1,1,1,1,
1,1,1,1,1,1,1,1,1,1,1,1,1,1,1,1,1,1,1,1,1,1,1,1,1,1,1,1,1,1,1,1,1,1,1,1,
1,1,1,1,1,1,1,6),(-1.,-0.984615384615383,-0.969230769230768,-0.953846153846152,
-0.938461538461537,-0.923076923076922,-0.907692307692306,-0.892307692307691,
-0.876923076923076,-0.86153846153846,-0.846153846153845,-0.83076923076923,
-0.815384615384614,-0.799999999999999,-0.784615384615384,-0.769230769230768,
-0.753846153846153,-0.738461538461538,-0.723076923076922,-0.707692307692307,
-0.692307692307692,-0.676923076923076,-0.661538461538461,-0.646153846153846,
-0.63076923076923,-0.615384615384615,-0.6,-0.584615384615384,-0.569230769230769,
-0.553846153846154,-0.538461538461538,-0.523076923076923,-0.507692307692308,
-0.492307692307692,-0.476923076923077,-0.461538461538462,-0.446153846153846,
-0.430769230769231,-0.415384615384615,-0.4,-0.384615384615385,-0.369230769230769,
-0.353846153846154,-0.338461538461538,-0.323076923076923,-0.307692307692308,
-0.292307692307692,-0.276923076923077,-0.261538461538462,-0.246153846153846,
-0.230769230769231,-0.215384615384615,-0.2,-0.184615384615385,-0.169230769230769,
-0.153846153846154,-0.138461538461538,-0.123076923076923,-0.107692307692308,
-0.0923076923076923,-0.0769230769230769,-0.0615384615384615,-0.0461538461538462,
-0.0307692307692308,-0.0153846153846154,-0.00577184337451611),
 .UNSPECIFIED.)
CURVE()
GEOMETRIC_REPRESENTATION_ITEM()
RATIONAL_B_SPLINE_CURVE((1.,1.,1.,1.,1.,1.,1.,1.,1.,1.,1.,1.,1.,1.,1.,1.,
1.,1.,1.,1.,1.,1.,1.,1.,1.,1.,1.,1.,1.,1.,1.,1.,1.,1.,1.,1.,1.,1.,1.,1.,
1.,1.,1.,1.,1.,1.,1.,1.,1.,1.,1.,1.,1.,1.,1.,1.,1.,1.,1.,1.,1.,1.,1.,1.,
1.,1.,1.,1.,1.,1.))
REPRESENTATION_ITEM('')
);
#371=ITEM_DEFINED_TRANSFORMATION($,$,#12154,#12276);
#372=ITEM_DEFINED_TRANSFORMATION($,$,#12174,#12277);
#373=ITEM_DEFINED_TRANSFORMATION($,$,#12194,#12278);
#374=ITEM_DEFINED_TRANSFORMATION($,$,#12209,#12279);
#375=ITEM_DEFINED_TRANSFORMATION($,$,#12259,#12280);
#376=ITEM_DEFINED_TRANSFORMATION($,$,#12282,#12410);
#377=ITEM_DEFINED_TRANSFORMATION($,$,#12302,#12411);
#378=ITEM_DEFINED_TRANSFORMATION($,$,#12322,#12412);
#379=ITEM_DEFINED_TRANSFORMATION($,$,#12339,#12413);
#380=ITEM_DEFINED_TRANSFORMATION($,$,#12393,#12414);
#381=ITEM_DEFINED_TRANSFORMATION($,$,#11808,#12441);
#382=ITEM_DEFINED_TRANSFORMATION($,$,#11827,#12442);
#383=ITEM_DEFINED_TRANSFORMATION($,$,#11902,#12443);
#384=ITEM_DEFINED_TRANSFORMATION($,$,#11977,#12444);
#385=ITEM_DEFINED_TRANSFORMATION($,$,#11986,#12445);
#386=ITEM_DEFINED_TRANSFORMATION($,$,#11995,#12446);
#387=ITEM_DEFINED_TRANSFORMATION($,$,#12004,#12447);
#388=ITEM_DEFINED_TRANSFORMATION($,$,#12013,#12448);
#389=ITEM_DEFINED_TRANSFORMATION($,$,#12035,#12449);
#390=ITEM_DEFINED_TRANSFORMATION($,$,#12057,#12450);
#391=ITEM_DEFINED_TRANSFORMATION($,$,#12079,#12451);
#392=ITEM_DEFINED_TRANSFORMATION($,$,#12101,#12452);
#393=ITEM_DEFINED_TRANSFORMATION($,$,#12101,#12453);
#394=ITEM_DEFINED_TRANSFORMATION($,$,#12101,#12454);
#395=ITEM_DEFINED_TRANSFORMATION($,$,#12101,#12455);
#396=ITEM_DEFINED_TRANSFORMATION($,$,#12101,#12456);
#397=ITEM_DEFINED_TRANSFORMATION($,$,#12101,#12457);
#398=ITEM_DEFINED_TRANSFORMATION($,$,#12101,#12458);
#399=ITEM_DEFINED_TRANSFORMATION($,$,#12101,#12459);
#400=ITEM_DEFINED_TRANSFORMATION($,$,#12127,#12460);
#401=ITEM_DEFINED_TRANSFORMATION($,$,#12127,#12461);
#402=ITEM_DEFINED_TRANSFORMATION($,$,#12127,#12462);
#403=ITEM_DEFINED_TRANSFORMATION($,$,#12127,#12463);
#404=ITEM_DEFINED_TRANSFORMATION($,$,#12153,#12464);
#405=ITEM_DEFINED_TRANSFORMATION($,$,#12415,#12465);
#406=ITEM_DEFINED_TRANSFORMATION($,$,#12415,#12466);
#407=ITEM_DEFINED_TRANSFORMATION($,$,#12415,#12467);
#408=ITEM_DEFINED_TRANSFORMATION($,$,#12281,#12468);
#409=ITEM_DEFINED_TRANSFORMATION($,$,#12415,#12469);
#410=ITEM_DEFINED_TRANSFORMATION($,$,#12415,#12470);
#411=ITEM_DEFINED_TRANSFORMATION($,$,#12415,#12471);
#412=ITEM_DEFINED_TRANSFORMATION($,$,#12153,#12472);
#413=ITEM_DEFINED_TRANSFORMATION($,$,#12415,#12473);
#414=ITEM_DEFINED_TRANSFORMATION($,$,#12415,#12474);
#415=ITEM_DEFINED_TRANSFORMATION($,$,#12415,#12475);
#416=ITEM_DEFINED_TRANSFORMATION($,$,#12281,#12476);
#417=ITEM_DEFINED_TRANSFORMATION($,$,#12415,#12477);
#418=ITEM_DEFINED_TRANSFORMATION($,$,#12415,#12478);
#419=ITEM_DEFINED_TRANSFORMATION($,$,#12415,#12479);
#420=ITEM_DEFINED_TRANSFORMATION($,$,#12481,#12957);
#421=ITEM_DEFINED_TRANSFORMATION($,$,#12494,#12958);
#422=ITEM_DEFINED_TRANSFORMATION($,$,#12503,#12959);
#423=ITEM_DEFINED_TRANSFORMATION($,$,#12512,#12960);
#424=ITEM_DEFINED_TRANSFORMATION($,$,#12527,#12961);
#425=ITEM_DEFINED_TRANSFORMATION($,$,#12536,#12962);
#426=ITEM_DEFINED_TRANSFORMATION($,$,#12551,#12963);
#427=ITEM_DEFINED_TRANSFORMATION($,$,#12560,#12964);
#428=ITEM_DEFINED_TRANSFORMATION($,$,#12653,#12965);
#429=ITEM_DEFINED_TRANSFORMATION($,$,#12940,#12966);
#430=ITEM_DEFINED_TRANSFORMATION($,$,#12940,#12967);
#431=ITEM_DEFINED_TRANSFORMATION($,$,#12677,#12968);
#432=ITEM_DEFINED_TRANSFORMATION($,$,#12690,#12969);
#433=ITEM_DEFINED_TRANSFORMATION($,$,#12699,#12970);
#434=ITEM_DEFINED_TRANSFORMATION($,$,#12708,#12971);
#435=ITEM_DEFINED_TRANSFORMATION($,$,#12723,#12972);
#436=ITEM_DEFINED_TRANSFORMATION($,$,#12732,#12973);
#437=ITEM_DEFINED_TRANSFORMATION($,$,#12747,#12974);
#438=ITEM_DEFINED_TRANSFORMATION($,$,#12756,#12975);
#439=ITEM_DEFINED_TRANSFORMATION($,$,#12929,#12976);
#440=ITEM_DEFINED_TRANSFORMATION($,$,#12940,#12977);
#441=ITEM_DEFINED_TRANSFORMATION($,$,#12940,#12978);
#442=ITEM_DEFINED_TRANSFORMATION($,$,#11807,#12979);
#443=ITEM_DEFINED_TRANSFORMATION($,$,#12480,#12980);
#444=ITEM_DEFINED_TRANSFORMATION($,$,#12676,#12981);
#445=(
REPRESENTATION_RELATIONSHIP($,$,#54102,#54101)
REPRESENTATION_RELATIONSHIP_WITH_TRANSFORMATION(#371)
SHAPE_REPRESENTATION_RELATIONSHIP()
);
#446=(
REPRESENTATION_RELATIONSHIP($,$,#54103,#54101)
REPRESENTATION_RELATIONSHIP_WITH_TRANSFORMATION(#372)
SHAPE_REPRESENTATION_RELATIONSHIP()
);
#447=(
REPRESENTATION_RELATIONSHIP($,$,#54104,#54101)
REPRESENTATION_RELATIONSHIP_WITH_TRANSFORMATION(#373)
SHAPE_REPRESENTATION_RELATIONSHIP()
);
#448=(
REPRESENTATION_RELATIONSHIP($,$,#54105,#54101)
REPRESENTATION_RELATIONSHIP_WITH_TRANSFORMATION(#374)
SHAPE_REPRESENTATION_RELATIONSHIP()
);
#449=(
REPRESENTATION_RELATIONSHIP($,$,#54106,#54101)
REPRESENTATION_RELATIONSHIP_WITH_TRANSFORMATION(#375)
SHAPE_REPRESENTATION_RELATIONSHIP()
);
#450=(
REPRESENTATION_RELATIONSHIP($,$,#54108,#54107)
REPRESENTATION_RELATIONSHIP_WITH_TRANSFORMATION(#376)
SHAPE_REPRESENTATION_RELATIONSHIP()
);
#451=(
REPRESENTATION_RELATIONSHIP($,$,#54109,#54107)
REPRESENTATION_RELATIONSHIP_WITH_TRANSFORMATION(#377)
SHAPE_REPRESENTATION_RELATIONSHIP()
);
#452=(
REPRESENTATION_RELATIONSHIP($,$,#54110,#54107)
REPRESENTATION_RELATIONSHIP_WITH_TRANSFORMATION(#378)
SHAPE_REPRESENTATION_RELATIONSHIP()
);
#453=(
REPRESENTATION_RELATIONSHIP($,$,#54111,#54107)
REPRESENTATION_RELATIONSHIP_WITH_TRANSFORMATION(#379)
SHAPE_REPRESENTATION_RELATIONSHIP()
);
#454=(
REPRESENTATION_RELATIONSHIP($,$,#54112,#54107)
REPRESENTATION_RELATIONSHIP_WITH_TRANSFORMATION(#380)
SHAPE_REPRESENTATION_RELATIONSHIP()
);
#455=(
REPRESENTATION_RELATIONSHIP($,$,#54088,#54087)
REPRESENTATION_RELATIONSHIP_WITH_TRANSFORMATION(#381)
SHAPE_REPRESENTATION_RELATIONSHIP()
);
#456=(
REPRESENTATION_RELATIONSHIP($,$,#54089,#54087)
REPRESENTATION_RELATIONSHIP_WITH_TRANSFORMATION(#382)
SHAPE_REPRESENTATION_RELATIONSHIP()
);
#457=(
REPRESENTATION_RELATIONSHIP($,$,#54090,#54087)
REPRESENTATION_RELATIONSHIP_WITH_TRANSFORMATION(#383)
SHAPE_REPRESENTATION_RELATIONSHIP()
);
#458=(
REPRESENTATION_RELATIONSHIP($,$,#54091,#54087)
REPRESENTATION_RELATIONSHIP_WITH_TRANSFORMATION(#384)
SHAPE_REPRESENTATION_RELATIONSHIP()
);
#459=(
REPRESENTATION_RELATIONSHIP($,$,#54092,#54087)
REPRESENTATION_RELATIONSHIP_WITH_TRANSFORMATION(#385)
SHAPE_REPRESENTATION_RELATIONSHIP()
);
#460=(
REPRESENTATION_RELATIONSHIP($,$,#54093,#54087)
REPRESENTATION_RELATIONSHIP_WITH_TRANSFORMATION(#386)
SHAPE_REPRESENTATION_RELATIONSHIP()
);
#461=(
REPRESENTATION_RELATIONSHIP($,$,#54094,#54087)
REPRESENTATION_RELATIONSHIP_WITH_TRANSFORMATION(#387)
SHAPE_REPRESENTATION_RELATIONSHIP()
);
#462=(
REPRESENTATION_RELATIONSHIP($,$,#54095,#54087)
REPRESENTATION_RELATIONSHIP_WITH_TRANSFORMATION(#388)
SHAPE_REPRESENTATION_RELATIONSHIP()
);
#463=(
REPRESENTATION_RELATIONSHIP($,$,#54096,#54087)
REPRESENTATION_RELATIONSHIP_WITH_TRANSFORMATION(#389)
SHAPE_REPRESENTATION_RELATIONSHIP()
);
#464=(
REPRESENTATION_RELATIONSHIP($,$,#54097,#54087)
REPRESENTATION_RELATIONSHIP_WITH_TRANSFORMATION(#390)
SHAPE_REPRESENTATION_RELATIONSHIP()
);
#465=(
REPRESENTATION_RELATIONSHIP($,$,#54098,#54087)
REPRESENTATION_RELATIONSHIP_WITH_TRANSFORMATION(#391)
SHAPE_REPRESENTATION_RELATIONSHIP()
);
#466=(
REPRESENTATION_RELATIONSHIP($,$,#54099,#54087)
REPRESENTATION_RELATIONSHIP_WITH_TRANSFORMATION(#392)
SHAPE_REPRESENTATION_RELATIONSHIP()
);
#467=(
REPRESENTATION_RELATIONSHIP($,$,#54099,#54087)
REPRESENTATION_RELATIONSHIP_WITH_TRANSFORMATION(#393)
SHAPE_REPRESENTATION_RELATIONSHIP()
);
#468=(
REPRESENTATION_RELATIONSHIP($,$,#54099,#54087)
REPRESENTATION_RELATIONSHIP_WITH_TRANSFORMATION(#394)
SHAPE_REPRESENTATION_RELATIONSHIP()
);
#469=(
REPRESENTATION_RELATIONSHIP($,$,#54099,#54087)
REPRESENTATION_RELATIONSHIP_WITH_TRANSFORMATION(#395)
SHAPE_REPRESENTATION_RELATIONSHIP()
);
#470=(
REPRESENTATION_RELATIONSHIP($,$,#54099,#54087)
REPRESENTATION_RELATIONSHIP_WITH_TRANSFORMATION(#396)
SHAPE_REPRESENTATION_RELATIONSHIP()
);
#471=(
REPRESENTATION_RELATIONSHIP($,$,#54099,#54087)
REPRESENTATION_RELATIONSHIP_WITH_TRANSFORMATION(#397)
SHAPE_REPRESENTATION_RELATIONSHIP()
);
#472=(
REPRESENTATION_RELATIONSHIP($,$,#54099,#54087)
REPRESENTATION_RELATIONSHIP_WITH_TRANSFORMATION(#398)
SHAPE_REPRESENTATION_RELATIONSHIP()
);
#473=(
REPRESENTATION_RELATIONSHIP($,$,#54099,#54087)
REPRESENTATION_RELATIONSHIP_WITH_TRANSFORMATION(#399)
SHAPE_REPRESENTATION_RELATIONSHIP()
);
#474=(
REPRESENTATION_RELATIONSHIP($,$,#54100,#54087)
REPRESENTATION_RELATIONSHIP_WITH_TRANSFORMATION(#400)
SHAPE_REPRESENTATION_RELATIONSHIP()
);
#475=(
REPRESENTATION_RELATIONSHIP($,$,#54100,#54087)
REPRESENTATION_RELATIONSHIP_WITH_TRANSFORMATION(#401)
SHAPE_REPRESENTATION_RELATIONSHIP()
);
#476=(
REPRESENTATION_RELATIONSHIP($,$,#54100,#54087)
REPRESENTATION_RELATIONSHIP_WITH_TRANSFORMATION(#402)
SHAPE_REPRESENTATION_RELATIONSHIP()
);
#477=(
REPRESENTATION_RELATIONSHIP($,$,#54100,#54087)
REPRESENTATION_RELATIONSHIP_WITH_TRANSFORMATION(#403)
SHAPE_REPRESENTATION_RELATIONSHIP()
);
#478=(
REPRESENTATION_RELATIONSHIP($,$,#54101,#54087)
REPRESENTATION_RELATIONSHIP_WITH_TRANSFORMATION(#404)
SHAPE_REPRESENTATION_RELATIONSHIP()
);
#479=(
REPRESENTATION_RELATIONSHIP($,$,#54113,#54087)
REPRESENTATION_RELATIONSHIP_WITH_TRANSFORMATION(#405)
SHAPE_REPRESENTATION_RELATIONSHIP()
);
#480=(
REPRESENTATION_RELATIONSHIP($,$,#54113,#54087)
REPRESENTATION_RELATIONSHIP_WITH_TRANSFORMATION(#406)
SHAPE_REPRESENTATION_RELATIONSHIP()
);
#481=(
REPRESENTATION_RELATIONSHIP($,$,#54113,#54087)
REPRESENTATION_RELATIONSHIP_WITH_TRANSFORMATION(#407)
SHAPE_REPRESENTATION_RELATIONSHIP()
);
#482=(
REPRESENTATION_RELATIONSHIP($,$,#54107,#54087)
REPRESENTATION_RELATIONSHIP_WITH_TRANSFORMATION(#408)
SHAPE_REPRESENTATION_RELATIONSHIP()
);
#483=(
REPRESENTATION_RELATIONSHIP($,$,#54113,#54087)
REPRESENTATION_RELATIONSHIP_WITH_TRANSFORMATION(#409)
SHAPE_REPRESENTATION_RELATIONSHIP()
);
#484=(
REPRESENTATION_RELATIONSHIP($,$,#54113,#54087)
REPRESENTATION_RELATIONSHIP_WITH_TRANSFORMATION(#410)
SHAPE_REPRESENTATION_RELATIONSHIP()
);
#485=(
REPRESENTATION_RELATIONSHIP($,$,#54113,#54087)
REPRESENTATION_RELATIONSHIP_WITH_TRANSFORMATION(#411)
SHAPE_REPRESENTATION_RELATIONSHIP()
);
#486=(
REPRESENTATION_RELATIONSHIP($,$,#54101,#54087)
REPRESENTATION_RELATIONSHIP_WITH_TRANSFORMATION(#412)
SHAPE_REPRESENTATION_RELATIONSHIP()
);
#487=(
REPRESENTATION_RELATIONSHIP($,$,#54113,#54087)
REPRESENTATION_RELATIONSHIP_WITH_TRANSFORMATION(#413)
SHAPE_REPRESENTATION_RELATIONSHIP()
);
#488=(
REPRESENTATION_RELATIONSHIP($,$,#54113,#54087)
REPRESENTATION_RELATIONSHIP_WITH_TRANSFORMATION(#414)
SHAPE_REPRESENTATION_RELATIONSHIP()
);
#489=(
REPRESENTATION_RELATIONSHIP($,$,#54113,#54087)
REPRESENTATION_RELATIONSHIP_WITH_TRANSFORMATION(#415)
SHAPE_REPRESENTATION_RELATIONSHIP()
);
#490=(
REPRESENTATION_RELATIONSHIP($,$,#54107,#54087)
REPRESENTATION_RELATIONSHIP_WITH_TRANSFORMATION(#416)
SHAPE_REPRESENTATION_RELATIONSHIP()
);
#491=(
REPRESENTATION_RELATIONSHIP($,$,#54113,#54087)
REPRESENTATION_RELATIONSHIP_WITH_TRANSFORMATION(#417)
SHAPE_REPRESENTATION_RELATIONSHIP()
);
#492=(
REPRESENTATION_RELATIONSHIP($,$,#54113,#54087)
REPRESENTATION_RELATIONSHIP_WITH_TRANSFORMATION(#418)
SHAPE_REPRESENTATION_RELATIONSHIP()
);
#493=(
REPRESENTATION_RELATIONSHIP($,$,#54113,#54087)
REPRESENTATION_RELATIONSHIP_WITH_TRANSFORMATION(#419)
SHAPE_REPRESENTATION_RELATIONSHIP()
);
#494=(
REPRESENTATION_RELATIONSHIP($,$,#54115,#54114)
REPRESENTATION_RELATIONSHIP_WITH_TRANSFORMATION(#420)
SHAPE_REPRESENTATION_RELATIONSHIP()
);
#495=(
REPRESENTATION_RELATIONSHIP($,$,#54116,#54114)
REPRESENTATION_RELATIONSHIP_WITH_TRANSFORMATION(#421)
SHAPE_REPRESENTATION_RELATIONSHIP()
);
#496=(
REPRESENTATION_RELATIONSHIP($,$,#54117,#54114)
REPRESENTATION_RELATIONSHIP_WITH_TRANSFORMATION(#422)
SHAPE_REPRESENTATION_RELATIONSHIP()
);
#497=(
REPRESENTATION_RELATIONSHIP($,$,#54118,#54114)
REPRESENTATION_RELATIONSHIP_WITH_TRANSFORMATION(#423)
SHAPE_REPRESENTATION_RELATIONSHIP()
);
#498=(
REPRESENTATION_RELATIONSHIP($,$,#54119,#54114)
REPRESENTATION_RELATIONSHIP_WITH_TRANSFORMATION(#424)
SHAPE_REPRESENTATION_RELATIONSHIP()
);
#499=(
REPRESENTATION_RELATIONSHIP($,$,#54120,#54114)
REPRESENTATION_RELATIONSHIP_WITH_TRANSFORMATION(#425)
SHAPE_REPRESENTATION_RELATIONSHIP()
);
#500=(
REPRESENTATION_RELATIONSHIP($,$,#54121,#54114)
REPRESENTATION_RELATIONSHIP_WITH_TRANSFORMATION(#426)
SHAPE_REPRESENTATION_RELATIONSHIP()
);
#501=(
REPRESENTATION_RELATIONSHIP($,$,#54122,#54114)
REPRESENTATION_RELATIONSHIP_WITH_TRANSFORMATION(#427)
SHAPE_REPRESENTATION_RELATIONSHIP()
);
#502=(
REPRESENTATION_RELATIONSHIP($,$,#54123,#54114)
REPRESENTATION_RELATIONSHIP_WITH_TRANSFORMATION(#428)
SHAPE_REPRESENTATION_RELATIONSHIP()
);
#503=(
REPRESENTATION_RELATIONSHIP($,$,#54134,#54114)
REPRESENTATION_RELATIONSHIP_WITH_TRANSFORMATION(#429)
SHAPE_REPRESENTATION_RELATIONSHIP()
);
#504=(
REPRESENTATION_RELATIONSHIP($,$,#54134,#54114)
REPRESENTATION_RELATIONSHIP_WITH_TRANSFORMATION(#430)
SHAPE_REPRESENTATION_RELATIONSHIP()
);
#505=(
REPRESENTATION_RELATIONSHIP($,$,#54125,#54124)
REPRESENTATION_RELATIONSHIP_WITH_TRANSFORMATION(#431)
SHAPE_REPRESENTATION_RELATIONSHIP()
);
#506=(
REPRESENTATION_RELATIONSHIP($,$,#54126,#54124)
REPRESENTATION_RELATIONSHIP_WITH_TRANSFORMATION(#432)
SHAPE_REPRESENTATION_RELATIONSHIP()
);
#507=(
REPRESENTATION_RELATIONSHIP($,$,#54127,#54124)
REPRESENTATION_RELATIONSHIP_WITH_TRANSFORMATION(#433)
SHAPE_REPRESENTATION_RELATIONSHIP()
);
#508=(
REPRESENTATION_RELATIONSHIP($,$,#54128,#54124)
REPRESENTATION_RELATIONSHIP_WITH_TRANSFORMATION(#434)
SHAPE_REPRESENTATION_RELATIONSHIP()
);
#509=(
REPRESENTATION_RELATIONSHIP($,$,#54129,#54124)
REPRESENTATION_RELATIONSHIP_WITH_TRANSFORMATION(#435)
SHAPE_REPRESENTATION_RELATIONSHIP()
);
#510=(
REPRESENTATION_RELATIONSHIP($,$,#54130,#54124)
REPRESENTATION_RELATIONSHIP_WITH_TRANSFORMATION(#436)
SHAPE_REPRESENTATION_RELATIONSHIP()
);
#511=(
REPRESENTATION_RELATIONSHIP($,$,#54131,#54124)
REPRESENTATION_RELATIONSHIP_WITH_TRANSFORMATION(#437)
SHAPE_REPRESENTATION_RELATIONSHIP()
);
#512=(
REPRESENTATION_RELATIONSHIP($,$,#54132,#54124)
REPRESENTATION_RELATIONSHIP_WITH_TRANSFORMATION(#438)
SHAPE_REPRESENTATION_RELATIONSHIP()
);
#513=(
REPRESENTATION_RELATIONSHIP($,$,#54133,#54124)
REPRESENTATION_RELATIONSHIP_WITH_TRANSFORMATION(#439)
SHAPE_REPRESENTATION_RELATIONSHIP()
);
#514=(
REPRESENTATION_RELATIONSHIP($,$,#54134,#54124)
REPRESENTATION_RELATIONSHIP_WITH_TRANSFORMATION(#440)
SHAPE_REPRESENTATION_RELATIONSHIP()
);
#515=(
REPRESENTATION_RELATIONSHIP($,$,#54134,#54124)
REPRESENTATION_RELATIONSHIP_WITH_TRANSFORMATION(#441)
SHAPE_REPRESENTATION_RELATIONSHIP()
);
#516=(
REPRESENTATION_RELATIONSHIP($,$,#54087,#54086)
REPRESENTATION_RELATIONSHIP_WITH_TRANSFORMATION(#442)
SHAPE_REPRESENTATION_RELATIONSHIP()
);
#517=(
REPRESENTATION_RELATIONSHIP($,$,#54114,#54086)
REPRESENTATION_RELATIONSHIP_WITH_TRANSFORMATION(#443)
SHAPE_REPRESENTATION_RELATIONSHIP()
);
#518=(
REPRESENTATION_RELATIONSHIP($,$,#54124,#54086)
REPRESENTATION_RELATIONSHIP_WITH_TRANSFORMATION(#444)
SHAPE_REPRESENTATION_RELATIONSHIP()
);
#519=CONTEXT_DEPENDENT_SHAPE_REPRESENTATION(#445,#53984);
#520=CONTEXT_DEPENDENT_SHAPE_REPRESENTATION(#446,#53985);
#521=CONTEXT_DEPENDENT_SHAPE_REPRESENTATION(#447,#53986);
#522=CONTEXT_DEPENDENT_SHAPE_REPRESENTATION(#448,#53987);
#523=CONTEXT_DEPENDENT_SHAPE_REPRESENTATION(#449,#53988);
#524=CONTEXT_DEPENDENT_SHAPE_REPRESENTATION(#450,#53995);
#525=CONTEXT_DEPENDENT_SHAPE_REPRESENTATION(#451,#53996);
#526=CONTEXT_DEPENDENT_SHAPE_REPRESENTATION(#452,#53997);
#527=CONTEXT_DEPENDENT_SHAPE_REPRESENTATION(#453,#53998);
#528=CONTEXT_DEPENDENT_SHAPE_REPRESENTATION(#454,#53999);
#529=CONTEXT_DEPENDENT_SHAPE_REPRESENTATION(#455,#54001);
#530=CONTEXT_DEPENDENT_SHAPE_REPRESENTATION(#456,#54002);
#531=CONTEXT_DEPENDENT_SHAPE_REPRESENTATION(#457,#54003);
#532=CONTEXT_DEPENDENT_SHAPE_REPRESENTATION(#458,#54004);
#533=CONTEXT_DEPENDENT_SHAPE_REPRESENTATION(#459,#54005);
#534=CONTEXT_DEPENDENT_SHAPE_REPRESENTATION(#460,#54006);
#535=CONTEXT_DEPENDENT_SHAPE_REPRESENTATION(#461,#54007);
#536=CONTEXT_DEPENDENT_SHAPE_REPRESENTATION(#462,#54008);
#537=CONTEXT_DEPENDENT_SHAPE_REPRESENTATION(#463,#54009);
#538=CONTEXT_DEPENDENT_SHAPE_REPRESENTATION(#464,#54010);
#539=CONTEXT_DEPENDENT_SHAPE_REPRESENTATION(#465,#54011);
#540=CONTEXT_DEPENDENT_SHAPE_REPRESENTATION(#466,#54012);
#541=CONTEXT_DEPENDENT_SHAPE_REPRESENTATION(#467,#54013);
#542=CONTEXT_DEPENDENT_SHAPE_REPRESENTATION(#468,#54014);
#543=CONTEXT_DEPENDENT_SHAPE_REPRESENTATION(#469,#54015);
#544=CONTEXT_DEPENDENT_SHAPE_REPRESENTATION(#470,#54016);
#545=CONTEXT_DEPENDENT_SHAPE_REPRESENTATION(#471,#54017);
#546=CONTEXT_DEPENDENT_SHAPE_REPRESENTATION(#472,#54018);
#547=CONTEXT_DEPENDENT_SHAPE_REPRESENTATION(#473,#54019);
#548=CONTEXT_DEPENDENT_SHAPE_REPRESENTATION(#474,#54020);
#549=CONTEXT_DEPENDENT_SHAPE_REPRESENTATION(#475,#54021);
#550=CONTEXT_DEPENDENT_SHAPE_REPRESENTATION(#476,#54022);
#551=CONTEXT_DEPENDENT_SHAPE_REPRESENTATION(#477,#54023);
#552=CONTEXT_DEPENDENT_SHAPE_REPRESENTATION(#478,#54024);
#553=CONTEXT_DEPENDENT_SHAPE_REPRESENTATION(#479,#54025);
#554=CONTEXT_DEPENDENT_SHAPE_REPRESENTATION(#480,#54026);
#555=CONTEXT_DEPENDENT_SHAPE_REPRESENTATION(#481,#54027);
#556=CONTEXT_DEPENDENT_SHAPE_REPRESENTATION(#482,#54028);
#557=CONTEXT_DEPENDENT_SHAPE_REPRESENTATION(#483,#54029);
#558=CONTEXT_DEPENDENT_SHAPE_REPRESENTATION(#484,#54030);
#559=CONTEXT_DEPENDENT_SHAPE_REPRESENTATION(#485,#54031);
#560=CONTEXT_DEPENDENT_SHAPE_REPRESENTATION(#486,#54032);
#561=CONTEXT_DEPENDENT_SHAPE_REPRESENTATION(#487,#54033);
#562=CONTEXT_DEPENDENT_SHAPE_REPRESENTATION(#488,#54034);
#563=CONTEXT_DEPENDENT_SHAPE_REPRESENTATION(#489,#54035);
#564=CONTEXT_DEPENDENT_SHAPE_REPRESENTATION(#490,#54036);
#565=CONTEXT_DEPENDENT_SHAPE_REPRESENTATION(#491,#54037);
#566=CONTEXT_DEPENDENT_SHAPE_REPRESENTATION(#492,#54038);
#567=CONTEXT_DEPENDENT_SHAPE_REPRESENTATION(#493,#54039);
#568=CONTEXT_DEPENDENT_SHAPE_REPRESENTATION(#494,#54061);
#569=CONTEXT_DEPENDENT_SHAPE_REPRESENTATION(#495,#54062);
#570=CONTEXT_DEPENDENT_SHAPE_REPRESENTATION(#496,#54063);
#571=CONTEXT_DEPENDENT_SHAPE_REPRESENTATION(#497,#54064);
#572=CONTEXT_DEPENDENT_SHAPE_REPRESENTATION(#498,#54065);
#573=CONTEXT_DEPENDENT_SHAPE_REPRESENTATION(#499,#54066);
#574=CONTEXT_DEPENDENT_SHAPE_REPRESENTATION(#500,#54067);
#575=CONTEXT_DEPENDENT_SHAPE_REPRESENTATION(#501,#54068);
#576=CONTEXT_DEPENDENT_SHAPE_REPRESENTATION(#502,#54069);
#577=CONTEXT_DEPENDENT_SHAPE_REPRESENTATION(#503,#54070);
#578=CONTEXT_DEPENDENT_SHAPE_REPRESENTATION(#504,#54071);
#579=CONTEXT_DEPENDENT_SHAPE_REPRESENTATION(#505,#54072);
#580=CONTEXT_DEPENDENT_SHAPE_REPRESENTATION(#506,#54073);
#581=CONTEXT_DEPENDENT_SHAPE_REPRESENTATION(#507,#54074);
#582=CONTEXT_DEPENDENT_SHAPE_REPRESENTATION(#508,#54075);
#583=CONTEXT_DEPENDENT_SHAPE_REPRESENTATION(#509,#54076);
#584=CONTEXT_DEPENDENT_SHAPE_REPRESENTATION(#510,#54077);
#585=CONTEXT_DEPENDENT_SHAPE_REPRESENTATION(#511,#54078);
#586=CONTEXT_DEPENDENT_SHAPE_REPRESENTATION(#512,#54079);
#587=CONTEXT_DEPENDENT_SHAPE_REPRESENTATION(#513,#54080);
#588=CONTEXT_DEPENDENT_SHAPE_REPRESENTATION(#514,#54081);
#589=CONTEXT_DEPENDENT_SHAPE_REPRESENTATION(#515,#54082);
#590=CONTEXT_DEPENDENT_SHAPE_REPRESENTATION(#516,#54083);
#591=CONTEXT_DEPENDENT_SHAPE_REPRESENTATION(#517,#54084);
#592=CONTEXT_DEPENDENT_SHAPE_REPRESENTATION(#518,#54085);
#593=NEXT_ASSEMBLY_USAGE_OCCURRENCE('Inner ring:1','Inner ring:1',
'Inner ring:1',#54151,#54152,'Inner ring:1');
#594=NEXT_ASSEMBLY_USAGE_OCCURRENCE('Outer ring:1','Outer ring:1',
'Outer ring:1',#54151,#54153,'Outer ring:1');
#595=NEXT_ASSEMBLY_USAGE_OCCURRENCE('Balls:1','Balls:1','Balls:1',#54151,
#54154,'Balls:1');
#596=NEXT_ASSEMBLY_USAGE_OCCURRENCE('Cage:1','Cage:1','Cage:1',#54151,#54155,
'Cage:1');
#597=NEXT_ASSEMBLY_USAGE_OCCURRENCE('Seals 2RS:1','Seals 2RS:1',
'Seals 2RS:1',#54151,#54156,'Seals 2RS:1');
#598=NEXT_ASSEMBLY_USAGE_OCCURRENCE('Inner ring (1):1',
'Inner ring (1):1','Inner ring (1):1',#54157,#54158,'Inner ring (1):1');
#599=NEXT_ASSEMBLY_USAGE_OCCURRENCE('Outer ring (1):1',
'Outer ring (1):1','Outer ring (1):1',#54157,#54159,'Outer ring (1):1');
#600=NEXT_ASSEMBLY_USAGE_OCCURRENCE('Balls (1):1','Balls (1):1',
'Balls (1):1',#54157,#54160,'Balls (1):1');
#601=NEXT_ASSEMBLY_USAGE_OCCURRENCE('Cage (1):1','Cage (1):1',
'Cage (1):1',#54157,#54161,'Cage (1):1');
#602=NEXT_ASSEMBLY_USAGE_OCCURRENCE('Seals 2RS (1):1','Seals 2RS (1):1',
'Seals 2RS (1):1',#54157,#54162,'Seals 2RS (1):1');
#603=NEXT_ASSEMBLY_USAGE_OCCURRENCE('Base:1','Base:1','Base:1',#54137,#54138,
'Base:1');
#604=NEXT_ASSEMBLY_USAGE_OCCURRENCE('Front plate:1','Front plate:1',
'Front plate:1',#54137,#54139,'Front plate:1');
#605=NEXT_ASSEMBLY_USAGE_OCCURRENCE('Rear plate:1','Rear plate:1',
'Rear plate:1',#54137,#54140,'Rear plate:1');
#606=NEXT_ASSEMBLY_USAGE_OCCURRENCE('Frame spacer:1','Frame spacer:1',
'Frame spacer:1',#54137,#54141,'Frame spacer:1');
#607=NEXT_ASSEMBLY_USAGE_OCCURRENCE('Frame spacer (1):1',
'Frame spacer (1):1','Frame spacer (1):1',#54137,#54142,
'Frame spacer (1):1');
#608=NEXT_ASSEMBLY_USAGE_OCCURRENCE('Frame spacer (2):1',
'Frame spacer (2):1','Frame spacer (2):1',#54137,#54143,
'Frame spacer (2):1');
#609=NEXT_ASSEMBLY_USAGE_OCCURRENCE('Frame spacer (3):1',
'Frame spacer (3):1','Frame spacer (3):1',#54137,#54144,
'Frame spacer (3):1');
#610=NEXT_ASSEMBLY_USAGE_OCCURRENCE('Small bearing cap:1',
'Small bearing cap:1','Small bearing cap:1',#54137,#54145,
'Small bearing cap:1');
#611=NEXT_ASSEMBLY_USAGE_OCCURRENCE('Large bearing cap:1',
'Large bearing cap:1','Large bearing cap:1',#54137,#54146,
'Large bearing cap:1');
#612=NEXT_ASSEMBLY_USAGE_OCCURRENCE('Small bearing cap (1):1',
'Small bearing cap (1):1','Small bearing cap (1):1',#54137,#54147,
'Small bearing cap (1):1');
#613=NEXT_ASSEMBLY_USAGE_OCCURRENCE('Large bearing cap (1):1',
'Large bearing cap (1):1','Large bearing cap (1):1',#54137,#54148,
'Large bearing cap (1):1');
#614=NEXT_ASSEMBLY_USAGE_OCCURRENCE('Cap Screw - M5x20:2',
'Cap Screw - M5x20:2','Cap Screw - M5x20:2',#54137,#54149,
'Cap Screw - M5x20:2');
#615=NEXT_ASSEMBLY_USAGE_OCCURRENCE('Cap Screw - M5x20:3',
'Cap Screw - M5x20:3','Cap Screw - M5x20:3',#54137,#54149,
'Cap Screw - M5x20:3');
#616=NEXT_ASSEMBLY_USAGE_OCCURRENCE('Cap Screw - M5x20:4',
'Cap Screw - M5x20:4','Cap Screw - M5x20:4',#54137,#54149,
'Cap Screw - M5x20:4');
#617=NEXT_ASSEMBLY_USAGE_OCCURRENCE('Cap Screw - M5x20:5',
'Cap Screw - M5x20:5','Cap Screw - M5x20:5',#54137,#54149,
'Cap Screw - M5x20:5');
#618=NEXT_ASSEMBLY_USAGE_OCCURRENCE('Cap Screw - M5x20:6',
'Cap Screw - M5x20:6','Cap Screw - M5x20:6',#54137,#54149,
'Cap Screw - M5x20:6');
#619=NEXT_ASSEMBLY_USAGE_OCCURRENCE('Cap Screw - M5x20:7',
'Cap Screw - M5x20:7','Cap Screw - M5x20:7',#54137,#54149,
'Cap Screw - M5x20:7');
#620=NEXT_ASSEMBLY_USAGE_OCCURRENCE('Cap Screw - M5x20:8',
'Cap Screw - M5x20:8','Cap Screw - M5x20:8',#54137,#54149,
'Cap Screw - M5x20:8');
#621=NEXT_ASSEMBLY_USAGE_OCCURRENCE('Cap Screw - M5x20:9',
'Cap Screw - M5x20:9','Cap Screw - M5x20:9',#54137,#54149,
'Cap Screw - M5x20:9');
#622=NEXT_ASSEMBLY_USAGE_OCCURRENCE('Cap Screw - M6x25:2',
'Cap Screw - M6x25:2','Cap Screw - M6x25:2',#54137,#54150,
'Cap Screw - M6x25:2');
#623=NEXT_ASSEMBLY_USAGE_OCCURRENCE('Cap Screw - M6x25:3',
'Cap Screw - M6x25:3','Cap Screw - M6x25:3',#54137,#54150,
'Cap Screw - M6x25:3');
#624=NEXT_ASSEMBLY_USAGE_OCCURRENCE('Cap Screw - M6x25:4',
'Cap Screw - M6x25:4','Cap Screw - M6x25:4',#54137,#54150,
'Cap Screw - M6x25:4');
#625=NEXT_ASSEMBLY_USAGE_OCCURRENCE('Cap Screw - M6x25:5',
'Cap Screw - M6x25:5','Cap Screw - M6x25:5',#54137,#54150,
'Cap Screw - M6x25:5');
#626=NEXT_ASSEMBLY_USAGE_OCCURRENCE(
'Sealed Ball Bearing - 12 x 32 x 10 mm:2',
'Sealed Ball Bearing - 12 x 32 x 10 mm:2',
'Sealed Ball Bearing - 12 x 32 x 10 mm:2',#54137,#54151,
'Sealed Ball Bearing - 12 x 32 x 10 mm:2');
#627=NEXT_ASSEMBLY_USAGE_OCCURRENCE('Cap Screw - M4x16:2',
'Cap Screw - M4x16:2','Cap Screw - M4x16:2',#54137,#54163,
'Cap Screw - M4x16:2');
#628=NEXT_ASSEMBLY_USAGE_OCCURRENCE('Cap Screw - M4x16:3',
'Cap Screw - M4x16:3','Cap Screw - M4x16:3',#54137,#54163,
'Cap Screw - M4x16:3');
#629=NEXT_ASSEMBLY_USAGE_OCCURRENCE('Cap Screw - M4x16:4',
'Cap Screw - M4x16:4','Cap Screw - M4x16:4',#54137,#54163,
'Cap Screw - M4x16:4');
#630=NEXT_ASSEMBLY_USAGE_OCCURRENCE(
'Sealed Ball Bearing - 20 x 47 x 14 mm:2',
'Sealed Ball Bearing - 20 x 47 x 14 mm:2',
'Sealed Ball Bearing - 20 x 47 x 14 mm:2',#54137,#54157,
'Sealed Ball Bearing - 20 x 47 x 14 mm:2');
#631=NEXT_ASSEMBLY_USAGE_OCCURRENCE('Cap Screw - M4x16:5',
'Cap Screw - M4x16:5','Cap Screw - M4x16:5',#54137,#54163,
'Cap Screw - M4x16:5');
#632=NEXT_ASSEMBLY_USAGE_OCCURRENCE('Cap Screw - M4x16:6',
'Cap Screw - M4x16:6','Cap Screw - M4x16:6',#54137,#54163,
'Cap Screw - M4x16:6');
#633=NEXT_ASSEMBLY_USAGE_OCCURRENCE('Cap Screw - M4x16:7',
'Cap Screw - M4x16:7','Cap Screw - M4x16:7',#54137,#54163,
'Cap Screw - M4x16:7');
#634=NEXT_ASSEMBLY_USAGE_OCCURRENCE(
'Sealed Ball Bearing - 12 x 32 x 10 mm:3',
'Sealed Ball Bearing - 12 x 32 x 10 mm:3',
'Sealed Ball Bearing - 12 x 32 x 10 mm:3',#54137,#54151,
'Sealed Ball Bearing - 12 x 32 x 10 mm:3');
#635=NEXT_ASSEMBLY_USAGE_OCCURRENCE('Cap Screw - M4x16:8',
'Cap Screw - M4x16:8','Cap Screw - M4x16:8',#54137,#54163,
'Cap Screw - M4x16:8');
#636=NEXT_ASSEMBLY_USAGE_OCCURRENCE('Cap Screw - M4x16:9',
'Cap Screw - M4x16:9','Cap Screw - M4x16:9',#54137,#54163,
'Cap Screw - M4x16:9');
#637=NEXT_ASSEMBLY_USAGE_OCCURRENCE('Cap Screw - M4x16:10',
'Cap Screw - M4x16:10','Cap Screw - M4x16:10',#54137,#54163,
'Cap Screw - M4x16:10');
#638=NEXT_ASSEMBLY_USAGE_OCCURRENCE(
'Sealed Ball Bearing - 20 x 47 x 14 mm:3',
'Sealed Ball Bearing - 20 x 47 x 14 mm:3',
'Sealed Ball Bearing - 20 x 47 x 14 mm:3',#54137,#54157,
'Sealed Ball Bearing - 20 x 47 x 14 mm:3');
#639=NEXT_ASSEMBLY_USAGE_OCCURRENCE('Cap Screw - M4x16:11',
'Cap Screw - M4x16:11','Cap Screw - M4x16:11',#54137,#54163,
'Cap Screw - M4x16:11');
#640=NEXT_ASSEMBLY_USAGE_OCCURRENCE('Cap Screw - M4x16:12',
'Cap Screw - M4x16:12','Cap Screw - M4x16:12',#54137,#54163,
'Cap Screw - M4x16:12');
#641=NEXT_ASSEMBLY_USAGE_OCCURRENCE('Cap Screw - M4x16:13',
'Cap Screw - M4x16:13','Cap Screw - M4x16:13',#54137,#54163,
'Cap Screw - M4x16:13');
#642=NEXT_ASSEMBLY_USAGE_OCCURRENCE('Input shaft:1','Input shaft:1',
'Input shaft:1',#54164,#54165,'Input shaft:1');
#643=NEXT_ASSEMBLY_USAGE_OCCURRENCE('Input front sleeve:1',
'Input front sleeve:1','Input front sleeve:1',#54164,#54166,
'Input front sleeve:1');
#644=NEXT_ASSEMBLY_USAGE_OCCURRENCE('Input rear sleeve:1',
'Input rear sleeve:1','Input rear sleeve:1',#54164,#54167,
'Input rear sleeve:1');
#645=NEXT_ASSEMBLY_USAGE_OCCURRENCE('Input retaining collar:1',
'Input retaining collar:1','Input retaining collar:1',#54164,#54168,
'Input retaining collar:1');
#646=NEXT_ASSEMBLY_USAGE_OCCURRENCE('Input outer race sleeve:1',
'Input outer race sleeve:1','Input outer race sleeve:1',#54164,#54169,
'Input outer race sleeve:1');
#647=NEXT_ASSEMBLY_USAGE_OCCURRENCE('Input retaining collar (1):1',
'Input retaining collar (1):1','Input retaining collar (1):1',#54164,#54170,
'Input retaining collar (1):1');
#648=NEXT_ASSEMBLY_USAGE_OCCURRENCE('Input outer race sleeve (1):1',
'Input outer race sleeve (1):1','Input outer race sleeve (1):1',#54164,
#54171,'Input outer race sleeve (1):1');
#649=NEXT_ASSEMBLY_USAGE_OCCURRENCE(
'Spur Gear - Module 2, 20 Teeth, 12 mm Bore:2',
'Spur Gear - Module 2, 20 Teeth, 12 mm Bore:2',
'Spur Gear - Module 2, 20 Teeth, 12 mm Bore:2',#54164,#54172,
'Spur Gear - Module 2, 20 Teeth, 12 mm Bore:2');
#650=NEXT_ASSEMBLY_USAGE_OCCURRENCE('Parallel Key - 4x4x25:2',
'Parallel Key - 4x4x25:2','Parallel Key - 4x4x25:2',#54164,#54173,
'Parallel Key - 4x4x25:2');
#651=NEXT_ASSEMBLY_USAGE_OCCURRENCE('Socket Set Screw - M5x8:2',
'Socket Set Screw - M5x8:2','Socket Set Screw - M5x8:2',#54164,#54184,
'Socket Set Screw - M5x8:2');
#652=NEXT_ASSEMBLY_USAGE_OCCURRENCE('Socket Set Screw - M5x8:3',
'Socket Set Screw - M5x8:3','Socket Set Screw - M5x8:3',#54164,#54184,
'Socket Set Screw - M5x8:3');
#653=NEXT_ASSEMBLY_USAGE_OCCURRENCE('Output shaft:1','Output shaft:1',
'Output shaft:1',#54174,#54175,'Output shaft:1');
#654=NEXT_ASSEMBLY_USAGE_OCCURRENCE('Output front sleeve:1',
'Output front sleeve:1','Output front sleeve:1',#54174,#54176,
'Output front sleeve:1');
#655=NEXT_ASSEMBLY_USAGE_OCCURRENCE('Output rear sleeve:1',
'Output rear sleeve:1','Output rear sleeve:1',#54174,#54177,
'Output rear sleeve:1');
#656=NEXT_ASSEMBLY_USAGE_OCCURRENCE('Output retaining collar:1',
'Output retaining collar:1','Output retaining collar:1',#54174,#54178,
'Output retaining collar:1');
#657=NEXT_ASSEMBLY_USAGE_OCCURRENCE('Output outer race sleeve:1',
'Output outer race sleeve:1','Output outer race sleeve:1',#54174,#54179,
'Output outer race sleeve:1');
#658=NEXT_ASSEMBLY_USAGE_OCCURRENCE('Output retaining collar (1):1',
'Output retaining collar (1):1','Output retaining collar (1):1',#54174,
#54180,'Output retaining collar (1):1');
#659=NEXT_ASSEMBLY_USAGE_OCCURRENCE('Output outer race sleeve (1):1',
'Output outer race sleeve (1):1','Output outer race sleeve (1):1',#54174,
#54181,'Output outer race sleeve (1):1');
#660=NEXT_ASSEMBLY_USAGE_OCCURRENCE(
'Spur Gear - Module 2, 40 Teeth, 20 mm Bore:2',
'Spur Gear - Module 2, 40 Teeth, 20 mm Bore:2',
'Spur Gear - Module 2, 40 Teeth, 20 mm Bore:2',#54174,#54182,
'Spur Gear - Module 2, 40 Teeth, 20 mm Bore:2');
#661=NEXT_ASSEMBLY_USAGE_OCCURRENCE('Parallel key 6x6x28:2',
'Parallel key 6x6x28:2','Parallel key 6x6x28:2',#54174,#54183,
'Parallel key 6x6x28:2');
#662=NEXT_ASSEMBLY_USAGE_OCCURRENCE('Socket Set Screw - M5x8:4',
'Socket Set Screw - M5x8:4','Socket Set Screw - M5x8:4',#54174,#54184,
'Socket Set Screw - M5x8:4');
#663=NEXT_ASSEMBLY_USAGE_OCCURRENCE('Socket Set Screw - M5x8:5',
'Socket Set Screw - M5x8:5','Socket Set Screw - M5x8:5',#54174,#54184,
'Socket Set Screw - M5x8:5');
#664=NEXT_ASSEMBLY_USAGE_OCCURRENCE('Bearing frame:1','Bearing frame:1',
'Bearing frame:1',#54136,#54137,'Bearing frame:1');
#665=NEXT_ASSEMBLY_USAGE_OCCURRENCE('Input rotor:1','Input rotor:1',
'Input rotor:1',#54136,#54164,'Input rotor:1');
#666=NEXT_ASSEMBLY_USAGE_OCCURRENCE('Output rotor:1','Output rotor:1',
'Output rotor:1',#54136,#54174,'Output rotor:1');
#667=B_SPLINE_CURVE_WITH_KNOTS('',3,(#16802,#16803,#16804,#16805,#16806,
#16807,#16808,#16809,#16810,#16811,#16812,#16813,#16814,#16815,#16816,#16817,
#16818,#16819,#16820,#16821,#16822,#16823),.UNSPECIFIED.,.F.,.F.,(4,2,2,
2,2,2,2,2,2,2,4),(0.0591825211272536,0.157966726598481,0.236950089897721,
0.315933453196962,0.391576304923761,0.46721915665056,0.54286200837736,0.618504860104159,
0.697488223403399,0.77647158670264,0.875255792173867),.UNSPECIFIED.);
#668=B_SPLINE_CURVE_WITH_KNOTS('',3,(#16827,#16828,#16829,#16830,#16831,
#16832,#16833,#16834,#16835,#16836,#16837,#16838,#16839,#16840,#16841,#16842,
#16843,#16844,#16845,#16846,#16847,#16848),.UNSPECIFIED.,.F.,.F.,(4,2,2,
2,2,2,2,2,2,2,4),(0.0581119756758434,0.106553146291161,0.213106292582322,
0.30849933801665,0.386091982889075,0.4636846277615,0.541277272633925,0.61886991750635,
0.714262962940678,0.820816109231839,0.869257279847157),.UNSPECIFIED.);
#669=B_SPLINE_CURVE_WITH_KNOTS('',3,(#16854,#16855,#16856,#16857,#16858,
#16859,#16860,#16861,#16862,#16863,#16864,#16865,#16866,#16867,#16868,#16869,
#16870,#16871,#16872,#16873,#16874,#16875),.UNSPECIFIED.,.F.,.F.,(4,2,2,
2,2,2,2,2,2,2,4),(0.0581119756758434,0.106553146291161,0.213106292582322,
0.30849933801665,0.386091982889075,0.4636846277615,0.541277272633925,0.61886991750635,
0.714262962940679,0.820816109231839,0.869257279847157),.UNSPECIFIED.);
#670=B_SPLINE_CURVE_WITH_KNOTS('',3,(#16879,#16880,#16881,#16882,#16883,
#16884,#16885,#16886,#16887,#16888,#16889,#16890,#16891,#16892,#16893,#16894,
#16895,#16896,#16897,#16898,#16899,#16900),.UNSPECIFIED.,.F.,.F.,(4,2,2,
2,2,2,2,2,2,2,4),(0.0581119756758433,0.106553146291161,0.213106292582322,
0.308499338016649,0.386091982889075,0.4636846277615,0.541277272633925,0.61886991750635,
0.714262962940678,0.820816109231839,0.869257279847157),.UNSPECIFIED.);
#671=B_SPLINE_CURVE_WITH_KNOTS('',3,(#16909,#16910,#16911,#16912,#16913,
#16914,#16915,#16916,#16917,#16918,#16919,#16920,#16921,#16922,#16923,#16924,
#16925,#16926,#16927,#16928,#16929,#16930),.UNSPECIFIED.,.F.,.F.,(4,2,2,
2,2,2,2,2,2,2,4),(0.0581119756758433,0.106553146291161,0.213106292582322,
0.30849933801665,0.386091982889075,0.4636846277615,0.541277272633925,0.61886991750635,
0.714262962940678,0.820816109231839,0.869257279847157),.UNSPECIFIED.);
#672=B_SPLINE_CURVE_WITH_KNOTS('',3,(#16934,#16935,#16936,#16937,#16938,
#16939,#16940,#16941,#16942,#16943,#16944,#16945,#16946,#16947,#16948,#16949,
#16950,#16951,#16952,#16953,#16954,#16955),.UNSPECIFIED.,.F.,.F.,(4,2,2,
2,2,2,2,2,2,2,4),(0.0581119756758434,0.106553146291161,0.213106292582322,
0.30849933801665,0.386091982889075,0.4636846277615,0.541277272633925,0.61886991750635,
0.714262962940678,0.820816109231839,0.869257279847157),.UNSPECIFIED.);
#673=B_SPLINE_CURVE_WITH_KNOTS('',3,(#16959,#16960,#16961,#16962,#16963,
#16964,#16965,#16966,#16967,#16968,#16969,#16970,#16971,#16972,#16973,#16974,
#16975,#16976,#16977,#16978,#16979,#16980),.UNSPECIFIED.,.F.,.F.,(4,2,2,
2,2,2,2,2,2,2,4),(0.0581119756758434,0.106553146291161,0.213106292582322,
0.30849933801665,0.386091982889075,0.4636846277615,0.541277272633925,0.61886991750635,
0.714262962940678,0.820816109231839,0.869257279847157),.UNSPECIFIED.);
#674=B_SPLINE_CURVE_WITH_KNOTS('',3,(#16984,#16985,#16986,#16987,#16988,
#16989,#16990,#16991,#16992,#16993,#16994,#16995,#16996,#16997,#16998,#16999,
#17000,#17001,#17002,#17003,#17004,#17005),.UNSPECIFIED.,.F.,.F.,(4,2,2,
2,2,2,2,2,2,2,4),(0.0581119756758433,0.106553146291161,0.213106292582322,
0.30849933801665,0.386091982889075,0.4636846277615,0.541277272633925,0.61886991750635,
0.714262962940678,0.820816109231839,0.869257279847157),.UNSPECIFIED.);
#675=B_SPLINE_CURVE_WITH_KNOTS('',3,(#17013,#17014,#17015,#17016,#17017,
#17018,#17019,#17020,#17021,#17022,#17023,#17024,#17025,#17026,#17027,#17028,
#17029,#17030,#17031,#17032,#17033,#17034),.UNSPECIFIED.,.F.,.F.,(4,2,2,
2,2,2,2,2,2,2,4),(0.0591825211272536,0.157966726598481,0.236950089897721,
0.315933453196962,0.391576304923761,0.467219156650561,0.54286200837736,
0.618504860104159,0.697488223403399,0.77647158670264,0.875255792173867),
 .UNSPECIFIED.);
#676=B_SPLINE_CURVE_WITH_KNOTS('',3,(#17042,#17043,#17044,#17045,#17046,
#17047,#17048,#17049,#17050,#17051,#17052,#17053,#17054,#17055,#17056,#17057,
#17058,#17059,#17060,#17061,#17062,#17063),.UNSPECIFIED.,.F.,.F.,(4,2,2,
2,2,2,2,2,2,2,4),(0.0591825211272536,0.157966726598481,0.236950089897722,
0.315933453196962,0.391576304923761,0.467219156650561,0.54286200837736,
0.618504860104159,0.697488223403399,0.77647158670264,0.875255792173867),
 .UNSPECIFIED.);
#677=B_SPLINE_CURVE_WITH_KNOTS('',3,(#17073,#17074,#17075,#17076,#17077,
#17078,#17079,#17080,#17081,#17082,#17083,#17084,#17085,#17086,#17087,#17088,
#17089,#17090,#17091,#17092,#17093,#17094),.UNSPECIFIED.,.F.,.F.,(4,2,2,
2,2,2,2,2,2,2,4),(0.0591825211272536,0.157966726598481,0.236950089897721,
0.315933453196962,0.391576304923761,0.46721915665056,0.54286200837736,0.618504860104159,
0.697488223403399,0.77647158670264,0.875255792173867),.UNSPECIFIED.);
#678=B_SPLINE_CURVE_WITH_KNOTS('',3,(#17102,#17103,#17104,#17105,#17106,
#17107,#17108,#17109,#17110,#17111,#17112,#17113,#17114,#17115,#17116,#17117,
#17118,#17119,#17120,#17121,#17122,#17123),.UNSPECIFIED.,.F.,.F.,(4,2,2,
2,2,2,2,2,2,2,4),(0.0591825211272536,0.157966726598481,0.236950089897721,
0.315933453196962,0.391576304923761,0.46721915665056,0.542862008377359,
0.618504860104159,0.697488223403399,0.776471586702639,0.875255792173867),
 .UNSPECIFIED.);
#679=B_SPLINE_CURVE_WITH_KNOTS('',3,(#17131,#17132,#17133,#17134,#17135,
#17136,#17137,#17138,#17139,#17140,#17141,#17142,#17143,#17144,#17145,#17146,
#17147,#17148,#17149,#17150,#17151,#17152),.UNSPECIFIED.,.F.,.F.,(4,2,2,
2,2,2,2,2,2,2,4),(0.0591825211272536,0.157966726598481,0.236950089897721,
0.315933453196962,0.391576304923761,0.46721915665056,0.54286200837736,0.618504860104159,
0.697488223403399,0.77647158670264,0.875255792173867),.UNSPECIFIED.);
#680=B_SPLINE_CURVE_WITH_KNOTS('',3,(#17161,#17162,#17163,#17164,#17165,
#17166,#17167,#17168,#17169,#17170,#17171,#17172,#17173,#17174,#17175,#17176,
#17177,#17178,#17179,#17180,#17181,#17182),.UNSPECIFIED.,.F.,.F.,(4,2,2,
2,2,2,2,2,2,2,4),(0.0591825211272536,0.157966726598481,0.236950089897721,
0.315933453196962,0.391576304923761,0.46721915665056,0.542862008377359,
0.618504860104159,0.697488223403399,0.776471586702639,0.875255792173867),
 .UNSPECIFIED.);
#681=B_SPLINE_CURVE_WITH_KNOTS('',3,(#17332,#17333,#17334,#17335,#17336,
#17337,#17338,#17339,#17340,#17341,#17342,#17343,#17344,#17345,#17346,#17347,
#17348,#17349,#17350,#17351,#17352,#17353),.UNSPECIFIED.,.F.,.F.,(4,2,2,
2,2,2,2,2,2,2,4),(0.0789094028588958,0.210573405340968,0.315860108011452,
0.421146810681936,0.522142632548711,0.623138454415485,0.72413427628226,
0.825130098149035,0.930416800819519,1.03570350349,1.16736750597208),
 .UNSPECIFIED.);
#682=B_SPLINE_CURVE_WITH_KNOTS('',3,(#17357,#17358,#17359,#17360,#17361,
#17362,#17363,#17364,#17365,#17366,#17367,#17368,#17369,#17370,#17371,#17372,
#17373,#17374,#17375,#17376,#17377,#17378),.UNSPECIFIED.,.F.,.F.,(4,2,2,
2,2,2,2,2,2,2,4),(0.0774793363974613,0.142088896491891,0.284177792983782,
0.411119756996526,0.514392970548519,0.617666184100513,0.720939397652506,
0.8242126112045,0.951154575217244,1.09324347170913,1.15785303180356),
 .UNSPECIFIED.);
#683=B_SPLINE_CURVE_WITH_KNOTS('',3,(#17384,#17385,#17386,#17387,#17388,
#17389,#17390,#17391,#17392,#17393,#17394,#17395,#17396,#17397,#17398,#17399,
#17400,#17401,#17402,#17403,#17404,#17405),.UNSPECIFIED.,.F.,.F.,(4,2,2,
2,2,2,2,2,2,2,4),(0.0774793363974613,0.142088896491891,0.284177792983782,
0.411119756996525,0.514392970548519,0.617666184100513,0.720939397652506,
0.8242126112045,0.951154575217243,1.09324347170913,1.15785303180356),
 .UNSPECIFIED.);
#684=B_SPLINE_CURVE_WITH_KNOTS('',3,(#17409,#17410,#17411,#17412,#17413,
#17414,#17415,#17416,#17417,#17418,#17419,#17420,#17421,#17422,#17423,#17424,
#17425,#17426,#17427,#17428,#17429,#17430),.UNSPECIFIED.,.F.,.F.,(4,2,2,
2,2,2,2,2,2,2,4),(0.0774793363974614,0.142088896491891,0.284177792983781,
0.411119756996525,0.514392970548519,0.617666184100512,0.720939397652506,
0.824212611204499,0.951154575217243,1.09324347170913,1.15785303180356),
 .UNSPECIFIED.);
#685=B_SPLINE_CURVE_WITH_KNOTS('',3,(#17434,#17435,#17436,#17437,#17438,
#17439,#17440,#17441,#17442,#17443,#17444,#17445),.UNSPECIFIED.,.F.,.F.,
(4,2,2,2,2,4),(0.0774793363974613,0.142088896491891,0.284177792983781,0.411119756996525,
0.514392970548519,0.617666184100512),.UNSPECIFIED.);
#686=B_SPLINE_CURVE_WITH_KNOTS('',3,(#17450,#17451,#17452,#17453,#17454,
#17455,#17456,#17457,#17458,#17459,#17460,#17461),.UNSPECIFIED.,.F.,.F.,
(4,2,2,2,2,4),(0.617666184100512,0.720939397652506,0.824212611204499,0.951154575217243,
1.09324347170913,1.15785303180356),.UNSPECIFIED.);
#687=B_SPLINE_CURVE_WITH_KNOTS('',3,(#17465,#17466,#17467,#17468,#17469,
#17470,#17471,#17472,#17473,#17474,#17475,#17476,#17477,#17478,#17479,#17480,
#17481,#17482,#17483,#17484,#17485,#17486),.UNSPECIFIED.,.F.,.F.,(4,2,2,
2,2,2,2,2,2,2,4),(0.0774793363974613,0.142088896491891,0.284177792983782,
0.411119756996526,0.514392970548519,0.617666184100513,0.720939397652507,
0.8242126112045,0.951154575217245,1.09324347170914,1.15785303180356),
 .UNSPECIFIED.);
#688=B_SPLINE_CURVE_WITH_KNOTS('',3,(#17490,#17491,#17492,#17493,#17494,
#17495,#17496,#17497,#17498,#17499,#17500,#17501,#17502,#17503,#17504,#17505,
#17506,#17507,#17508,#17509,#17510,#17511),.UNSPECIFIED.,.F.,.F.,(4,2,2,
2,2,2,2,2,2,2,4),(0.0774793363974613,0.142088896491891,0.284177792983782,
0.411119756996526,0.514392970548519,0.617666184100513,0.720939397652506,
0.824212611204499,0.951154575217243,1.09324347170913,1.15785303180356),
 .UNSPECIFIED.);
#689=B_SPLINE_CURVE_WITH_KNOTS('',3,(#17515,#17516,#17517,#17518,#17519,
#17520,#17521,#17522,#17523,#17524,#17525,#17526,#17527,#17528,#17529,#17530,
#17531,#17532,#17533,#17534,#17535,#17536),.UNSPECIFIED.,.F.,.F.,(4,2,2,
2,2,2,2,2,2,2,4),(0.0774793363974613,0.142088896491891,0.284177792983782,
0.411119756996526,0.514392970548519,0.617666184100513,0.720939397652506,
0.8242126112045,0.951154575217244,1.09324347170913,1.15785303180356),
 .UNSPECIFIED.);
#690=B_SPLINE_CURVE_WITH_KNOTS('',3,(#17540,#17541,#17542,#17543,#17544,
#17545,#17546,#17547,#17548,#17549,#17550,#17551,#17552,#17553,#17554,#17555,
#17556,#17557,#17558,#17559,#17560,#17561),.UNSPECIFIED.,.F.,.F.,(4,2,2,
2,2,2,2,2,2,2,4),(0.0774793363974613,0.142088896491891,0.284177792983782,
0.411119756996526,0.514392970548519,0.617666184100513,0.720939397652506,
0.8242126112045,0.951154575217243,1.09324347170913,1.15785303180356),
 .UNSPECIFIED.);
#691=B_SPLINE_CURVE_WITH_KNOTS('',3,(#17569,#17570,#17571,#17572,#17573,
#17574,#17575,#17576,#17577,#17578,#17579,#17580,#17581,#17582,#17583,#17584,
#17585,#17586,#17587,#17588,#17589,#17590),.UNSPECIFIED.,.F.,.F.,(4,2,2,
2,2,2,2,2,2,2,4),(0.0789094028588958,0.210573405340968,0.315860108011452,
0.421146810681936,0.522142632548711,0.623138454415485,0.72413427628226,
0.825130098149035,0.930416800819519,1.03570350349,1.16736750597208),
 .UNSPECIFIED.);
#692=B_SPLINE_CURVE_WITH_KNOTS('',3,(#17598,#17599,#17600,#17601,#17602,
#17603,#17604,#17605,#17606,#17607,#17608,#17609,#17610,#17611,#17612,#17613,
#17614,#17615,#17616,#17617,#17618,#17619),.UNSPECIFIED.,.F.,.F.,(4,2,2,
2,2,2,2,2,2,2,4),(0.0789094028588958,0.210573405340969,0.315860108011453,
0.421146810681937,0.522142632548712,0.623138454415486,0.724134276282261,
0.825130098149035,0.930416800819519,1.03570350349,1.16736750597208),
 .UNSPECIFIED.);
#693=B_SPLINE_CURVE_WITH_KNOTS('',3,(#17628,#17629,#17630,#17631,#17632,
#17633,#17634,#17635,#17636,#17637,#17638,#17639),.UNSPECIFIED.,.F.,.F.,
(4,2,2,2,2,4),(0.0789094028588958,0.210573405340968,0.315860108011452,0.421146810681937,
0.522142632548711,0.623138454415486),.UNSPECIFIED.);
#694=B_SPLINE_CURVE_WITH_KNOTS('',3,(#17641,#17642,#17643,#17644,#17645,
#17646,#17647,#17648,#17649,#17650,#17651,#17652),.UNSPECIFIED.,.F.,.F.,
(4,2,2,2,2,4),(0.623138454415486,0.72413427628226,0.825130098149035,0.930416800819519,
1.03570350349,1.16736750597208),.UNSPECIFIED.);
#695=B_SPLINE_CURVE_WITH_KNOTS('',3,(#17659,#17660,#17661,#17662,#17663,
#17664,#17665,#17666,#17667,#17668,#17669,#17670,#17671,#17672,#17673,#17674,
#17675,#17676,#17677,#17678,#17679,#17680),.UNSPECIFIED.,.F.,.F.,(4,2,2,
2,2,2,2,2,2,2,4),(0.0789094028588958,0.210573405340968,0.315860108011452,
0.421146810681936,0.522142632548711,0.623138454415486,0.72413427628226,
0.825130098149035,0.930416800819519,1.03570350349,1.16736750597208),
 .UNSPECIFIED.);
#696=B_SPLINE_CURVE_WITH_KNOTS('',3,(#17688,#17689,#17690,#17691,#17692,
#17693,#17694,#17695,#17696,#17697,#17698,#17699,#17700,#17701,#17702,#17703,
#17704,#17705,#17706,#17707,#17708,#17709),.UNSPECIFIED.,.F.,.F.,(4,2,2,
2,2,2,2,2,2,2,4),(0.0789094028588957,0.210573405340968,0.315860108011452,
0.421146810681936,0.522142632548711,0.623138454415485,0.72413427628226,
0.825130098149035,0.930416800819519,1.03570350349,1.16736750597207),
 .UNSPECIFIED.);
#697=B_SPLINE_CURVE_WITH_KNOTS('',3,(#17717,#17718,#17719,#17720,#17721,
#17722,#17723,#17724,#17725,#17726,#17727,#17728,#17729,#17730,#17731,#17732,
#17733,#17734,#17735,#17736,#17737,#17738),.UNSPECIFIED.,.F.,.F.,(4,2,2,
2,2,2,2,2,2,2,4),(0.0789094028588958,0.210573405340968,0.315860108011452,
0.421146810681936,0.522142632548711,0.623138454415486,0.72413427628226,
0.825130098149035,0.930416800819519,1.03570350349,1.16736750597208),
 .UNSPECIFIED.);
#698=B_SPLINE_CURVE_WITH_KNOTS('',3,(#17747,#17748,#17749,#17750,#17751,
#17752,#17753,#17754,#17755,#17756,#17757,#17758,#17759,#17760,#17761,#17762,
#17763,#17764,#17765,#17766,#17767,#17768),.UNSPECIFIED.,.F.,.F.,(4,2,2,
2,2,2,2,2,2,2,4),(0.0789094028588958,0.210573405340968,0.315860108011452,
0.421146810681936,0.522142632548711,0.623138454415485,0.72413427628226,
0.825130098149035,0.930416800819519,1.03570350349,1.16736750597208),
 .UNSPECIFIED.);
#699=B_SPLINE_CURVE_WITH_KNOTS('',3,(#17992,#17993,#17994,#17995,#17996,
#17997,#17998,#17999,#18000,#18001),.UNSPECIFIED.,.F.,.F.,(4,2,2,2,4),(0.818088904349169,
0.878131747417165,0.957937926194036,1.03774410497091,1.0977869480389),
 .UNSPECIFIED.);
#700=B_SPLINE_CURVE_WITH_KNOTS('',3,(#18007,#18008,#18009,#18010,#18011,
#18012,#18013,#18014,#18015,#18016,#18017,#18018,#18019,#18020,#18021,#18022,
#18023,#18024),.UNSPECIFIED.,.F.,.F.,(4,2,2,2,2,2,2,2,4),(0.,0.0793157643915219,
0.158631528783044,0.23794361593365,0.317255703084255,0.396567790234861,
0.475879877385467,0.555195641776989,0.634511406168511),.UNSPECIFIED.);
#701=B_SPLINE_CURVE_WITH_KNOTS('',3,(#18025,#18026,#18027,#18028,#18029,
#18030,#18031,#18032,#18033,#18034,#18035,#18036,#18037,#18038,#18039,#18040,
#18041,#18042),.UNSPECIFIED.,.F.,.F.,(4,2,2,2,2,2,2,2,4),(0.634511406168511,
0.713827170560033,0.793142934951554,0.87245502210216,0.951767109252766,
1.03107919640337,1.11039128355398,1.1897070479455,1.26902281233702),
 .UNSPECIFIED.);
#702=B_SPLINE_CURVE_WITH_KNOTS('',3,(#18045,#18046,#18047,#18048,#18049,
#18050,#18051,#18052,#18053,#18054),.UNSPECIFIED.,.F.,.F.,(4,2,2,2,4),(0.179463620219812,
0.239506463287808,0.319312642064679,0.399118820841549,0.459161663909545),
 .UNSPECIFIED.);
#703=B_SPLINE_CURVE_WITH_KNOTS('',3,(#18094,#18095,#18096,#18097,#18098,
#18099,#18100,#18101,#18102,#18103),.UNSPECIFIED.,.F.,.F.,(4,2,2,2,4),(0.818088904349169,
0.878131747417165,0.957937926194036,1.03774410497091,1.0977869480389),
 .UNSPECIFIED.);
#704=B_SPLINE_CURVE_WITH_KNOTS('',3,(#18109,#18110,#18111,#18112,#18113,
#18114,#18115,#18116,#18117,#18118,#18119,#18120,#18121,#18122,#18123,#18124,
#18125,#18126),.UNSPECIFIED.,.F.,.F.,(4,2,2,2,2,2,2,2,4),(0.,0.0793157643915219,
0.158631528783044,0.23794361593365,0.317255703084255,0.396567790234861,
0.475879877385467,0.555195641776989,0.634511406168511),.UNSPECIFIED.);
#705=B_SPLINE_CURVE_WITH_KNOTS('',3,(#18127,#18128,#18129,#18130,#18131,
#18132,#18133,#18134,#18135,#18136,#18137,#18138,#18139,#18140,#18141,#18142,
#18143,#18144),.UNSPECIFIED.,.F.,.F.,(4,2,2,2,2,2,2,2,4),(0.634511406168511,
0.713827170560033,0.793142934951554,0.87245502210216,0.951767109252766,
1.03107919640337,1.11039128355398,1.1897070479455,1.26902281233702),
 .UNSPECIFIED.);
#706=B_SPLINE_CURVE_WITH_KNOTS('',3,(#18147,#18148,#18149,#18150,#18151,
#18152,#18153,#18154,#18155,#18156),.UNSPECIFIED.,.F.,.F.,(4,2,2,2,4),(0.179463620219812,
0.239506463287808,0.319312642064679,0.399118820841549,0.459161663909545),
 .UNSPECIFIED.);
#707=B_SPLINE_CURVE_WITH_KNOTS('',3,(#29914,#29915,#29916,#29917,#29918,
#29919,#29920,#29921,#29922,#29923,#29924,#29925,#29926,#29927),
 .UNSPECIFIED.,.F.,.F.,(4,2,2,2,2,2,4),(0.75600573798701,0.793568827564648,
0.872922520054202,0.952276212543757,1.03162990503331,1.11098359752287,1.1485466871005),
 .UNSPECIFIED.);
#708=B_SPLINE_CURVE_WITH_KNOTS('',3,(#29933,#29934,#29935,#29936,#29937,
#29938,#29939,#29940,#29941,#29942,#29943,#29944,#29945,#29946,#29947,#29948,
#29949,#29950),.UNSPECIFIED.,.F.,.F.,(4,2,2,2,2,2,2,2,4),(0.,0.0792028026112442,
0.158405605222488,0.237607602356378,0.316809599490267,0.396011596624156,
0.475213593758045,0.554416396369289,0.633619198980534),.UNSPECIFIED.);
#709=B_SPLINE_CURVE_WITH_KNOTS('',3,(#29951,#29952,#29953,#29954,#29955,
#29956,#29957,#29958,#29959,#29960,#29961,#29962,#29963,#29964,#29965,#29966,
#29967,#29968),.UNSPECIFIED.,.F.,.F.,(4,2,2,2,2,2,2,2,4),(0.633619198980534,
0.712822001591778,0.792024804203022,0.871226801336911,0.9504287984708,1.02963079560469,
1.10883279273858,1.18803559534982,1.26723839796107),.UNSPECIFIED.);
#710=B_SPLINE_CURVE_WITH_KNOTS('',3,(#29971,#29972,#29973,#29974,#29975,
#29976,#29977,#29978,#29979,#29980,#29981,#29982,#29983,#29984),
 .UNSPECIFIED.,.F.,.F.,(4,2,2,2,2,2,4),(0.121154929624505,0.158718019202143,
0.238071711691698,0.317425404181252,0.396779096670807,0.476132789160362,
0.513695878738),.UNSPECIFIED.);
#711=B_SPLINE_CURVE_WITH_KNOTS('',3,(#30024,#30025,#30026,#30027,#30028,
#30029,#30030,#30031,#30032,#30033,#30034,#30035,#30036,#30037),
 .UNSPECIFIED.,.F.,.F.,(4,2,2,2,2,2,4),(0.75600573798701,0.793568827564648,
0.872922520054202,0.952276212543757,1.03162990503331,1.11098359752287,1.14854668710051),
 .UNSPECIFIED.);
#712=B_SPLINE_CURVE_WITH_KNOTS('',3,(#30043,#30044,#30045,#30046,#30047,
#30048,#30049,#30050,#30051,#30052,#30053,#30054,#30055,#30056,#30057,#30058,
#30059,#30060),.UNSPECIFIED.,.F.,.F.,(4,2,2,2,2,2,2,2,4),(0.,0.0792028026112442,
0.158405605222488,0.237607602356378,0.316809599490267,0.396011596624156,
0.475213593758045,0.554416396369289,0.633619198980534),.UNSPECIFIED.);
#713=B_SPLINE_CURVE_WITH_KNOTS('',3,(#30061,#30062,#30063,#30064,#30065,
#30066,#30067,#30068,#30069,#30070,#30071,#30072,#30073,#30074,#30075,#30076,
#30077,#30078),.UNSPECIFIED.,.F.,.F.,(4,2,2,2,2,2,2,2,4),(0.633619198980534,
0.712822001591778,0.792024804203022,0.871226801336911,0.9504287984708,1.02963079560469,
1.10883279273858,1.18803559534982,1.26723839796107),.UNSPECIFIED.);
#714=B_SPLINE_CURVE_WITH_KNOTS('',3,(#30081,#30082,#30083,#30084,#30085,
#30086,#30087,#30088,#30089,#30090,#30091,#30092,#30093,#30094),
 .UNSPECIFIED.,.F.,.F.,(4,2,2,2,2,2,4),(0.121154929624506,0.158718019202143,
0.238071711691698,0.317425404181252,0.396779096670807,0.476132789160362,
0.513695878738),.UNSPECIFIED.);
#715=B_SPLINE_CURVE_WITH_KNOTS('',3,(#36140,#36141,#36142,#36143,#36144,
#36145),.UNSPECIFIED.,.F.,.F.,(4,2,4),(0.,1.,2.),.UNSPECIFIED.);
#716=B_SPLINE_CURVE_WITH_KNOTS('',3,(#36359,#36360,#36361,#36362,#36363,
#36364),.UNSPECIFIED.,.F.,.F.,(4,2,4),(0.,1.,2.),.UNSPECIFIED.);
#717=B_SPLINE_CURVE_WITH_KNOTS('',3,(#36442,#36443,#36444,#36445,#36446,
#36447),.UNSPECIFIED.,.F.,.F.,(4,2,4),(0.,1.,2.),.UNSPECIFIED.);
#718=B_SPLINE_CURVE_WITH_KNOTS('',3,(#36801,#36802,#36803,#36804,#36805,
#36806),.UNSPECIFIED.,.F.,.F.,(4,2,4),(0.,1.,2.),.UNSPECIFIED.);
#719=B_SPLINE_CURVE_WITH_KNOTS('',3,(#36884,#36885,#36886,#36887,#36888,
#36889),.UNSPECIFIED.,.F.,.F.,(4,2,4),(0.,1.,2.),.UNSPECIFIED.);
#720=B_SPLINE_CURVE_WITH_KNOTS('',3,(#37243,#37244,#37245,#37246,#37247,
#37248),.UNSPECIFIED.,.F.,.F.,(4,2,4),(0.,1.,2.),.UNSPECIFIED.);
#721=B_SPLINE_CURVE_WITH_KNOTS('',3,(#37326,#37327,#37328,#37329,#37330,
#37331),.UNSPECIFIED.,.F.,.F.,(4,2,4),(0.,1.,2.),.UNSPECIFIED.);
#722=B_SPLINE_CURVE_WITH_KNOTS('',3,(#37685,#37686,#37687,#37688,#37689,
#37690),.UNSPECIFIED.,.F.,.F.,(4,2,4),(0.,1.,2.),.UNSPECIFIED.);
#723=B_SPLINE_CURVE_WITH_KNOTS('',3,(#37768,#37769,#37770,#37771,#37772,
#37773),.UNSPECIFIED.,.F.,.F.,(4,2,4),(0.,1.,2.),.UNSPECIFIED.);
#724=B_SPLINE_CURVE_WITH_KNOTS('',3,(#38127,#38128,#38129,#38130,#38131,
#38132),.UNSPECIFIED.,.F.,.F.,(4,2,4),(0.,1.,2.),.UNSPECIFIED.);
#725=B_SPLINE_CURVE_WITH_KNOTS('',3,(#38210,#38211,#38212,#38213,#38214,
#38215),.UNSPECIFIED.,.F.,.F.,(4,2,4),(0.,1.,2.),.UNSPECIFIED.);
#726=B_SPLINE_CURVE_WITH_KNOTS('',3,(#38569,#38570,#38571,#38572,#38573,
#38574),.UNSPECIFIED.,.F.,.F.,(4,2,4),(0.,1.,2.),.UNSPECIFIED.);
#727=B_SPLINE_CURVE_WITH_KNOTS('',3,(#38652,#38653,#38654,#38655,#38656,
#38657),.UNSPECIFIED.,.F.,.F.,(4,2,4),(0.,1.,2.),.UNSPECIFIED.);
#728=B_SPLINE_CURVE_WITH_KNOTS('',3,(#39011,#39012,#39013,#39014,#39015,
#39016),.UNSPECIFIED.,.F.,.F.,(4,2,4),(0.,1.,2.),.UNSPECIFIED.);
#729=B_SPLINE_CURVE_WITH_KNOTS('',3,(#39094,#39095,#39096,#39097,#39098,
#39099),.UNSPECIFIED.,.F.,.F.,(4,2,4),(0.,1.,2.),.UNSPECIFIED.);
#730=B_SPLINE_CURVE_WITH_KNOTS('',3,(#39453,#39454,#39455,#39456,#39457,
#39458),.UNSPECIFIED.,.F.,.F.,(4,2,4),(0.,1.,2.),.UNSPECIFIED.);
#731=B_SPLINE_CURVE_WITH_KNOTS('',3,(#39536,#39537,#39538,#39539,#39540,
#39541),.UNSPECIFIED.,.F.,.F.,(4,2,4),(0.,1.,2.),.UNSPECIFIED.);
#732=B_SPLINE_CURVE_WITH_KNOTS('',3,(#39895,#39896,#39897,#39898,#39899,
#39900),.UNSPECIFIED.,.F.,.F.,(4,2,4),(0.,1.,2.),.UNSPECIFIED.);
#733=B_SPLINE_CURVE_WITH_KNOTS('',3,(#39978,#39979,#39980,#39981,#39982,
#39983),.UNSPECIFIED.,.F.,.F.,(4,2,4),(0.,1.,2.),.UNSPECIFIED.);
#734=B_SPLINE_CURVE_WITH_KNOTS('',3,(#40337,#40338,#40339,#40340,#40341,
#40342),.UNSPECIFIED.,.F.,.F.,(4,2,4),(0.,1.,2.),.UNSPECIFIED.);
#735=B_SPLINE_CURVE_WITH_KNOTS('',3,(#40420,#40421,#40422,#40423,#40424,
#40425),.UNSPECIFIED.,.F.,.F.,(4,2,4),(0.,1.,2.),.UNSPECIFIED.);
#736=B_SPLINE_CURVE_WITH_KNOTS('',3,(#40779,#40780,#40781,#40782,#40783,
#40784),.UNSPECIFIED.,.F.,.F.,(4,2,4),(0.,1.,2.),.UNSPECIFIED.);
#737=B_SPLINE_CURVE_WITH_KNOTS('',3,(#40862,#40863,#40864,#40865,#40866,
#40867),.UNSPECIFIED.,.F.,.F.,(4,2,4),(0.,1.,2.),.UNSPECIFIED.);
#738=B_SPLINE_CURVE_WITH_KNOTS('',3,(#41221,#41222,#41223,#41224,#41225,
#41226),.UNSPECIFIED.,.F.,.F.,(4,2,4),(0.,1.,2.),.UNSPECIFIED.);
#739=B_SPLINE_CURVE_WITH_KNOTS('',3,(#41304,#41305,#41306,#41307,#41308,
#41309),.UNSPECIFIED.,.F.,.F.,(4,2,4),(0.,1.,2.),.UNSPECIFIED.);
#740=B_SPLINE_CURVE_WITH_KNOTS('',3,(#41663,#41664,#41665,#41666,#41667,
#41668),.UNSPECIFIED.,.F.,.F.,(4,2,4),(0.,1.,2.),.UNSPECIFIED.);
#741=B_SPLINE_CURVE_WITH_KNOTS('',3,(#41746,#41747,#41748,#41749,#41750,
#41751),.UNSPECIFIED.,.F.,.F.,(4,2,4),(0.,1.,2.),.UNSPECIFIED.);
#742=B_SPLINE_CURVE_WITH_KNOTS('',3,(#42105,#42106,#42107,#42108,#42109,
#42110),.UNSPECIFIED.,.F.,.F.,(4,2,4),(0.,1.,2.),.UNSPECIFIED.);
#743=B_SPLINE_CURVE_WITH_KNOTS('',3,(#42188,#42189,#42190,#42191,#42192,
#42193),.UNSPECIFIED.,.F.,.F.,(4,2,4),(0.,1.,2.),.UNSPECIFIED.);
#744=B_SPLINE_CURVE_WITH_KNOTS('',3,(#42547,#42548,#42549,#42550,#42551,
#42552),.UNSPECIFIED.,.F.,.F.,(4,2,4),(0.,1.,2.),.UNSPECIFIED.);
#745=B_SPLINE_CURVE_WITH_KNOTS('',3,(#42630,#42631,#42632,#42633,#42634,
#42635),.UNSPECIFIED.,.F.,.F.,(4,2,4),(0.,1.,2.),.UNSPECIFIED.);
#746=B_SPLINE_CURVE_WITH_KNOTS('',3,(#42989,#42990,#42991,#42992,#42993,
#42994),.UNSPECIFIED.,.F.,.F.,(4,2,4),(0.,1.,2.),.UNSPECIFIED.);
#747=B_SPLINE_CURVE_WITH_KNOTS('',3,(#43072,#43073,#43074,#43075,#43076,
#43077),.UNSPECIFIED.,.F.,.F.,(4,2,4),(0.,1.,2.),.UNSPECIFIED.);
#748=B_SPLINE_CURVE_WITH_KNOTS('',3,(#43431,#43432,#43433,#43434,#43435,
#43436),.UNSPECIFIED.,.F.,.F.,(4,2,4),(0.,1.,2.),.UNSPECIFIED.);
#749=B_SPLINE_CURVE_WITH_KNOTS('',3,(#43514,#43515,#43516,#43517,#43518,
#43519),.UNSPECIFIED.,.F.,.F.,(4,2,4),(0.,1.,2.),.UNSPECIFIED.);
#750=B_SPLINE_CURVE_WITH_KNOTS('',3,(#43873,#43874,#43875,#43876,#43877,
#43878),.UNSPECIFIED.,.F.,.F.,(4,2,4),(0.,1.,2.),.UNSPECIFIED.);
#751=B_SPLINE_CURVE_WITH_KNOTS('',3,(#43956,#43957,#43958,#43959,#43960,
#43961),.UNSPECIFIED.,.F.,.F.,(4,2,4),(0.,1.,2.),.UNSPECIFIED.);
#752=B_SPLINE_CURVE_WITH_KNOTS('',3,(#44315,#44316,#44317,#44318,#44319,
#44320),.UNSPECIFIED.,.F.,.F.,(4,2,4),(0.,1.,2.),.UNSPECIFIED.);
#753=B_SPLINE_CURVE_WITH_KNOTS('',3,(#44398,#44399,#44400,#44401,#44402,
#44403),.UNSPECIFIED.,.F.,.F.,(4,2,4),(0.,1.,2.),.UNSPECIFIED.);
#754=B_SPLINE_CURVE_WITH_KNOTS('',3,(#44757,#44758,#44759,#44760,#44761,
#44762),.UNSPECIFIED.,.F.,.F.,(4,2,4),(0.,1.,2.),.UNSPECIFIED.);
#755=B_SPLINE_CURVE_WITH_KNOTS('',3,(#44840,#44841,#44842,#44843,#44844,
#44845),.UNSPECIFIED.,.F.,.F.,(4,2,4),(0.,1.,2.),.UNSPECIFIED.);
#756=B_SPLINE_CURVE_WITH_KNOTS('',3,(#45199,#45200,#45201,#45202,#45203,
#45204),.UNSPECIFIED.,.F.,.F.,(4,2,4),(0.,1.,2.),.UNSPECIFIED.);
#757=B_SPLINE_CURVE_WITH_KNOTS('',3,(#45282,#45283,#45284,#45285,#45286,
#45287),.UNSPECIFIED.,.F.,.F.,(4,2,4),(0.,1.,2.),.UNSPECIFIED.);
#758=B_SPLINE_CURVE_WITH_KNOTS('',3,(#45641,#45642,#45643,#45644,#45645,
#45646),.UNSPECIFIED.,.F.,.F.,(4,2,4),(0.,1.,2.),.UNSPECIFIED.);
#759=B_SPLINE_CURVE_WITH_KNOTS('',3,(#45724,#45725,#45726,#45727,#45728,
#45729),.UNSPECIFIED.,.F.,.F.,(4,2,4),(0.,1.,2.),.UNSPECIFIED.);
#760=B_SPLINE_CURVE_WITH_KNOTS('',3,(#46083,#46084,#46085,#46086,#46087,
#46088),.UNSPECIFIED.,.F.,.F.,(4,2,4),(0.,1.,2.),.UNSPECIFIED.);
#761=B_SPLINE_CURVE_WITH_KNOTS('',3,(#46166,#46167,#46168,#46169,#46170,
#46171),.UNSPECIFIED.,.F.,.F.,(4,2,4),(0.,1.,2.),.UNSPECIFIED.);
#762=B_SPLINE_CURVE_WITH_KNOTS('',3,(#46525,#46526,#46527,#46528,#46529,
#46530),.UNSPECIFIED.,.F.,.F.,(4,2,4),(0.,1.,2.),.UNSPECIFIED.);
#763=B_SPLINE_CURVE_WITH_KNOTS('',3,(#46608,#46609,#46610,#46611,#46612,
#46613),.UNSPECIFIED.,.F.,.F.,(4,2,4),(0.,1.,2.),.UNSPECIFIED.);
#764=B_SPLINE_CURVE_WITH_KNOTS('',3,(#46967,#46968,#46969,#46970,#46971,
#46972),.UNSPECIFIED.,.F.,.F.,(4,2,4),(0.,1.,2.),.UNSPECIFIED.);
#765=B_SPLINE_CURVE_WITH_KNOTS('',3,(#47050,#47051,#47052,#47053,#47054,
#47055),.UNSPECIFIED.,.F.,.F.,(4,2,4),(0.,1.,2.),.UNSPECIFIED.);
#766=B_SPLINE_CURVE_WITH_KNOTS('',3,(#47409,#47410,#47411,#47412,#47413,
#47414),.UNSPECIFIED.,.F.,.F.,(4,2,4),(0.,1.,2.),.UNSPECIFIED.);
#767=B_SPLINE_CURVE_WITH_KNOTS('',3,(#47492,#47493,#47494,#47495,#47496,
#47497),.UNSPECIFIED.,.F.,.F.,(4,2,4),(0.,1.,2.),.UNSPECIFIED.);
#768=B_SPLINE_CURVE_WITH_KNOTS('',3,(#47851,#47852,#47853,#47854,#47855,
#47856),.UNSPECIFIED.,.F.,.F.,(4,2,4),(0.,1.,2.),.UNSPECIFIED.);
#769=B_SPLINE_CURVE_WITH_KNOTS('',3,(#47934,#47935,#47936,#47937,#47938,
#47939),.UNSPECIFIED.,.F.,.F.,(4,2,4),(0.,1.,2.),.UNSPECIFIED.);
#770=B_SPLINE_CURVE_WITH_KNOTS('',3,(#48293,#48294,#48295,#48296,#48297,
#48298),.UNSPECIFIED.,.F.,.F.,(4,2,4),(0.,1.,2.),.UNSPECIFIED.);
#771=B_SPLINE_CURVE_WITH_KNOTS('',3,(#48376,#48377,#48378,#48379,#48380,
#48381),.UNSPECIFIED.,.F.,.F.,(4,2,4),(0.,1.,2.),.UNSPECIFIED.);
#772=B_SPLINE_CURVE_WITH_KNOTS('',3,(#48735,#48736,#48737,#48738,#48739,
#48740),.UNSPECIFIED.,.F.,.F.,(4,2,4),(0.,1.,2.),.UNSPECIFIED.);
#773=B_SPLINE_CURVE_WITH_KNOTS('',3,(#48818,#48819,#48820,#48821,#48822,
#48823),.UNSPECIFIED.,.F.,.F.,(4,2,4),(0.,1.,2.),.UNSPECIFIED.);
#774=B_SPLINE_CURVE_WITH_KNOTS('',3,(#49177,#49178,#49179,#49180,#49181,
#49182),.UNSPECIFIED.,.F.,.F.,(4,2,4),(0.,1.,2.),.UNSPECIFIED.);
#775=B_SPLINE_CURVE_WITH_KNOTS('',3,(#49260,#49261,#49262,#49263,#49264,
#49265),.UNSPECIFIED.,.F.,.F.,(4,2,4),(0.,1.,2.),.UNSPECIFIED.);
#776=B_SPLINE_CURVE_WITH_KNOTS('',3,(#49619,#49620,#49621,#49622,#49623,
#49624),.UNSPECIFIED.,.F.,.F.,(4,2,4),(0.,1.,2.),.UNSPECIFIED.);
#777=B_SPLINE_CURVE_WITH_KNOTS('',3,(#49702,#49703,#49704,#49705,#49706,
#49707),.UNSPECIFIED.,.F.,.F.,(4,2,4),(0.,1.,2.),.UNSPECIFIED.);
#778=B_SPLINE_CURVE_WITH_KNOTS('',3,(#50061,#50062,#50063,#50064,#50065,
#50066),.UNSPECIFIED.,.F.,.F.,(4,2,4),(0.,1.,2.),.UNSPECIFIED.);
#779=B_SPLINE_CURVE_WITH_KNOTS('',3,(#50144,#50145,#50146,#50147,#50148,
#50149),.UNSPECIFIED.,.F.,.F.,(4,2,4),(0.,1.,2.),.UNSPECIFIED.);
#780=B_SPLINE_CURVE_WITH_KNOTS('',3,(#50503,#50504,#50505,#50506,#50507,
#50508),.UNSPECIFIED.,.F.,.F.,(4,2,4),(0.,1.,2.),.UNSPECIFIED.);
#781=B_SPLINE_CURVE_WITH_KNOTS('',3,(#50586,#50587,#50588,#50589,#50590,
#50591),.UNSPECIFIED.,.F.,.F.,(4,2,4),(0.,1.,2.),.UNSPECIFIED.);
#782=B_SPLINE_CURVE_WITH_KNOTS('',3,(#50945,#50946,#50947,#50948,#50949,
#50950),.UNSPECIFIED.,.F.,.F.,(4,2,4),(0.,1.,2.),.UNSPECIFIED.);
#783=B_SPLINE_CURVE_WITH_KNOTS('',3,(#51028,#51029,#51030,#51031,#51032,
#51033),.UNSPECIFIED.,.F.,.F.,(4,2,4),(0.,1.,2.),.UNSPECIFIED.);
#784=B_SPLINE_CURVE_WITH_KNOTS('',3,(#51387,#51388,#51389,#51390,#51391,
#51392),.UNSPECIFIED.,.F.,.F.,(4,2,4),(0.,1.,2.),.UNSPECIFIED.);
#785=B_SPLINE_CURVE_WITH_KNOTS('',3,(#51470,#51471,#51472,#51473,#51474,
#51475),.UNSPECIFIED.,.F.,.F.,(4,2,4),(0.,1.,2.),.UNSPECIFIED.);
#786=B_SPLINE_CURVE_WITH_KNOTS('',3,(#51829,#51830,#51831,#51832,#51833,
#51834),.UNSPECIFIED.,.F.,.F.,(4,2,4),(0.,1.,2.),.UNSPECIFIED.);
#787=B_SPLINE_CURVE_WITH_KNOTS('',3,(#51912,#51913,#51914,#51915,#51916,
#51917),.UNSPECIFIED.,.F.,.F.,(4,2,4),(0.,1.,2.),.UNSPECIFIED.);
#788=B_SPLINE_CURVE_WITH_KNOTS('',3,(#52271,#52272,#52273,#52274,#52275,
#52276),.UNSPECIFIED.,.F.,.F.,(4,2,4),(0.,1.,2.),.UNSPECIFIED.);
#789=B_SPLINE_CURVE_WITH_KNOTS('',3,(#52354,#52355,#52356,#52357,#52358,
#52359),.UNSPECIFIED.,.F.,.F.,(4,2,4),(0.,1.,2.),.UNSPECIFIED.);
#790=B_SPLINE_CURVE_WITH_KNOTS('',3,(#52713,#52714,#52715,#52716,#52717,
#52718),.UNSPECIFIED.,.F.,.F.,(4,2,4),(0.,1.,2.),.UNSPECIFIED.);
#791=B_SPLINE_CURVE_WITH_KNOTS('',3,(#52796,#52797,#52798,#52799,#52800,
#52801),.UNSPECIFIED.,.F.,.F.,(4,2,4),(0.,1.,2.),.UNSPECIFIED.);
#792=B_SPLINE_CURVE_WITH_KNOTS('',3,(#53159,#53160,#53161,#53162,#53163,
#53164),.UNSPECIFIED.,.F.,.F.,(4,2,4),(0.,1.,2.),.UNSPECIFIED.);
#793=B_SPLINE_CURVE_WITH_KNOTS('',3,(#53238,#53239,#53240,#53241,#53242,
#53243),.UNSPECIFIED.,.F.,.F.,(4,2,4),(0.,1.,2.),.UNSPECIFIED.);
#794=B_SPLINE_CURVE_WITH_KNOTS('',3,(#53385,#53386,#53387,#53388,#53389,
#53390),.UNSPECIFIED.,.F.,.F.,(4,2,4),(0.,1.,2.),.UNSPECIFIED.);
#795=SPHERICAL_SURFACE('',#12195,0.29765);
#796=SPHERICAL_SURFACE('',#12197,0.29765);
#797=SPHERICAL_SURFACE('',#12199,0.29765);
#798=SPHERICAL_SURFACE('',#12201,0.29765);
#799=SPHERICAL_SURFACE('',#12203,0.29765);
#800=SPHERICAL_SURFACE('',#12205,0.29765);
#801=SPHERICAL_SURFACE('',#12207,0.29765);
#802=SPHERICAL_SURFACE('',#12210,0.309556);
#803=SPHERICAL_SURFACE('',#12226,0.309556);
#804=SPHERICAL_SURFACE('',#12231,0.309556);
#805=SPHERICAL_SURFACE('',#12237,0.309556);
#806=SPHERICAL_SURFACE('',#12242,0.309556);
#807=SPHERICAL_SURFACE('',#12247,0.309556);
#808=SPHERICAL_SURFACE('',#12255,0.309556);
#809=SPHERICAL_SURFACE('',#12323,0.3969);
#810=SPHERICAL_SURFACE('',#12325,0.3969);
#811=SPHERICAL_SURFACE('',#12327,0.3969);
#812=SPHERICAL_SURFACE('',#12329,0.3969);
#813=SPHERICAL_SURFACE('',#12331,0.3969);
#814=SPHERICAL_SURFACE('',#12333,0.3969);
#815=SPHERICAL_SURFACE('',#12335,0.3969);
#816=SPHERICAL_SURFACE('',#12337,0.3969);
#817=SPHERICAL_SURFACE('',#12340,0.412776);
#818=SPHERICAL_SURFACE('',#12356,0.412776);
#819=SPHERICAL_SURFACE('',#12361,0.412776);
#820=SPHERICAL_SURFACE('',#12366,0.412776);
#821=SPHERICAL_SURFACE('',#12371,0.412776);
#822=SPHERICAL_SURFACE('',#12376,0.412776);
#823=SPHERICAL_SURFACE('',#12381,0.412776);
#824=SPHERICAL_SURFACE('',#12389,0.412776);
#825=TOROIDAL_SURFACE('',#12155,1.1,0.309556);
#826=TOROIDAL_SURFACE('',#12175,1.1,0.309556);
#827=TOROIDAL_SURFACE('',#12283,1.675,0.412776);
#828=TOROIDAL_SURFACE('',#12303,1.675,0.412776);
#829=ORIENTED_CLOSED_SHELL('',*,#11283,.F.);
#830=ORIENTED_CLOSED_SHELL('',*,#11285,.F.);
#831=ORIENTED_CLOSED_SHELL('',*,#11312,.F.);
#832=CONICAL_SURFACE('',#12104,0.4,0.785398163397448);
#833=CONICAL_SURFACE('',#12108,0.41,0.785398163397448);
#834=CONICAL_SURFACE('',#12112,0.26,0.463647609000806);
#835=CONICAL_SURFACE('',#12116,0.225,0.785398163397448);
#836=CONICAL_SURFACE('',#12130,0.475,0.785398163397449);
#837=CONICAL_SURFACE('',#12134,0.485,0.785398163397448);
#838=CONICAL_SURFACE('',#12138,0.31,0.463647609000806);
#839=CONICAL_SURFACE('',#12142,0.27,0.785398163397448);
#840=CONICAL_SURFACE('',#12166,0.63,0.785398163397448);
#841=CONICAL_SURFACE('',#12173,0.63,0.785398163397448);
#842=CONICAL_SURFACE('',#12186,1.57,0.785398163397449);
#843=CONICAL_SURFACE('',#12190,1.57,0.785398163397449);
#844=CONICAL_SURFACE('',#12294,1.05,0.785398163397449);
#845=CONICAL_SURFACE('',#12301,1.05,0.785398163397449);
#846=CONICAL_SURFACE('',#12314,2.3,0.785398163397449);
#847=CONICAL_SURFACE('',#12318,2.3,0.785398163397449);
#848=CONICAL_SURFACE('',#12418,0.325,0.785398163397448);
#849=CONICAL_SURFACE('',#12422,0.335,0.785398163397448);
#850=CONICAL_SURFACE('',#12426,0.21,0.463647609000806);
#851=CONICAL_SURFACE('',#12430,0.18,0.785398163397448);
#852=CONICAL_SURFACE('',#12655,0.18,0.785398163397448);
#853=CONICAL_SURFACE('',#12659,0.18,0.785398163397448);
#854=CONICAL_SURFACE('',#12667,0.18,0.785398163397449);
#855=CONICAL_SURFACE('',#12670,0.18,0.785398163397449);
#856=CONICAL_SURFACE('',#12950,0.235,0.785398163397448);
#857=CONICAL_SURFACE('',#12954,0.2125,0.785398163397448);
#858=BREP_WITH_VOIDS('Body1',#11282,(#829));
#859=BREP_WITH_VOIDS('Body1',#11284,(#830));
#860=BREP_WITH_VOIDS('Body1',#11311,(#831));
#861=SHAPE_REPRESENTATION_RELATIONSHIP('SRR','None',#54088,#904);
#862=SHAPE_REPRESENTATION_RELATIONSHIP('SRR','None',#54089,#905);
#863=SHAPE_REPRESENTATION_RELATIONSHIP('SRR','None',#54090,#906);
#864=SHAPE_REPRESENTATION_RELATIONSHIP('SRR','None',#54091,#907);
#865=SHAPE_REPRESENTATION_RELATIONSHIP('SRR','None',#54092,#908);
#866=SHAPE_REPRESENTATION_RELATIONSHIP('SRR','None',#54093,#909);
#867=SHAPE_REPRESENTATION_RELATIONSHIP('SRR','None',#54094,#910);
#868=SHAPE_REPRESENTATION_RELATIONSHIP('SRR','None',#54095,#911);
#869=SHAPE_REPRESENTATION_RELATIONSHIP('SRR','None',#54096,#912);
#870=SHAPE_REPRESENTATION_RELATIONSHIP('SRR','None',#54097,#913);
#871=SHAPE_REPRESENTATION_RELATIONSHIP('SRR','None',#54098,#914);
#872=SHAPE_REPRESENTATION_RELATIONSHIP('SRR','None',#54099,#915);
#873=SHAPE_REPRESENTATION_RELATIONSHIP('SRR','None',#54100,#916);
#874=SHAPE_REPRESENTATION_RELATIONSHIP('SRR','None',#54102,#917);
#875=SHAPE_REPRESENTATION_RELATIONSHIP('SRR','None',#54103,#918);
#876=SHAPE_REPRESENTATION_RELATIONSHIP('SRR','None',#54104,#919);
#877=SHAPE_REPRESENTATION_RELATIONSHIP('SRR','None',#54105,#920);
#878=SHAPE_REPRESENTATION_RELATIONSHIP('SRR','None',#54106,#921);
#879=SHAPE_REPRESENTATION_RELATIONSHIP('SRR','None',#54108,#922);
#880=SHAPE_REPRESENTATION_RELATIONSHIP('SRR','None',#54109,#923);
#881=SHAPE_REPRESENTATION_RELATIONSHIP('SRR','None',#54110,#924);
#882=SHAPE_REPRESENTATION_RELATIONSHIP('SRR','None',#54111,#925);
#883=SHAPE_REPRESENTATION_RELATIONSHIP('SRR','None',#54112,#926);
#884=SHAPE_REPRESENTATION_RELATIONSHIP('SRR','None',#54113,#927);
#885=SHAPE_REPRESENTATION_RELATIONSHIP('SRR','None',#54115,#928);
#886=SHAPE_REPRESENTATION_RELATIONSHIP('SRR','None',#54116,#929);
#887=SHAPE_REPRESENTATION_RELATIONSHIP('SRR','None',#54117,#930);
#888=SHAPE_REPRESENTATION_RELATIONSHIP('SRR','None',#54118,#931);
#889=SHAPE_REPRESENTATION_RELATIONSHIP('SRR','None',#54119,#932);
#890=SHAPE_REPRESENTATION_RELATIONSHIP('SRR','None',#54120,#933);
#891=SHAPE_REPRESENTATION_RELATIONSHIP('SRR','None',#54121,#934);
#892=SHAPE_REPRESENTATION_RELATIONSHIP('SRR','None',#54122,#935);
#893=SHAPE_REPRESENTATION_RELATIONSHIP('SRR','None',#54123,#936);
#894=SHAPE_REPRESENTATION_RELATIONSHIP('SRR','None',#54125,#937);
#895=SHAPE_REPRESENTATION_RELATIONSHIP('SRR','None',#54126,#938);
#896=SHAPE_REPRESENTATION_RELATIONSHIP('SRR','None',#54127,#939);
#897=SHAPE_REPRESENTATION_RELATIONSHIP('SRR','None',#54128,#940);
#898=SHAPE_REPRESENTATION_RELATIONSHIP('SRR','None',#54129,#941);
#899=SHAPE_REPRESENTATION_RELATIONSHIP('SRR','None',#54130,#942);
#900=SHAPE_REPRESENTATION_RELATIONSHIP('SRR','None',#54131,#943);
#901=SHAPE_REPRESENTATION_RELATIONSHIP('SRR','None',#54132,#944);
#902=SHAPE_REPRESENTATION_RELATIONSHIP('SRR','None',#54133,#945);
#903=SHAPE_REPRESENTATION_RELATIONSHIP('SRR','None',#54134,#946);
#904=ADVANCED_BREP_SHAPE_REPRESENTATION('',(#1005),#53862);
#905=ADVANCED_BREP_SHAPE_REPRESENTATION('',(#1006),#53863);
#906=ADVANCED_BREP_SHAPE_REPRESENTATION('',(#1007),#53864);
#907=ADVANCED_BREP_SHAPE_REPRESENTATION('',(#1008),#53865);
#908=ADVANCED_BREP_SHAPE_REPRESENTATION('',(#1009),#53866);
#909=ADVANCED_BREP_SHAPE_REPRESENTATION('',(#1010),#53867);
#910=ADVANCED_BREP_SHAPE_REPRESENTATION('',(#1011),#53868);
#911=ADVANCED_BREP_SHAPE_REPRESENTATION('',(#1012),#53869);
#912=ADVANCED_BREP_SHAPE_REPRESENTATION('',(#1013),#53870);
#913=ADVANCED_BREP_SHAPE_REPRESENTATION('',(#1014),#53871);
#914=ADVANCED_BREP_SHAPE_REPRESENTATION('',(#1015),#53872);
#915=ADVANCED_BREP_SHAPE_REPRESENTATION('',(#858),#53873);
#916=ADVANCED_BREP_SHAPE_REPRESENTATION('',(#859),#53874);
#917=ADVANCED_BREP_SHAPE_REPRESENTATION('',(#1016),#53876);
#918=ADVANCED_BREP_SHAPE_REPRESENTATION('',(#1017),#53877);
#919=ADVANCED_BREP_SHAPE_REPRESENTATION('',(#1018,#1019,#1020,#1021,#1022,
#1023,#1024),#53878);
#920=ADVANCED_BREP_SHAPE_REPRESENTATION('',(#1025),#53879);
#921=ADVANCED_BREP_SHAPE_REPRESENTATION('',(#1026,#1027),#53880);
#922=ADVANCED_BREP_SHAPE_REPRESENTATION('',(#1028),#53882);
#923=ADVANCED_BREP_SHAPE_REPRESENTATION('',(#1029),#53883);
#924=ADVANCED_BREP_SHAPE_REPRESENTATION('',(#1030,#1031,#1032,#1033,#1034,
#1035,#1036,#1037),#53884);
#925=ADVANCED_BREP_SHAPE_REPRESENTATION('',(#1038),#53885);
#926=ADVANCED_BREP_SHAPE_REPRESENTATION('',(#1039,#1040),#53886);
#927=ADVANCED_BREP_SHAPE_REPRESENTATION('',(#860),#53887);
#928=ADVANCED_BREP_SHAPE_REPRESENTATION('',(#1041),#53889);
#929=ADVANCED_BREP_SHAPE_REPRESENTATION('',(#1042),#53890);
#930=ADVANCED_BREP_SHAPE_REPRESENTATION('',(#1043),#53891);
#931=ADVANCED_BREP_SHAPE_REPRESENTATION('',(#1044),#53892);
#932=ADVANCED_BREP_SHAPE_REPRESENTATION('',(#1045),#53893);
#933=ADVANCED_BREP_SHAPE_REPRESENTATION('',(#1046),#53894);
#934=ADVANCED_BREP_SHAPE_REPRESENTATION('',(#1047),#53895);
#935=ADVANCED_BREP_SHAPE_REPRESENTATION('',(#1048),#53896);
#936=ADVANCED_BREP_SHAPE_REPRESENTATION('',(#1049),#53897);
#937=ADVANCED_BREP_SHAPE_REPRESENTATION('',(#1050),#53899);
#938=ADVANCED_BREP_SHAPE_REPRESENTATION('',(#1051),#53900);
#939=ADVANCED_BREP_SHAPE_REPRESENTATION('',(#1052),#53901);
#940=ADVANCED_BREP_SHAPE_REPRESENTATION('',(#1053),#53902);
#941=ADVANCED_BREP_SHAPE_REPRESENTATION('',(#1054),#53903);
#942=ADVANCED_BREP_SHAPE_REPRESENTATION('',(#1055),#53904);
#943=ADVANCED_BREP_SHAPE_REPRESENTATION('',(#1056),#53905);
#944=ADVANCED_BREP_SHAPE_REPRESENTATION('',(#1057),#53906);
#945=ADVANCED_BREP_SHAPE_REPRESENTATION('',(#1058),#53907);
#946=ADVANCED_BREP_SHAPE_REPRESENTATION('',(#1059),#53908);
#947=STYLED_ITEM('',(#54376),#1005);
#948=STYLED_ITEM('',(#54411),#1006);
#949=STYLED_ITEM('',(#54411),#1007);
#950=STYLED_ITEM('',(#54376),#1008);
#951=STYLED_ITEM('',(#54376),#1009);
#952=STYLED_ITEM('',(#54376),#1010);
#953=STYLED_ITEM('',(#54376),#1011);
#954=STYLED_ITEM('',(#54397),#1012);
#955=STYLED_ITEM('',(#54397),#1013);
#956=STYLED_ITEM('',(#54397),#1014);
#957=STYLED_ITEM('',(#54397),#1015);
#958=STYLED_ITEM('',(#54404),#858);
#959=STYLED_ITEM('',(#54404),#859);
#960=STYLED_ITEM('',(#54397),#1016);
#961=STYLED_ITEM('',(#54397),#1017);
#962=STYLED_ITEM('',(#54397),#1018);
#963=STYLED_ITEM('',(#54397),#1019);
#964=STYLED_ITEM('',(#54397),#1020);
#965=STYLED_ITEM('',(#54397),#1021);
#966=STYLED_ITEM('',(#54397),#1022);
#967=STYLED_ITEM('',(#54397),#1023);
#968=STYLED_ITEM('',(#54397),#1024);
#969=STYLED_ITEM('',(#54397),#1025);
#970=STYLED_ITEM('',(#54397),#1026);
#971=STYLED_ITEM('',(#54397),#1027);
#972=STYLED_ITEM('',(#54397),#1028);
#973=STYLED_ITEM('',(#54397),#1029);
#974=STYLED_ITEM('',(#54397),#1030);
#975=STYLED_ITEM('',(#54397),#1031);
#976=STYLED_ITEM('',(#54397),#1032);
#977=STYLED_ITEM('',(#54397),#1033);
#978=STYLED_ITEM('',(#54397),#1034);
#979=STYLED_ITEM('',(#54397),#1035);
#980=STYLED_ITEM('',(#54397),#1036);
#981=STYLED_ITEM('',(#54397),#1037);
#982=STYLED_ITEM('',(#54397),#1038);
#983=STYLED_ITEM('',(#54397),#1039);
#984=STYLED_ITEM('',(#54397),#1040);
#985=STYLED_ITEM('',(#54404),#860);
#986=STYLED_ITEM('',(#54397),#1041);
#987=STYLED_ITEM('',(#54383),#1042);
#988=STYLED_ITEM('',(#54390),#1043);
#989=STYLED_ITEM('',(#54383),#1044);
#990=STYLED_ITEM('',(#54397),#1045);
#991=STYLED_ITEM('',(#54383),#1046);
#992=STYLED_ITEM('',(#54397),#1047);
#993=STYLED_ITEM('',(#54411),#1048);
#994=STYLED_ITEM('',(#54397),#1049);
#995=STYLED_ITEM('',(#54397),#1050);
#996=STYLED_ITEM('',(#54411),#1051);
#997=STYLED_ITEM('',(#54383),#1052);
#998=STYLED_ITEM('',(#54411),#1053);
#999=STYLED_ITEM('',(#54397),#1054);
#1000=STYLED_ITEM('',(#54411),#1055);
#1001=STYLED_ITEM('',(#54397),#1056);
#1002=STYLED_ITEM('',(#54390),#1057);
#1003=STYLED_ITEM('',(#54397),#1058);
#1004=STYLED_ITEM('',(#54404),#1059);
#1005=MANIFOLD_SOLID_BREP('Body1',#11271);
#1006=MANIFOLD_SOLID_BREP('Body1',#11272);
#1007=MANIFOLD_SOLID_BREP('Body1',#11273);
#1008=MANIFOLD_SOLID_BREP('Body1',#11274);
#1009=MANIFOLD_SOLID_BREP('Body1',#11275);
#1010=MANIFOLD_SOLID_BREP('Body1',#11276);
#1011=MANIFOLD_SOLID_BREP('Body1',#11277);
#1012=MANIFOLD_SOLID_BREP('Body1',#11278);
#1013=MANIFOLD_SOLID_BREP('Body1',#11279);
#1014=MANIFOLD_SOLID_BREP('Body1',#11280);
#1015=MANIFOLD_SOLID_BREP('Body1',#11281);
#1016=MANIFOLD_SOLID_BREP('Body1',#11286);
#1017=MANIFOLD_SOLID_BREP('Body1',#11287);
#1018=MANIFOLD_SOLID_BREP('Body1',#11288);
#1019=MANIFOLD_SOLID_BREP('Body2',#11289);
#1020=MANIFOLD_SOLID_BREP('Body3',#11290);
#1021=MANIFOLD_SOLID_BREP('Body4',#11291);
#1022=MANIFOLD_SOLID_BREP('Body5',#11292);
#1023=MANIFOLD_SOLID_BREP('Body6',#11293);
#1024=MANIFOLD_SOLID_BREP('Body7',#11294);
#1025=MANIFOLD_SOLID_BREP('Continuous crown cage',#11295);
#1026=MANIFOLD_SOLID_BREP('Body1',#11296);
#1027=MANIFOLD_SOLID_BREP('Body2',#11297);
#1028=MANIFOLD_SOLID_BREP('Body1',#11298);
#1029=MANIFOLD_SOLID_BREP('Body1',#11299);
#1030=MANIFOLD_SOLID_BREP('Body1',#11300);
#1031=MANIFOLD_SOLID_BREP('Body2',#11301);
#1032=MANIFOLD_SOLID_BREP('Body3',#11302);
#1033=MANIFOLD_SOLID_BREP('Body4',#11303);
#1034=MANIFOLD_SOLID_BREP('Body5',#11304);
#1035=MANIFOLD_SOLID_BREP('Body6',#11305);
#1036=MANIFOLD_SOLID_BREP('Body7',#11306);
#1037=MANIFOLD_SOLID_BREP('Body8',#11307);
#1038=MANIFOLD_SOLID_BREP('Continuous crown cage',#11308);
#1039=MANIFOLD_SOLID_BREP('Body1',#11309);
#1040=MANIFOLD_SOLID_BREP('Body2',#11310);
#1041=MANIFOLD_SOLID_BREP('Body1',#11313);
#1042=MANIFOLD_SOLID_BREP('Body1',#11314);
#1043=MANIFOLD_SOLID_BREP('Body1',#11315);
#1044=MANIFOLD_SOLID_BREP('Body1',#11316);
#1045=MANIFOLD_SOLID_BREP('Body1',#11317);
#1046=MANIFOLD_SOLID_BREP('Body1',#11318);
#1047=MANIFOLD_SOLID_BREP('Body1',#11319);
#1048=MANIFOLD_SOLID_BREP('Body1',#11320);
#1049=MANIFOLD_SOLID_BREP('Body1',#11321);
#1050=MANIFOLD_SOLID_BREP('Body1',#11322);
#1051=MANIFOLD_SOLID_BREP('Body1',#11323);
#1052=MANIFOLD_SOLID_BREP('Body1',#11324);
#1053=MANIFOLD_SOLID_BREP('Body1',#11325);
#1054=MANIFOLD_SOLID_BREP('Body1',#11326);
#1055=MANIFOLD_SOLID_BREP('Body1',#11327);
#1056=MANIFOLD_SOLID_BREP('Body1',#11328);
#1057=MANIFOLD_SOLID_BREP('Body1',#11329);
#1058=MANIFOLD_SOLID_BREP('Body1',#11330);
#1059=MANIFOLD_SOLID_BREP('Body1',#11331);
#1060=FACE_BOUND('',#2160,.T.);
#1061=FACE_BOUND('',#2161,.T.);
#1062=FACE_BOUND('',#2162,.T.);
#1063=FACE_BOUND('',#2163,.T.);
#1064=FACE_BOUND('',#2165,.T.);
#1065=FACE_BOUND('',#2166,.T.);
#1066=FACE_BOUND('',#2167,.T.);
#1067=FACE_BOUND('',#2168,.T.);
#1068=FACE_BOUND('',#2177,.T.);
#1069=FACE_BOUND('',#2180,.T.);
#1070=FACE_BOUND('',#2183,.T.);
#1071=FACE_BOUND('',#2186,.T.);
#1072=FACE_BOUND('',#2197,.T.);
#1073=FACE_BOUND('',#2201,.T.);
#1074=FACE_BOUND('',#2204,.T.);
#1075=FACE_BOUND('',#2205,.T.);
#1076=FACE_BOUND('',#2206,.T.);
#1077=FACE_BOUND('',#2207,.T.);
#1078=FACE_BOUND('',#2208,.T.);
#1079=FACE_BOUND('',#2209,.T.);
#1080=FACE_BOUND('',#2210,.T.);
#1081=FACE_BOUND('',#2211,.T.);
#1082=FACE_BOUND('',#2212,.T.);
#1083=FACE_BOUND('',#2213,.T.);
#1084=FACE_BOUND('',#2214,.T.);
#1085=FACE_BOUND('',#2215,.T.);
#1086=FACE_BOUND('',#2218,.T.);
#1087=FACE_BOUND('',#2219,.T.);
#1088=FACE_BOUND('',#2220,.T.);
#1089=FACE_BOUND('',#2221,.T.);
#1090=FACE_BOUND('',#2222,.T.);
#1091=FACE_BOUND('',#2223,.T.);
#1092=FACE_BOUND('',#2224,.T.);
#1093=FACE_BOUND('',#2225,.T.);
#1094=FACE_BOUND('',#2226,.T.);
#1095=FACE_BOUND('',#2227,.T.);
#1096=FACE_BOUND('',#2228,.T.);
#1097=FACE_BOUND('',#2229,.T.);
#1098=FACE_BOUND('',#2233,.T.);
#1099=FACE_BOUND('',#2234,.T.);
#1100=FACE_BOUND('',#2243,.T.);
#1101=FACE_BOUND('',#2246,.T.);
#1102=FACE_BOUND('',#2249,.T.);
#1103=FACE_BOUND('',#2252,.T.);
#1104=FACE_BOUND('',#2263,.T.);
#1105=FACE_BOUND('',#2267,.T.);
#1106=FACE_BOUND('',#2270,.T.);
#1107=FACE_BOUND('',#2271,.T.);
#1108=FACE_BOUND('',#2272,.T.);
#1109=FACE_BOUND('',#2273,.T.);
#1110=FACE_BOUND('',#2274,.T.);
#1111=FACE_BOUND('',#2275,.T.);
#1112=FACE_BOUND('',#2276,.T.);
#1113=FACE_BOUND('',#2277,.T.);
#1114=FACE_BOUND('',#2278,.T.);
#1115=FACE_BOUND('',#2279,.T.);
#1116=FACE_BOUND('',#2280,.T.);
#1117=FACE_BOUND('',#2281,.T.);
#1118=FACE_BOUND('',#2284,.T.);
#1119=FACE_BOUND('',#2285,.T.);
#1120=FACE_BOUND('',#2286,.T.);
#1121=FACE_BOUND('',#2287,.T.);
#1122=FACE_BOUND('',#2288,.T.);
#1123=FACE_BOUND('',#2289,.T.);
#1124=FACE_BOUND('',#2290,.T.);
#1125=FACE_BOUND('',#2291,.T.);
#1126=FACE_BOUND('',#2292,.T.);
#1127=FACE_BOUND('',#2293,.T.);
#1128=FACE_BOUND('',#2294,.T.);
#1129=FACE_BOUND('',#2295,.T.);
#1130=FACE_BOUND('',#2299,.T.);
#1131=FACE_BOUND('',#2300,.T.);
#1132=FACE_BOUND('',#2304,.T.);
#1133=FACE_BOUND('',#2306,.T.);
#1134=FACE_BOUND('',#2310,.T.);
#1135=FACE_BOUND('',#2312,.T.);
#1136=FACE_BOUND('',#2316,.T.);
#1137=FACE_BOUND('',#2318,.T.);
#1138=FACE_BOUND('',#2322,.T.);
#1139=FACE_BOUND('',#2324,.T.);
#1140=FACE_BOUND('',#2330,.T.);
#1141=FACE_BOUND('',#2334,.T.);
#1142=FACE_BOUND('',#2335,.T.);
#1143=FACE_BOUND('',#2336,.T.);
#1144=FACE_BOUND('',#2337,.T.);
#1145=FACE_BOUND('',#2339,.T.);
#1146=FACE_BOUND('',#2340,.T.);
#1147=FACE_BOUND('',#2341,.T.);
#1148=FACE_BOUND('',#2342,.T.);
#1149=FACE_BOUND('',#2348,.T.);
#1150=FACE_BOUND('',#2352,.T.);
#1151=FACE_BOUND('',#2353,.T.);
#1152=FACE_BOUND('',#2354,.T.);
#1153=FACE_BOUND('',#2355,.T.);
#1154=FACE_BOUND('',#2357,.T.);
#1155=FACE_BOUND('',#2358,.T.);
#1156=FACE_BOUND('',#2359,.T.);
#1157=FACE_BOUND('',#2360,.T.);
#1158=FACE_BOUND('',#2366,.T.);
#1159=FACE_BOUND('',#2370,.T.);
#1160=FACE_BOUND('',#2371,.T.);
#1161=FACE_BOUND('',#2372,.T.);
#1162=FACE_BOUND('',#2373,.T.);
#1163=FACE_BOUND('',#2375,.T.);
#1164=FACE_BOUND('',#2376,.T.);
#1165=FACE_BOUND('',#2377,.T.);
#1166=FACE_BOUND('',#2378,.T.);
#1167=FACE_BOUND('',#2384,.T.);
#1168=FACE_BOUND('',#2388,.T.);
#1169=FACE_BOUND('',#2389,.T.);
#1170=FACE_BOUND('',#2390,.T.);
#1171=FACE_BOUND('',#2391,.T.);
#1172=FACE_BOUND('',#2393,.T.);
#1173=FACE_BOUND('',#2394,.T.);
#1174=FACE_BOUND('',#2395,.T.);
#1175=FACE_BOUND('',#2396,.T.);
#1176=FACE_BOUND('',#2402,.T.);
#1177=FACE_BOUND('',#2420,.T.);
#1178=FACE_BOUND('',#2438,.T.);
#1179=FACE_BOUND('',#2441,.T.);
#1180=FACE_BOUND('',#2446,.T.);
#1181=FACE_BOUND('',#2451,.T.);
#1182=FACE_BOUND('',#2476,.T.);
#1183=FACE_BOUND('',#2479,.T.);
#1184=FACE_BOUND('',#2482,.T.);
#1185=FACE_BOUND('',#2485,.T.);
#1186=FACE_BOUND('',#2488,.T.);
#1187=FACE_BOUND('',#2495,.T.);
#1188=FACE_BOUND('',#2498,.T.);
#1189=FACE_BOUND('',#2503,.T.);
#1190=FACE_BOUND('',#2508,.T.);
#1191=FACE_BOUND('',#2536,.T.);
#1192=FACE_BOUND('',#2539,.T.);
#1193=FACE_BOUND('',#2542,.T.);
#1194=FACE_BOUND('',#2545,.T.);
#1195=FACE_BOUND('',#2548,.T.);
#1196=FACE_BOUND('',#2555,.T.);
#1197=FACE_BOUND('',#2574,.T.);
#1198=FACE_BOUND('',#2580,.T.);
#1199=FACE_BOUND('',#2582,.T.);
#1200=FACE_BOUND('',#2586,.T.);
#1201=FACE_BOUND('',#2588,.T.);
#1202=FACE_BOUND('',#2593,.T.);
#1203=FACE_BOUND('',#2595,.T.);
#1204=FACE_BOUND('',#2597,.T.);
#1205=FACE_BOUND('',#2599,.T.);
#1206=FACE_BOUND('',#2603,.T.);
#1207=FACE_BOUND('',#2605,.T.);
#1208=FACE_BOUND('',#2610,.T.);
#1209=FACE_BOUND('',#2612,.T.);
#1210=FACE_BOUND('',#2614,.T.);
#1211=FACE_BOUND('',#2616,.T.);
#1212=FACE_BOUND('',#2620,.T.);
#1213=FACE_BOUND('',#2622,.T.);
#1214=FACE_BOUND('',#2627,.T.);
#1215=FACE_BOUND('',#2631,.T.);
#1216=FACE_BOUND('',#2712,.T.);
#1217=FACE_BOUND('',#2734,.T.);
#1218=FACE_BOUND('',#2740,.T.);
#1219=FACE_BOUND('',#2742,.T.);
#1220=FACE_BOUND('',#2746,.T.);
#1221=FACE_BOUND('',#2748,.T.);
#1222=FACE_BOUND('',#2753,.T.);
#1223=FACE_BOUND('',#2755,.T.);
#1224=FACE_BOUND('',#2757,.T.);
#1225=FACE_BOUND('',#2759,.T.);
#1226=FACE_BOUND('',#2763,.T.);
#1227=FACE_BOUND('',#2765,.T.);
#1228=FACE_BOUND('',#2770,.T.);
#1229=FACE_BOUND('',#2772,.T.);
#1230=FACE_BOUND('',#2774,.T.);
#1231=FACE_BOUND('',#2776,.T.);
#1232=FACE_BOUND('',#2780,.T.);
#1233=FACE_BOUND('',#2782,.T.);
#1234=FACE_BOUND('',#2787,.T.);
#1235=FACE_BOUND('',#2791,.T.);
#1236=FACE_BOUND('',#2952,.T.);
#1237=FACE_BOUND('',#2972,.T.);
#1238=PLANE('',#11821);
#1239=PLANE('',#11822);
#1240=PLANE('',#11823);
#1241=PLANE('',#11824);
#1242=PLANE('',#11825);
#1243=PLANE('',#11826);
#1244=PLANE('',#11849);
#1245=PLANE('',#11854);
#1246=PLANE('',#11859);
#1247=PLANE('',#11864);
#1248=PLANE('',#11877);
#1249=PLANE('',#11881);
#1250=PLANE('',#11885);
#1251=PLANE('',#11892);
#1252=PLANE('',#11896);
#1253=PLANE('',#11897);
#1254=PLANE('',#11898);
#1255=PLANE('',#11899);
#1256=PLANE('',#11900);
#1257=PLANE('',#11901);
#1258=PLANE('',#11924);
#1259=PLANE('',#11929);
#1260=PLANE('',#11934);
#1261=PLANE('',#11939);
#1262=PLANE('',#11952);
#1263=PLANE('',#11956);
#1264=PLANE('',#11960);
#1265=PLANE('',#11967);
#1266=PLANE('',#11971);
#1267=PLANE('',#11972);
#1268=PLANE('',#11973);
#1269=PLANE('',#11974);
#1270=PLANE('',#11975);
#1271=PLANE('',#11976);
#1272=PLANE('',#11984);
#1273=PLANE('',#11985);
#1274=PLANE('',#11993);
#1275=PLANE('',#11994);
#1276=PLANE('',#12002);
#1277=PLANE('',#12003);
#1278=PLANE('',#12011);
#1279=PLANE('',#12012);
#1280=PLANE('',#12026);
#1281=PLANE('',#12033);
#1282=PLANE('',#12034);
#1283=PLANE('',#12048);
#1284=PLANE('',#12055);
#1285=PLANE('',#12056);
#1286=PLANE('',#12070);
#1287=PLANE('',#12077);
#1288=PLANE('',#12078);
#1289=PLANE('',#12092);
#1290=PLANE('',#12099);
#1291=PLANE('',#12100);
#1292=PLANE('',#12102);
#1293=PLANE('',#12110);
#1294=PLANE('',#12118);
#1295=PLANE('',#12119);
#1296=PLANE('',#12120);
#1297=PLANE('',#12121);
#1298=PLANE('',#12122);
#1299=PLANE('',#12123);
#1300=PLANE('',#12124);
#1301=PLANE('',#12125);
#1302=PLANE('',#12126);
#1303=PLANE('',#12128);
#1304=PLANE('',#12136);
#1305=PLANE('',#12144);
#1306=PLANE('',#12145);
#1307=PLANE('',#12146);
#1308=PLANE('',#12147);
#1309=PLANE('',#12148);
#1310=PLANE('',#12149);
#1311=PLANE('',#12150);
#1312=PLANE('',#12151);
#1313=PLANE('',#12152);
#1314=PLANE('',#12168);
#1315=PLANE('',#12171);
#1316=PLANE('',#12183);
#1317=PLANE('',#12192);
#1318=PLANE('',#12223);
#1319=PLANE('',#12228);
#1320=PLANE('',#12233);
#1321=PLANE('',#12239);
#1322=PLANE('',#12244);
#1323=PLANE('',#12253);
#1324=PLANE('',#12257);
#1325=PLANE('',#12258);
#1326=PLANE('',#12260);
#1327=PLANE('',#12265);
#1328=PLANE('',#12268);
#1329=PLANE('',#12273);
#1330=PLANE('',#12296);
#1331=PLANE('',#12299);
#1332=PLANE('',#12311);
#1333=PLANE('',#12320);
#1334=PLANE('',#12353);
#1335=PLANE('',#12358);
#1336=PLANE('',#12363);
#1337=PLANE('',#12368);
#1338=PLANE('',#12373);
#1339=PLANE('',#12378);
#1340=PLANE('',#12387);
#1341=PLANE('',#12391);
#1342=PLANE('',#12392);
#1343=PLANE('',#12394);
#1344=PLANE('',#12399);
#1345=PLANE('',#12402);
#1346=PLANE('',#12407);
#1347=PLANE('',#12416);
#1348=PLANE('',#12424);
#1349=PLANE('',#12432);
#1350=PLANE('',#12433);
#1351=PLANE('',#12434);
#1352=PLANE('',#12435);
#1353=PLANE('',#12436);
#1354=PLANE('',#12437);
#1355=PLANE('',#12438);
#1356=PLANE('',#12439);
#1357=PLANE('',#12440);
#1358=PLANE('',#12482);
#1359=PLANE('',#12483);
#1360=PLANE('',#12485);
#1361=PLANE('',#12486);
#1362=PLANE('',#12487);
#1363=PLANE('',#12492);
#1364=PLANE('',#12493);
#1365=PLANE('',#12501);
#1366=PLANE('',#12502);
#1367=PLANE('',#12510);
#1368=PLANE('',#12511);
#1369=PLANE('',#12513);
#1370=PLANE('',#12518);
#1371=PLANE('',#12525);
#1372=PLANE('',#12526);
#1373=PLANE('',#12534);
#1374=PLANE('',#12535);
#1375=PLANE('',#12537);
#1376=PLANE('',#12542);
#1377=PLANE('',#12549);
#1378=PLANE('',#12550);
#1379=PLANE('',#12558);
#1380=PLANE('',#12559);
#1381=PLANE('',#12561);
#1382=PLANE('',#12562);
#1383=PLANE('',#12563);
#1384=PLANE('',#12564);
#1385=PLANE('',#12591);
#1386=PLANE('',#12592);
#1387=PLANE('',#12595);
#1388=PLANE('',#12598);
#1389=PLANE('',#12601);
#1390=PLANE('',#12604);
#1391=PLANE('',#12607);
#1392=PLANE('',#12610);
#1393=PLANE('',#12613);
#1394=PLANE('',#12616);
#1395=PLANE('',#12619);
#1396=PLANE('',#12622);
#1397=PLANE('',#12625);
#1398=PLANE('',#12628);
#1399=PLANE('',#12631);
#1400=PLANE('',#12634);
#1401=PLANE('',#12637);
#1402=PLANE('',#12640);
#1403=PLANE('',#12643);
#1404=PLANE('',#12646);
#1405=PLANE('',#12649);
#1406=PLANE('',#12650);
#1407=PLANE('',#12654);
#1408=PLANE('',#12658);
#1409=PLANE('',#12664);
#1410=PLANE('',#12665);
#1411=PLANE('',#12666);
#1412=PLANE('',#12669);
#1413=PLANE('',#12674);
#1414=PLANE('',#12675);
#1415=PLANE('',#12678);
#1416=PLANE('',#12679);
#1417=PLANE('',#12681);
#1418=PLANE('',#12682);
#1419=PLANE('',#12683);
#1420=PLANE('',#12688);
#1421=PLANE('',#12689);
#1422=PLANE('',#12697);
#1423=PLANE('',#12698);
#1424=PLANE('',#12706);
#1425=PLANE('',#12707);
#1426=PLANE('',#12709);
#1427=PLANE('',#12714);
#1428=PLANE('',#12721);
#1429=PLANE('',#12722);
#1430=PLANE('',#12730);
#1431=PLANE('',#12731);
#1432=PLANE('',#12733);
#1433=PLANE('',#12738);
#1434=PLANE('',#12745);
#1435=PLANE('',#12746);
#1436=PLANE('',#12754);
#1437=PLANE('',#12755);
#1438=PLANE('',#12757);
#1439=PLANE('',#12758);
#1440=PLANE('',#12759);
#1441=PLANE('',#12760);
#1442=PLANE('',#12807);
#1443=PLANE('',#12808);
#1444=PLANE('',#12811);
#1445=PLANE('',#12814);
#1446=PLANE('',#12817);
#1447=PLANE('',#12820);
#1448=PLANE('',#12823);
#1449=PLANE('',#12826);
#1450=PLANE('',#12829);
#1451=PLANE('',#12832);
#1452=PLANE('',#12835);
#1453=PLANE('',#12838);
#1454=PLANE('',#12841);
#1455=PLANE('',#12844);
#1456=PLANE('',#12847);
#1457=PLANE('',#12850);
#1458=PLANE('',#12853);
#1459=PLANE('',#12856);
#1460=PLANE('',#12859);
#1461=PLANE('',#12862);
#1462=PLANE('',#12865);
#1463=PLANE('',#12868);
#1464=PLANE('',#12871);
#1465=PLANE('',#12874);
#1466=PLANE('',#12877);
#1467=PLANE('',#12880);
#1468=PLANE('',#12883);
#1469=PLANE('',#12886);
#1470=PLANE('',#12889);
#1471=PLANE('',#12892);
#1472=PLANE('',#12895);
#1473=PLANE('',#12898);
#1474=PLANE('',#12901);
#1475=PLANE('',#12904);
#1476=PLANE('',#12907);
#1477=PLANE('',#12910);
#1478=PLANE('',#12913);
#1479=PLANE('',#12916);
#1480=PLANE('',#12919);
#1481=PLANE('',#12922);
#1482=PLANE('',#12925);
#1483=PLANE('',#12926);
#1484=PLANE('',#12930);
#1485=PLANE('',#12931);
#1486=PLANE('',#12932);
#1487=PLANE('',#12933);
#1488=PLANE('',#12934);
#1489=PLANE('',#12935);
#1490=PLANE('',#12936);
#1491=PLANE('',#12937);
#1492=PLANE('',#12938);
#1493=PLANE('',#12939);
#1494=PLANE('',#12941);
#1495=PLANE('',#12942);
#1496=PLANE('',#12943);
#1497=PLANE('',#12944);
#1498=PLANE('',#12945);
#1499=PLANE('',#12946);
#1500=PLANE('',#12947);
#1501=PLANE('',#12948);
#1502=PLANE('',#12956);
#1503=FACE_OUTER_BOUND('',#2151,.T.);
#1504=FACE_OUTER_BOUND('',#2152,.T.);
#1505=FACE_OUTER_BOUND('',#2153,.T.);
#1506=FACE_OUTER_BOUND('',#2154,.T.);
#1507=FACE_OUTER_BOUND('',#2155,.T.);
#1508=FACE_OUTER_BOUND('',#2156,.T.);
#1509=FACE_OUTER_BOUND('',#2157,.T.);
#1510=FACE_OUTER_BOUND('',#2158,.T.);
#1511=FACE_OUTER_BOUND('',#2159,.T.);
#1512=FACE_OUTER_BOUND('',#2164,.T.);
#1513=FACE_OUTER_BOUND('',#2169,.T.);
#1514=FACE_OUTER_BOUND('',#2170,.T.);
#1515=FACE_OUTER_BOUND('',#2171,.T.);
#1516=FACE_OUTER_BOUND('',#2172,.T.);
#1517=FACE_OUTER_BOUND('',#2173,.T.);
#1518=FACE_OUTER_BOUND('',#2174,.T.);
#1519=FACE_OUTER_BOUND('',#2175,.T.);
#1520=FACE_OUTER_BOUND('',#2176,.T.);
#1521=FACE_OUTER_BOUND('',#2178,.T.);
#1522=FACE_OUTER_BOUND('',#2179,.T.);
#1523=FACE_OUTER_BOUND('',#2181,.T.);
#1524=FACE_OUTER_BOUND('',#2182,.T.);
#1525=FACE_OUTER_BOUND('',#2184,.T.);
#1526=FACE_OUTER_BOUND('',#2185,.T.);
#1527=FACE_OUTER_BOUND('',#2187,.T.);
#1528=FACE_OUTER_BOUND('',#2188,.T.);
#1529=FACE_OUTER_BOUND('',#2189,.T.);
#1530=FACE_OUTER_BOUND('',#2190,.T.);
#1531=FACE_OUTER_BOUND('',#2191,.T.);
#1532=FACE_OUTER_BOUND('',#2192,.T.);
#1533=FACE_OUTER_BOUND('',#2193,.T.);
#1534=FACE_OUTER_BOUND('',#2194,.T.);
#1535=FACE_OUTER_BOUND('',#2195,.T.);
#1536=FACE_OUTER_BOUND('',#2196,.T.);
#1537=FACE_OUTER_BOUND('',#2198,.T.);
#1538=FACE_OUTER_BOUND('',#2199,.T.);
#1539=FACE_OUTER_BOUND('',#2200,.T.);
#1540=FACE_OUTER_BOUND('',#2202,.T.);
#1541=FACE_OUTER_BOUND('',#2203,.T.);
#1542=FACE_OUTER_BOUND('',#2216,.T.);
#1543=FACE_OUTER_BOUND('',#2217,.T.);
#1544=FACE_OUTER_BOUND('',#2230,.T.);
#1545=FACE_OUTER_BOUND('',#2231,.T.);
#1546=FACE_OUTER_BOUND('',#2232,.T.);
#1547=FACE_OUTER_BOUND('',#2235,.T.);
#1548=FACE_OUTER_BOUND('',#2236,.T.);
#1549=FACE_OUTER_BOUND('',#2237,.T.);
#1550=FACE_OUTER_BOUND('',#2238,.T.);
#1551=FACE_OUTER_BOUND('',#2239,.T.);
#1552=FACE_OUTER_BOUND('',#2240,.T.);
#1553=FACE_OUTER_BOUND('',#2241,.T.);
#1554=FACE_OUTER_BOUND('',#2242,.T.);
#1555=FACE_OUTER_BOUND('',#2244,.T.);
#1556=FACE_OUTER_BOUND('',#2245,.T.);
#1557=FACE_OUTER_BOUND('',#2247,.T.);
#1558=FACE_OUTER_BOUND('',#2248,.T.);
#1559=FACE_OUTER_BOUND('',#2250,.T.);
#1560=FACE_OUTER_BOUND('',#2251,.T.);
#1561=FACE_OUTER_BOUND('',#2253,.T.);
#1562=FACE_OUTER_BOUND('',#2254,.T.);
#1563=FACE_OUTER_BOUND('',#2255,.T.);
#1564=FACE_OUTER_BOUND('',#2256,.T.);
#1565=FACE_OUTER_BOUND('',#2257,.T.);
#1566=FACE_OUTER_BOUND('',#2258,.T.);
#1567=FACE_OUTER_BOUND('',#2259,.T.);
#1568=FACE_OUTER_BOUND('',#2260,.T.);
#1569=FACE_OUTER_BOUND('',#2261,.T.);
#1570=FACE_OUTER_BOUND('',#2262,.T.);
#1571=FACE_OUTER_BOUND('',#2264,.T.);
#1572=FACE_OUTER_BOUND('',#2265,.T.);
#1573=FACE_OUTER_BOUND('',#2266,.T.);
#1574=FACE_OUTER_BOUND('',#2268,.T.);
#1575=FACE_OUTER_BOUND('',#2269,.T.);
#1576=FACE_OUTER_BOUND('',#2282,.T.);
#1577=FACE_OUTER_BOUND('',#2283,.T.);
#1578=FACE_OUTER_BOUND('',#2296,.T.);
#1579=FACE_OUTER_BOUND('',#2297,.T.);
#1580=FACE_OUTER_BOUND('',#2298,.T.);
#1581=FACE_OUTER_BOUND('',#2301,.T.);
#1582=FACE_OUTER_BOUND('',#2302,.T.);
#1583=FACE_OUTER_BOUND('',#2303,.T.);
#1584=FACE_OUTER_BOUND('',#2305,.T.);
#1585=FACE_OUTER_BOUND('',#2307,.T.);
#1586=FACE_OUTER_BOUND('',#2308,.T.);
#1587=FACE_OUTER_BOUND('',#2309,.T.);
#1588=FACE_OUTER_BOUND('',#2311,.T.);
#1589=FACE_OUTER_BOUND('',#2313,.T.);
#1590=FACE_OUTER_BOUND('',#2314,.T.);
#1591=FACE_OUTER_BOUND('',#2315,.T.);
#1592=FACE_OUTER_BOUND('',#2317,.T.);
#1593=FACE_OUTER_BOUND('',#2319,.T.);
#1594=FACE_OUTER_BOUND('',#2320,.T.);
#1595=FACE_OUTER_BOUND('',#2321,.T.);
#1596=FACE_OUTER_BOUND('',#2323,.T.);
#1597=FACE_OUTER_BOUND('',#2325,.T.);
#1598=FACE_OUTER_BOUND('',#2326,.T.);
#1599=FACE_OUTER_BOUND('',#2327,.T.);
#1600=FACE_OUTER_BOUND('',#2328,.T.);
#1601=FACE_OUTER_BOUND('',#2329,.T.);
#1602=FACE_OUTER_BOUND('',#2331,.T.);
#1603=FACE_OUTER_BOUND('',#2332,.T.);
#1604=FACE_OUTER_BOUND('',#2333,.T.);
#1605=FACE_OUTER_BOUND('',#2338,.T.);
#1606=FACE_OUTER_BOUND('',#2343,.T.);
#1607=FACE_OUTER_BOUND('',#2344,.T.);
#1608=FACE_OUTER_BOUND('',#2345,.T.);
#1609=FACE_OUTER_BOUND('',#2346,.T.);
#1610=FACE_OUTER_BOUND('',#2347,.T.);
#1611=FACE_OUTER_BOUND('',#2349,.T.);
#1612=FACE_OUTER_BOUND('',#2350,.T.);
#1613=FACE_OUTER_BOUND('',#2351,.T.);
#1614=FACE_OUTER_BOUND('',#2356,.T.);
#1615=FACE_OUTER_BOUND('',#2361,.T.);
#1616=FACE_OUTER_BOUND('',#2362,.T.);
#1617=FACE_OUTER_BOUND('',#2363,.T.);
#1618=FACE_OUTER_BOUND('',#2364,.T.);
#1619=FACE_OUTER_BOUND('',#2365,.T.);
#1620=FACE_OUTER_BOUND('',#2367,.T.);
#1621=FACE_OUTER_BOUND('',#2368,.T.);
#1622=FACE_OUTER_BOUND('',#2369,.T.);
#1623=FACE_OUTER_BOUND('',#2374,.T.);
#1624=FACE_OUTER_BOUND('',#2379,.T.);
#1625=FACE_OUTER_BOUND('',#2380,.T.);
#1626=FACE_OUTER_BOUND('',#2381,.T.);
#1627=FACE_OUTER_BOUND('',#2382,.T.);
#1628=FACE_OUTER_BOUND('',#2383,.T.);
#1629=FACE_OUTER_BOUND('',#2385,.T.);
#1630=FACE_OUTER_BOUND('',#2386,.T.);
#1631=FACE_OUTER_BOUND('',#2387,.T.);
#1632=FACE_OUTER_BOUND('',#2392,.T.);
#1633=FACE_OUTER_BOUND('',#2397,.T.);
#1634=FACE_OUTER_BOUND('',#2398,.T.);
#1635=FACE_OUTER_BOUND('',#2399,.T.);
#1636=FACE_OUTER_BOUND('',#2400,.T.);
#1637=FACE_OUTER_BOUND('',#2401,.T.);
#1638=FACE_OUTER_BOUND('',#2403,.T.);
#1639=FACE_OUTER_BOUND('',#2404,.T.);
#1640=FACE_OUTER_BOUND('',#2405,.T.);
#1641=FACE_OUTER_BOUND('',#2406,.T.);
#1642=FACE_OUTER_BOUND('',#2407,.T.);
#1643=FACE_OUTER_BOUND('',#2408,.T.);
#1644=FACE_OUTER_BOUND('',#2409,.T.);
#1645=FACE_OUTER_BOUND('',#2410,.T.);
#1646=FACE_OUTER_BOUND('',#2411,.T.);
#1647=FACE_OUTER_BOUND('',#2412,.T.);
#1648=FACE_OUTER_BOUND('',#2413,.T.);
#1649=FACE_OUTER_BOUND('',#2414,.T.);
#1650=FACE_OUTER_BOUND('',#2415,.T.);
#1651=FACE_OUTER_BOUND('',#2416,.T.);
#1652=FACE_OUTER_BOUND('',#2417,.T.);
#1653=FACE_OUTER_BOUND('',#2418,.T.);
#1654=FACE_OUTER_BOUND('',#2419,.T.);
#1655=FACE_OUTER_BOUND('',#2421,.T.);
#1656=FACE_OUTER_BOUND('',#2422,.T.);
#1657=FACE_OUTER_BOUND('',#2423,.T.);
#1658=FACE_OUTER_BOUND('',#2424,.T.);
#1659=FACE_OUTER_BOUND('',#2425,.T.);
#1660=FACE_OUTER_BOUND('',#2426,.T.);
#1661=FACE_OUTER_BOUND('',#2427,.T.);
#1662=FACE_OUTER_BOUND('',#2428,.T.);
#1663=FACE_OUTER_BOUND('',#2429,.T.);
#1664=FACE_OUTER_BOUND('',#2430,.T.);
#1665=FACE_OUTER_BOUND('',#2431,.T.);
#1666=FACE_OUTER_BOUND('',#2432,.T.);
#1667=FACE_OUTER_BOUND('',#2433,.T.);
#1668=FACE_OUTER_BOUND('',#2434,.T.);
#1669=FACE_OUTER_BOUND('',#2435,.T.);
#1670=FACE_OUTER_BOUND('',#2436,.T.);
#1671=FACE_OUTER_BOUND('',#2437,.T.);
#1672=FACE_OUTER_BOUND('',#2439,.T.);
#1673=FACE_OUTER_BOUND('',#2440,.T.);
#1674=FACE_OUTER_BOUND('',#2442,.T.);
#1675=FACE_OUTER_BOUND('',#2443,.T.);
#1676=FACE_OUTER_BOUND('',#2444,.T.);
#1677=FACE_OUTER_BOUND('',#2445,.T.);
#1678=FACE_OUTER_BOUND('',#2447,.T.);
#1679=FACE_OUTER_BOUND('',#2448,.T.);
#1680=FACE_OUTER_BOUND('',#2449,.T.);
#1681=FACE_OUTER_BOUND('',#2450,.T.);
#1682=FACE_OUTER_BOUND('',#2452,.T.);
#1683=FACE_OUTER_BOUND('',#2453,.T.);
#1684=FACE_OUTER_BOUND('',#2454,.T.);
#1685=FACE_OUTER_BOUND('',#2455,.T.);
#1686=FACE_OUTER_BOUND('',#2456,.T.);
#1687=FACE_OUTER_BOUND('',#2457,.T.);
#1688=FACE_OUTER_BOUND('',#2458,.T.);
#1689=FACE_OUTER_BOUND('',#2459,.T.);
#1690=FACE_OUTER_BOUND('',#2460,.T.);
#1691=FACE_OUTER_BOUND('',#2461,.T.);
#1692=FACE_OUTER_BOUND('',#2462,.T.);
#1693=FACE_OUTER_BOUND('',#2463,.T.);
#1694=FACE_OUTER_BOUND('',#2464,.T.);
#1695=FACE_OUTER_BOUND('',#2465,.T.);
#1696=FACE_OUTER_BOUND('',#2466,.T.);
#1697=FACE_OUTER_BOUND('',#2467,.T.);
#1698=FACE_OUTER_BOUND('',#2468,.T.);
#1699=FACE_OUTER_BOUND('',#2469,.T.);
#1700=FACE_OUTER_BOUND('',#2470,.T.);
#1701=FACE_OUTER_BOUND('',#2471,.T.);
#1702=FACE_OUTER_BOUND('',#2472,.T.);
#1703=FACE_OUTER_BOUND('',#2473,.T.);
#1704=FACE_OUTER_BOUND('',#2474,.T.);
#1705=FACE_OUTER_BOUND('',#2475,.T.);
#1706=FACE_OUTER_BOUND('',#2477,.T.);
#1707=FACE_OUTER_BOUND('',#2478,.T.);
#1708=FACE_OUTER_BOUND('',#2480,.T.);
#1709=FACE_OUTER_BOUND('',#2481,.T.);
#1710=FACE_OUTER_BOUND('',#2483,.T.);
#1711=FACE_OUTER_BOUND('',#2484,.T.);
#1712=FACE_OUTER_BOUND('',#2486,.T.);
#1713=FACE_OUTER_BOUND('',#2487,.T.);
#1714=FACE_OUTER_BOUND('',#2489,.T.);
#1715=FACE_OUTER_BOUND('',#2490,.T.);
#1716=FACE_OUTER_BOUND('',#2491,.T.);
#1717=FACE_OUTER_BOUND('',#2492,.T.);
#1718=FACE_OUTER_BOUND('',#2493,.T.);
#1719=FACE_OUTER_BOUND('',#2494,.T.);
#1720=FACE_OUTER_BOUND('',#2496,.T.);
#1721=FACE_OUTER_BOUND('',#2497,.T.);
#1722=FACE_OUTER_BOUND('',#2499,.T.);
#1723=FACE_OUTER_BOUND('',#2500,.T.);
#1724=FACE_OUTER_BOUND('',#2501,.T.);
#1725=FACE_OUTER_BOUND('',#2502,.T.);
#1726=FACE_OUTER_BOUND('',#2504,.T.);
#1727=FACE_OUTER_BOUND('',#2505,.T.);
#1728=FACE_OUTER_BOUND('',#2506,.T.);
#1729=FACE_OUTER_BOUND('',#2507,.T.);
#1730=FACE_OUTER_BOUND('',#2509,.T.);
#1731=FACE_OUTER_BOUND('',#2510,.T.);
#1732=FACE_OUTER_BOUND('',#2511,.T.);
#1733=FACE_OUTER_BOUND('',#2512,.T.);
#1734=FACE_OUTER_BOUND('',#2513,.T.);
#1735=FACE_OUTER_BOUND('',#2514,.T.);
#1736=FACE_OUTER_BOUND('',#2515,.T.);
#1737=FACE_OUTER_BOUND('',#2516,.T.);
#1738=FACE_OUTER_BOUND('',#2517,.T.);
#1739=FACE_OUTER_BOUND('',#2518,.T.);
#1740=FACE_OUTER_BOUND('',#2519,.T.);
#1741=FACE_OUTER_BOUND('',#2520,.T.);
#1742=FACE_OUTER_BOUND('',#2521,.T.);
#1743=FACE_OUTER_BOUND('',#2522,.T.);
#1744=FACE_OUTER_BOUND('',#2523,.T.);
#1745=FACE_OUTER_BOUND('',#2524,.T.);
#1746=FACE_OUTER_BOUND('',#2525,.T.);
#1747=FACE_OUTER_BOUND('',#2526,.T.);
#1748=FACE_OUTER_BOUND('',#2527,.T.);
#1749=FACE_OUTER_BOUND('',#2528,.T.);
#1750=FACE_OUTER_BOUND('',#2529,.T.);
#1751=FACE_OUTER_BOUND('',#2530,.T.);
#1752=FACE_OUTER_BOUND('',#2531,.T.);
#1753=FACE_OUTER_BOUND('',#2532,.T.);
#1754=FACE_OUTER_BOUND('',#2533,.T.);
#1755=FACE_OUTER_BOUND('',#2534,.T.);
#1756=FACE_OUTER_BOUND('',#2535,.T.);
#1757=FACE_OUTER_BOUND('',#2537,.T.);
#1758=FACE_OUTER_BOUND('',#2538,.T.);
#1759=FACE_OUTER_BOUND('',#2540,.T.);
#1760=FACE_OUTER_BOUND('',#2541,.T.);
#1761=FACE_OUTER_BOUND('',#2543,.T.);
#1762=FACE_OUTER_BOUND('',#2544,.T.);
#1763=FACE_OUTER_BOUND('',#2546,.T.);
#1764=FACE_OUTER_BOUND('',#2547,.T.);
#1765=FACE_OUTER_BOUND('',#2549,.T.);
#1766=FACE_OUTER_BOUND('',#2550,.T.);
#1767=FACE_OUTER_BOUND('',#2551,.T.);
#1768=FACE_OUTER_BOUND('',#2552,.T.);
#1769=FACE_OUTER_BOUND('',#2553,.T.);
#1770=FACE_OUTER_BOUND('',#2554,.T.);
#1771=FACE_OUTER_BOUND('',#2556,.T.);
#1772=FACE_OUTER_BOUND('',#2557,.T.);
#1773=FACE_OUTER_BOUND('',#2558,.T.);
#1774=FACE_OUTER_BOUND('',#2559,.T.);
#1775=FACE_OUTER_BOUND('',#2560,.T.);
#1776=FACE_OUTER_BOUND('',#2561,.T.);
#1777=FACE_OUTER_BOUND('',#2562,.T.);
#1778=FACE_OUTER_BOUND('',#2563,.T.);
#1779=FACE_OUTER_BOUND('',#2564,.T.);
#1780=FACE_OUTER_BOUND('',#2565,.T.);
#1781=FACE_OUTER_BOUND('',#2566,.T.);
#1782=FACE_OUTER_BOUND('',#2567,.T.);
#1783=FACE_OUTER_BOUND('',#2568,.T.);
#1784=FACE_OUTER_BOUND('',#2569,.T.);
#1785=FACE_OUTER_BOUND('',#2570,.T.);
#1786=FACE_OUTER_BOUND('',#2571,.T.);
#1787=FACE_OUTER_BOUND('',#2572,.T.);
#1788=FACE_OUTER_BOUND('',#2573,.T.);
#1789=FACE_OUTER_BOUND('',#2575,.T.);
#1790=FACE_OUTER_BOUND('',#2576,.T.);
#1791=FACE_OUTER_BOUND('',#2577,.T.);
#1792=FACE_OUTER_BOUND('',#2578,.T.);
#1793=FACE_OUTER_BOUND('',#2579,.T.);
#1794=FACE_OUTER_BOUND('',#2581,.T.);
#1795=FACE_OUTER_BOUND('',#2583,.T.);
#1796=FACE_OUTER_BOUND('',#2584,.T.);
#1797=FACE_OUTER_BOUND('',#2585,.T.);
#1798=FACE_OUTER_BOUND('',#2587,.T.);
#1799=FACE_OUTER_BOUND('',#2589,.T.);
#1800=FACE_OUTER_BOUND('',#2590,.T.);
#1801=FACE_OUTER_BOUND('',#2591,.T.);
#1802=FACE_OUTER_BOUND('',#2592,.T.);
#1803=FACE_OUTER_BOUND('',#2594,.T.);
#1804=FACE_OUTER_BOUND('',#2596,.T.);
#1805=FACE_OUTER_BOUND('',#2598,.T.);
#1806=FACE_OUTER_BOUND('',#2600,.T.);
#1807=FACE_OUTER_BOUND('',#2601,.T.);
#1808=FACE_OUTER_BOUND('',#2602,.T.);
#1809=FACE_OUTER_BOUND('',#2604,.T.);
#1810=FACE_OUTER_BOUND('',#2606,.T.);
#1811=FACE_OUTER_BOUND('',#2607,.T.);
#1812=FACE_OUTER_BOUND('',#2608,.T.);
#1813=FACE_OUTER_BOUND('',#2609,.T.);
#1814=FACE_OUTER_BOUND('',#2611,.T.);
#1815=FACE_OUTER_BOUND('',#2613,.T.);
#1816=FACE_OUTER_BOUND('',#2615,.T.);
#1817=FACE_OUTER_BOUND('',#2617,.T.);
#1818=FACE_OUTER_BOUND('',#2618,.T.);
#1819=FACE_OUTER_BOUND('',#2619,.T.);
#1820=FACE_OUTER_BOUND('',#2621,.T.);
#1821=FACE_OUTER_BOUND('',#2623,.T.);
#1822=FACE_OUTER_BOUND('',#2624,.T.);
#1823=FACE_OUTER_BOUND('',#2625,.T.);
#1824=FACE_OUTER_BOUND('',#2626,.T.);
#1825=FACE_OUTER_BOUND('',#2628,.T.);
#1826=FACE_OUTER_BOUND('',#2629,.T.);
#1827=FACE_OUTER_BOUND('',#2630,.T.);
#1828=FACE_OUTER_BOUND('',#2632,.T.);
#1829=FACE_OUTER_BOUND('',#2633,.T.);
#1830=FACE_OUTER_BOUND('',#2634,.T.);
#1831=FACE_OUTER_BOUND('',#2635,.T.);
#1832=FACE_OUTER_BOUND('',#2636,.T.);
#1833=FACE_OUTER_BOUND('',#2637,.T.);
#1834=FACE_OUTER_BOUND('',#2638,.T.);
#1835=FACE_OUTER_BOUND('',#2639,.T.);
#1836=FACE_OUTER_BOUND('',#2640,.T.);
#1837=FACE_OUTER_BOUND('',#2641,.T.);
#1838=FACE_OUTER_BOUND('',#2642,.T.);
#1839=FACE_OUTER_BOUND('',#2643,.T.);
#1840=FACE_OUTER_BOUND('',#2644,.T.);
#1841=FACE_OUTER_BOUND('',#2645,.T.);
#1842=FACE_OUTER_BOUND('',#2646,.T.);
#1843=FACE_OUTER_BOUND('',#2647,.T.);
#1844=FACE_OUTER_BOUND('',#2648,.T.);
#1845=FACE_OUTER_BOUND('',#2649,.T.);
#1846=FACE_OUTER_BOUND('',#2650,.T.);
#1847=FACE_OUTER_BOUND('',#2651,.T.);
#1848=FACE_OUTER_BOUND('',#2652,.T.);
#1849=FACE_OUTER_BOUND('',#2653,.T.);
#1850=FACE_OUTER_BOUND('',#2654,.T.);
#1851=FACE_OUTER_BOUND('',#2655,.T.);
#1852=FACE_OUTER_BOUND('',#2656,.T.);
#1853=FACE_OUTER_BOUND('',#2657,.T.);
#1854=FACE_OUTER_BOUND('',#2658,.T.);
#1855=FACE_OUTER_BOUND('',#2659,.T.);
#1856=FACE_OUTER_BOUND('',#2660,.T.);
#1857=FACE_OUTER_BOUND('',#2661,.T.);
#1858=FACE_OUTER_BOUND('',#2662,.T.);
#1859=FACE_OUTER_BOUND('',#2663,.T.);
#1860=FACE_OUTER_BOUND('',#2664,.T.);
#1861=FACE_OUTER_BOUND('',#2665,.T.);
#1862=FACE_OUTER_BOUND('',#2666,.T.);
#1863=FACE_OUTER_BOUND('',#2667,.T.);
#1864=FACE_OUTER_BOUND('',#2668,.T.);
#1865=FACE_OUTER_BOUND('',#2669,.T.);
#1866=FACE_OUTER_BOUND('',#2670,.T.);
#1867=FACE_OUTER_BOUND('',#2671,.T.);
#1868=FACE_OUTER_BOUND('',#2672,.T.);
#1869=FACE_OUTER_BOUND('',#2673,.T.);
#1870=FACE_OUTER_BOUND('',#2674,.T.);
#1871=FACE_OUTER_BOUND('',#2675,.T.);
#1872=FACE_OUTER_BOUND('',#2676,.T.);
#1873=FACE_OUTER_BOUND('',#2677,.T.);
#1874=FACE_OUTER_BOUND('',#2678,.T.);
#1875=FACE_OUTER_BOUND('',#2679,.T.);
#1876=FACE_OUTER_BOUND('',#2680,.T.);
#1877=FACE_OUTER_BOUND('',#2681,.T.);
#1878=FACE_OUTER_BOUND('',#2682,.T.);
#1879=FACE_OUTER_BOUND('',#2683,.T.);
#1880=FACE_OUTER_BOUND('',#2684,.T.);
#1881=FACE_OUTER_BOUND('',#2685,.T.);
#1882=FACE_OUTER_BOUND('',#2686,.T.);
#1883=FACE_OUTER_BOUND('',#2687,.T.);
#1884=FACE_OUTER_BOUND('',#2688,.T.);
#1885=FACE_OUTER_BOUND('',#2689,.T.);
#1886=FACE_OUTER_BOUND('',#2690,.T.);
#1887=FACE_OUTER_BOUND('',#2691,.T.);
#1888=FACE_OUTER_BOUND('',#2692,.T.);
#1889=FACE_OUTER_BOUND('',#2693,.T.);
#1890=FACE_OUTER_BOUND('',#2694,.T.);
#1891=FACE_OUTER_BOUND('',#2695,.T.);
#1892=FACE_OUTER_BOUND('',#2696,.T.);
#1893=FACE_OUTER_BOUND('',#2697,.T.);
#1894=FACE_OUTER_BOUND('',#2698,.T.);
#1895=FACE_OUTER_BOUND('',#2699,.T.);
#1896=FACE_OUTER_BOUND('',#2700,.T.);
#1897=FACE_OUTER_BOUND('',#2701,.T.);
#1898=FACE_OUTER_BOUND('',#2702,.T.);
#1899=FACE_OUTER_BOUND('',#2703,.T.);
#1900=FACE_OUTER_BOUND('',#2704,.T.);
#1901=FACE_OUTER_BOUND('',#2705,.T.);
#1902=FACE_OUTER_BOUND('',#2706,.T.);
#1903=FACE_OUTER_BOUND('',#2707,.T.);
#1904=FACE_OUTER_BOUND('',#2708,.T.);
#1905=FACE_OUTER_BOUND('',#2709,.T.);
#1906=FACE_OUTER_BOUND('',#2710,.T.);
#1907=FACE_OUTER_BOUND('',#2711,.T.);
#1908=FACE_OUTER_BOUND('',#2713,.T.);
#1909=FACE_OUTER_BOUND('',#2714,.T.);
#1910=FACE_OUTER_BOUND('',#2715,.T.);
#1911=FACE_OUTER_BOUND('',#2716,.T.);
#1912=FACE_OUTER_BOUND('',#2717,.T.);
#1913=FACE_OUTER_BOUND('',#2718,.T.);
#1914=FACE_OUTER_BOUND('',#2719,.T.);
#1915=FACE_OUTER_BOUND('',#2720,.T.);
#1916=FACE_OUTER_BOUND('',#2721,.T.);
#1917=FACE_OUTER_BOUND('',#2722,.T.);
#1918=FACE_OUTER_BOUND('',#2723,.T.);
#1919=FACE_OUTER_BOUND('',#2724,.T.);
#1920=FACE_OUTER_BOUND('',#2725,.T.);
#1921=FACE_OUTER_BOUND('',#2726,.T.);
#1922=FACE_OUTER_BOUND('',#2727,.T.);
#1923=FACE_OUTER_BOUND('',#2728,.T.);
#1924=FACE_OUTER_BOUND('',#2729,.T.);
#1925=FACE_OUTER_BOUND('',#2730,.T.);
#1926=FACE_OUTER_BOUND('',#2731,.T.);
#1927=FACE_OUTER_BOUND('',#2732,.T.);
#1928=FACE_OUTER_BOUND('',#2733,.T.);
#1929=FACE_OUTER_BOUND('',#2735,.T.);
#1930=FACE_OUTER_BOUND('',#2736,.T.);
#1931=FACE_OUTER_BOUND('',#2737,.T.);
#1932=FACE_OUTER_BOUND('',#2738,.T.);
#1933=FACE_OUTER_BOUND('',#2739,.T.);
#1934=FACE_OUTER_BOUND('',#2741,.T.);
#1935=FACE_OUTER_BOUND('',#2743,.T.);
#1936=FACE_OUTER_BOUND('',#2744,.T.);
#1937=FACE_OUTER_BOUND('',#2745,.T.);
#1938=FACE_OUTER_BOUND('',#2747,.T.);
#1939=FACE_OUTER_BOUND('',#2749,.T.);
#1940=FACE_OUTER_BOUND('',#2750,.T.);
#1941=FACE_OUTER_BOUND('',#2751,.T.);
#1942=FACE_OUTER_BOUND('',#2752,.T.);
#1943=FACE_OUTER_BOUND('',#2754,.T.);
#1944=FACE_OUTER_BOUND('',#2756,.T.);
#1945=FACE_OUTER_BOUND('',#2758,.T.);
#1946=FACE_OUTER_BOUND('',#2760,.T.);
#1947=FACE_OUTER_BOUND('',#2761,.T.);
#1948=FACE_OUTER_BOUND('',#2762,.T.);
#1949=FACE_OUTER_BOUND('',#2764,.T.);
#1950=FACE_OUTER_BOUND('',#2766,.T.);
#1951=FACE_OUTER_BOUND('',#2767,.T.);
#1952=FACE_OUTER_BOUND('',#2768,.T.);
#1953=FACE_OUTER_BOUND('',#2769,.T.);
#1954=FACE_OUTER_BOUND('',#2771,.T.);
#1955=FACE_OUTER_BOUND('',#2773,.T.);
#1956=FACE_OUTER_BOUND('',#2775,.T.);
#1957=FACE_OUTER_BOUND('',#2777,.T.);
#1958=FACE_OUTER_BOUND('',#2778,.T.);
#1959=FACE_OUTER_BOUND('',#2779,.T.);
#1960=FACE_OUTER_BOUND('',#2781,.T.);
#1961=FACE_OUTER_BOUND('',#2783,.T.);
#1962=FACE_OUTER_BOUND('',#2784,.T.);
#1963=FACE_OUTER_BOUND('',#2785,.T.);
#1964=FACE_OUTER_BOUND('',#2786,.T.);
#1965=FACE_OUTER_BOUND('',#2788,.T.);
#1966=FACE_OUTER_BOUND('',#2789,.T.);
#1967=FACE_OUTER_BOUND('',#2790,.T.);
#1968=FACE_OUTER_BOUND('',#2792,.T.);
#1969=FACE_OUTER_BOUND('',#2793,.T.);
#1970=FACE_OUTER_BOUND('',#2794,.T.);
#1971=FACE_OUTER_BOUND('',#2795,.T.);
#1972=FACE_OUTER_BOUND('',#2796,.T.);
#1973=FACE_OUTER_BOUND('',#2797,.T.);
#1974=FACE_OUTER_BOUND('',#2798,.T.);
#1975=FACE_OUTER_BOUND('',#2799,.T.);
#1976=FACE_OUTER_BOUND('',#2800,.T.);
#1977=FACE_OUTER_BOUND('',#2801,.T.);
#1978=FACE_OUTER_BOUND('',#2802,.T.);
#1979=FACE_OUTER_BOUND('',#2803,.T.);
#1980=FACE_OUTER_BOUND('',#2804,.T.);
#1981=FACE_OUTER_BOUND('',#2805,.T.);
#1982=FACE_OUTER_BOUND('',#2806,.T.);
#1983=FACE_OUTER_BOUND('',#2807,.T.);
#1984=FACE_OUTER_BOUND('',#2808,.T.);
#1985=FACE_OUTER_BOUND('',#2809,.T.);
#1986=FACE_OUTER_BOUND('',#2810,.T.);
#1987=FACE_OUTER_BOUND('',#2811,.T.);
#1988=FACE_OUTER_BOUND('',#2812,.T.);
#1989=FACE_OUTER_BOUND('',#2813,.T.);
#1990=FACE_OUTER_BOUND('',#2814,.T.);
#1991=FACE_OUTER_BOUND('',#2815,.T.);
#1992=FACE_OUTER_BOUND('',#2816,.T.);
#1993=FACE_OUTER_BOUND('',#2817,.T.);
#1994=FACE_OUTER_BOUND('',#2818,.T.);
#1995=FACE_OUTER_BOUND('',#2819,.T.);
#1996=FACE_OUTER_BOUND('',#2820,.T.);
#1997=FACE_OUTER_BOUND('',#2821,.T.);
#1998=FACE_OUTER_BOUND('',#2822,.T.);
#1999=FACE_OUTER_BOUND('',#2823,.T.);
#2000=FACE_OUTER_BOUND('',#2824,.T.);
#2001=FACE_OUTER_BOUND('',#2825,.T.);
#2002=FACE_OUTER_BOUND('',#2826,.T.);
#2003=FACE_OUTER_BOUND('',#2827,.T.);
#2004=FACE_OUTER_BOUND('',#2828,.T.);
#2005=FACE_OUTER_BOUND('',#2829,.T.);
#2006=FACE_OUTER_BOUND('',#2830,.T.);
#2007=FACE_OUTER_BOUND('',#2831,.T.);
#2008=FACE_OUTER_BOUND('',#2832,.T.);
#2009=FACE_OUTER_BOUND('',#2833,.T.);
#2010=FACE_OUTER_BOUND('',#2834,.T.);
#2011=FACE_OUTER_BOUND('',#2835,.T.);
#2012=FACE_OUTER_BOUND('',#2836,.T.);
#2013=FACE_OUTER_BOUND('',#2837,.T.);
#2014=FACE_OUTER_BOUND('',#2838,.T.);
#2015=FACE_OUTER_BOUND('',#2839,.T.);
#2016=FACE_OUTER_BOUND('',#2840,.T.);
#2017=FACE_OUTER_BOUND('',#2841,.T.);
#2018=FACE_OUTER_BOUND('',#2842,.T.);
#2019=FACE_OUTER_BOUND('',#2843,.T.);
#2020=FACE_OUTER_BOUND('',#2844,.T.);
#2021=FACE_OUTER_BOUND('',#2845,.T.);
#2022=FACE_OUTER_BOUND('',#2846,.T.);
#2023=FACE_OUTER_BOUND('',#2847,.T.);
#2024=FACE_OUTER_BOUND('',#2848,.T.);
#2025=FACE_OUTER_BOUND('',#2849,.T.);
#2026=FACE_OUTER_BOUND('',#2850,.T.);
#2027=FACE_OUTER_BOUND('',#2851,.T.);
#2028=FACE_OUTER_BOUND('',#2852,.T.);
#2029=FACE_OUTER_BOUND('',#2853,.T.);
#2030=FACE_OUTER_BOUND('',#2854,.T.);
#2031=FACE_OUTER_BOUND('',#2855,.T.);
#2032=FACE_OUTER_BOUND('',#2856,.T.);
#2033=FACE_OUTER_BOUND('',#2857,.T.);
#2034=FACE_OUTER_BOUND('',#2858,.T.);
#2035=FACE_OUTER_BOUND('',#2859,.T.);
#2036=FACE_OUTER_BOUND('',#2860,.T.);
#2037=FACE_OUTER_BOUND('',#2861,.T.);
#2038=FACE_OUTER_BOUND('',#2862,.T.);
#2039=FACE_OUTER_BOUND('',#2863,.T.);
#2040=FACE_OUTER_BOUND('',#2864,.T.);
#2041=FACE_OUTER_BOUND('',#2865,.T.);
#2042=FACE_OUTER_BOUND('',#2866,.T.);
#2043=FACE_OUTER_BOUND('',#2867,.T.);
#2044=FACE_OUTER_BOUND('',#2868,.T.);
#2045=FACE_OUTER_BOUND('',#2869,.T.);
#2046=FACE_OUTER_BOUND('',#2870,.T.);
#2047=FACE_OUTER_BOUND('',#2871,.T.);
#2048=FACE_OUTER_BOUND('',#2872,.T.);
#2049=FACE_OUTER_BOUND('',#2873,.T.);
#2050=FACE_OUTER_BOUND('',#2874,.T.);
#2051=FACE_OUTER_BOUND('',#2875,.T.);
#2052=FACE_OUTER_BOUND('',#2876,.T.);
#2053=FACE_OUTER_BOUND('',#2877,.T.);
#2054=FACE_OUTER_BOUND('',#2878,.T.);
#2055=FACE_OUTER_BOUND('',#2879,.T.);
#2056=FACE_OUTER_BOUND('',#2880,.T.);
#2057=FACE_OUTER_BOUND('',#2881,.T.);
#2058=FACE_OUTER_BOUND('',#2882,.T.);
#2059=FACE_OUTER_BOUND('',#2883,.T.);
#2060=FACE_OUTER_BOUND('',#2884,.T.);
#2061=FACE_OUTER_BOUND('',#2885,.T.);
#2062=FACE_OUTER_BOUND('',#2886,.T.);
#2063=FACE_OUTER_BOUND('',#2887,.T.);
#2064=FACE_OUTER_BOUND('',#2888,.T.);
#2065=FACE_OUTER_BOUND('',#2889,.T.);
#2066=FACE_OUTER_BOUND('',#2890,.T.);
#2067=FACE_OUTER_BOUND('',#2891,.T.);
#2068=FACE_OUTER_BOUND('',#2892,.T.);
#2069=FACE_OUTER_BOUND('',#2893,.T.);
#2070=FACE_OUTER_BOUND('',#2894,.T.);
#2071=FACE_OUTER_BOUND('',#2895,.T.);
#2072=FACE_OUTER_BOUND('',#2896,.T.);
#2073=FACE_OUTER_BOUND('',#2897,.T.);
#2074=FACE_OUTER_BOUND('',#2898,.T.);
#2075=FACE_OUTER_BOUND('',#2899,.T.);
#2076=FACE_OUTER_BOUND('',#2900,.T.);
#2077=FACE_OUTER_BOUND('',#2901,.T.);
#2078=FACE_OUTER_BOUND('',#2902,.T.);
#2079=FACE_OUTER_BOUND('',#2903,.T.);
#2080=FACE_OUTER_BOUND('',#2904,.T.);
#2081=FACE_OUTER_BOUND('',#2905,.T.);
#2082=FACE_OUTER_BOUND('',#2906,.T.);
#2083=FACE_OUTER_BOUND('',#2907,.T.);
#2084=FACE_OUTER_BOUND('',#2908,.T.);
#2085=FACE_OUTER_BOUND('',#2909,.T.);
#2086=FACE_OUTER_BOUND('',#2910,.T.);
#2087=FACE_OUTER_BOUND('',#2911,.T.);
#2088=FACE_OUTER_BOUND('',#2912,.T.);
#2089=FACE_OUTER_BOUND('',#2913,.T.);
#2090=FACE_OUTER_BOUND('',#2914,.T.);
#2091=FACE_OUTER_BOUND('',#2915,.T.);
#2092=FACE_OUTER_BOUND('',#2916,.T.);
#2093=FACE_OUTER_BOUND('',#2917,.T.);
#2094=FACE_OUTER_BOUND('',#2918,.T.);
#2095=FACE_OUTER_BOUND('',#2919,.T.);
#2096=FACE_OUTER_BOUND('',#2920,.T.);
#2097=FACE_OUTER_BOUND('',#2921,.T.);
#2098=FACE_OUTER_BOUND('',#2922,.T.);
#2099=FACE_OUTER_BOUND('',#2923,.T.);
#2100=FACE_OUTER_BOUND('',#2924,.T.);
#2101=FACE_OUTER_BOUND('',#2925,.T.);
#2102=FACE_OUTER_BOUND('',#2926,.T.);
#2103=FACE_OUTER_BOUND('',#2927,.T.);
#2104=FACE_OUTER_BOUND('',#2928,.T.);
#2105=FACE_OUTER_BOUND('',#2929,.T.);
#2106=FACE_OUTER_BOUND('',#2930,.T.);
#2107=FACE_OUTER_BOUND('',#2931,.T.);
#2108=FACE_OUTER_BOUND('',#2932,.T.);
#2109=FACE_OUTER_BOUND('',#2933,.T.);
#2110=FACE_OUTER_BOUND('',#2934,.T.);
#2111=FACE_OUTER_BOUND('',#2935,.T.);
#2112=FACE_OUTER_BOUND('',#2936,.T.);
#2113=FACE_OUTER_BOUND('',#2937,.T.);
#2114=FACE_OUTER_BOUND('',#2938,.T.);
#2115=FACE_OUTER_BOUND('',#2939,.T.);
#2116=FACE_OUTER_BOUND('',#2940,.T.);
#2117=FACE_OUTER_BOUND('',#2941,.T.);
#2118=FACE_OUTER_BOUND('',#2942,.T.);
#2119=FACE_OUTER_BOUND('',#2943,.T.);
#2120=FACE_OUTER_BOUND('',#2944,.T.);
#2121=FACE_OUTER_BOUND('',#2945,.T.);
#2122=FACE_OUTER_BOUND('',#2946,.T.);
#2123=FACE_OUTER_BOUND('',#2947,.T.);
#2124=FACE_OUTER_BOUND('',#2948,.T.);
#2125=FACE_OUTER_BOUND('',#2949,.T.);
#2126=FACE_OUTER_BOUND('',#2950,.T.);
#2127=FACE_OUTER_BOUND('',#2951,.T.);
#2128=FACE_OUTER_BOUND('',#2953,.T.);
#2129=FACE_OUTER_BOUND('',#2954,.T.);
#2130=FACE_OUTER_BOUND('',#2955,.T.);
#2131=FACE_OUTER_BOUND('',#2956,.T.);
#2132=FACE_OUTER_BOUND('',#2957,.T.);
#2133=FACE_OUTER_BOUND('',#2958,.T.);
#2134=FACE_OUTER_BOUND('',#2959,.T.);
#2135=FACE_OUTER_BOUND('',#2960,.T.);
#2136=FACE_OUTER_BOUND('',#2961,.T.);
#2137=FACE_OUTER_BOUND('',#2962,.T.);
#2138=FACE_OUTER_BOUND('',#2963,.T.);
#2139=FACE_OUTER_BOUND('',#2964,.T.);
#2140=FACE_OUTER_BOUND('',#2965,.T.);
#2141=FACE_OUTER_BOUND('',#2966,.T.);
#2142=FACE_OUTER_BOUND('',#2967,.T.);
#2143=FACE_OUTER_BOUND('',#2968,.T.);
#2144=FACE_OUTER_BOUND('',#2969,.T.);
#2145=FACE_OUTER_BOUND('',#2970,.T.);
#2146=FACE_OUTER_BOUND('',#2971,.T.);
#2147=FACE_OUTER_BOUND('',#2973,.T.);
#2148=FACE_OUTER_BOUND('',#2974,.T.);
#2149=FACE_OUTER_BOUND('',#2975,.T.);
#2150=FACE_OUTER_BOUND('',#2976,.T.);
#2151=EDGE_LOOP('',(#7352,#7353,#7354,#7355));
#2152=EDGE_LOOP('',(#7356,#7357,#7358,#7359));
#2153=EDGE_LOOP('',(#7360,#7361,#7362,#7363));
#2154=EDGE_LOOP('',(#7364,#7365,#7366,#7367));
#2155=EDGE_LOOP('',(#7368,#7369,#7370,#7371));
#2156=EDGE_LOOP('',(#7372,#7373,#7374,#7375));
#2157=EDGE_LOOP('',(#7376,#7377,#7378,#7379));
#2158=EDGE_LOOP('',(#7380,#7381,#7382,#7383));
#2159=EDGE_LOOP('',(#7384,#7385,#7386,#7387));
#2160=EDGE_LOOP('',(#7388));
#2161=EDGE_LOOP('',(#7389));
#2162=EDGE_LOOP('',(#7390));
#2163=EDGE_LOOP('',(#7391));
#2164=EDGE_LOOP('',(#7392,#7393,#7394,#7395));
#2165=EDGE_LOOP('',(#7396));
#2166=EDGE_LOOP('',(#7397));
#2167=EDGE_LOOP('',(#7398));
#2168=EDGE_LOOP('',(#7399));
#2169=EDGE_LOOP('',(#7400,#7401,#7402,#7403));
#2170=EDGE_LOOP('',(#7404,#7405,#7406,#7407));
#2171=EDGE_LOOP('',(#7408,#7409,#7410,#7411));
#2172=EDGE_LOOP('',(#7412,#7413,#7414,#7415));
#2173=EDGE_LOOP('',(#7416,#7417,#7418,#7419));
#2174=EDGE_LOOP('',(#7420,#7421,#7422,#7423));
#2175=EDGE_LOOP('',(#7424,#7425,#7426,#7427));
#2176=EDGE_LOOP('',(#7428));
#2177=EDGE_LOOP('',(#7429));
#2178=EDGE_LOOP('',(#7430,#7431,#7432,#7433));
#2179=EDGE_LOOP('',(#7434));
#2180=EDGE_LOOP('',(#7435));
#2181=EDGE_LOOP('',(#7436,#7437,#7438,#7439));
#2182=EDGE_LOOP('',(#7440));
#2183=EDGE_LOOP('',(#7441));
#2184=EDGE_LOOP('',(#7442,#7443,#7444,#7445));
#2185=EDGE_LOOP('',(#7446));
#2186=EDGE_LOOP('',(#7447));
#2187=EDGE_LOOP('',(#7448,#7449,#7450,#7451));
#2188=EDGE_LOOP('',(#7452,#7453,#7454,#7455));
#2189=EDGE_LOOP('',(#7456,#7457,#7458,#7459));
#2190=EDGE_LOOP('',(#7460,#7461,#7462,#7463));
#2191=EDGE_LOOP('',(#7464,#7465,#7466,#7467));
#2192=EDGE_LOOP('',(#7468));
#2193=EDGE_LOOP('',(#7469,#7470,#7471,#7472));
#2194=EDGE_LOOP('',(#7473));
#2195=EDGE_LOOP('',(#7474,#7475,#7476,#7477));
#2196=EDGE_LOOP('',(#7478));
#2197=EDGE_LOOP('',(#7479));
#2198=EDGE_LOOP('',(#7480,#7481,#7482,#7483));
#2199=EDGE_LOOP('',(#7484,#7485,#7486,#7487));
#2200=EDGE_LOOP('',(#7488));
#2201=EDGE_LOOP('',(#7489));
#2202=EDGE_LOOP('',(#7490,#7491,#7492,#7493));
#2203=EDGE_LOOP('',(#7494,#7495,#7496,#7497));
#2204=EDGE_LOOP('',(#7498));
#2205=EDGE_LOOP('',(#7499));
#2206=EDGE_LOOP('',(#7500));
#2207=EDGE_LOOP('',(#7501));
#2208=EDGE_LOOP('',(#7502));
#2209=EDGE_LOOP('',(#7503));
#2210=EDGE_LOOP('',(#7504));
#2211=EDGE_LOOP('',(#7505));
#2212=EDGE_LOOP('',(#7506));
#2213=EDGE_LOOP('',(#7507));
#2214=EDGE_LOOP('',(#7508));
#2215=EDGE_LOOP('',(#7509));
#2216=EDGE_LOOP('',(#7510,#7511,#7512,#7513));
#2217=EDGE_LOOP('',(#7514,#7515,#7516,#7517));
#2218=EDGE_LOOP('',(#7518));
#2219=EDGE_LOOP('',(#7519));
#2220=EDGE_LOOP('',(#7520));
#2221=EDGE_LOOP('',(#7521));
#2222=EDGE_LOOP('',(#7522));
#2223=EDGE_LOOP('',(#7523));
#2224=EDGE_LOOP('',(#7524));
#2225=EDGE_LOOP('',(#7525));
#2226=EDGE_LOOP('',(#7526));
#2227=EDGE_LOOP('',(#7527));
#2228=EDGE_LOOP('',(#7528));
#2229=EDGE_LOOP('',(#7529));
#2230=EDGE_LOOP('',(#7530,#7531,#7532,#7533));
#2231=EDGE_LOOP('',(#7534,#7535,#7536,#7537));
#2232=EDGE_LOOP('',(#7538,#7539,#7540,#7541));
#2233=EDGE_LOOP('',(#7542));
#2234=EDGE_LOOP('',(#7543));
#2235=EDGE_LOOP('',(#7544,#7545,#7546,#7547));
#2236=EDGE_LOOP('',(#7548,#7549,#7550,#7551));
#2237=EDGE_LOOP('',(#7552,#7553,#7554,#7555));
#2238=EDGE_LOOP('',(#7556,#7557,#7558,#7559));
#2239=EDGE_LOOP('',(#7560,#7561,#7562,#7563));
#2240=EDGE_LOOP('',(#7564,#7565,#7566,#7567));
#2241=EDGE_LOOP('',(#7568,#7569,#7570,#7571));
#2242=EDGE_LOOP('',(#7572));
#2243=EDGE_LOOP('',(#7573));
#2244=EDGE_LOOP('',(#7574,#7575,#7576,#7577));
#2245=EDGE_LOOP('',(#7578));
#2246=EDGE_LOOP('',(#7579));
#2247=EDGE_LOOP('',(#7580,#7581,#7582,#7583));
#2248=EDGE_LOOP('',(#7584));
#2249=EDGE_LOOP('',(#7585));
#2250=EDGE_LOOP('',(#7586,#7587,#7588,#7589));
#2251=EDGE_LOOP('',(#7590));
#2252=EDGE_LOOP('',(#7591));
#2253=EDGE_LOOP('',(#7592,#7593,#7594,#7595));
#2254=EDGE_LOOP('',(#7596,#7597,#7598,#7599));
#2255=EDGE_LOOP('',(#7600,#7601,#7602,#7603));
#2256=EDGE_LOOP('',(#7604,#7605,#7606,#7607));
#2257=EDGE_LOOP('',(#7608,#7609,#7610,#7611));
#2258=EDGE_LOOP('',(#7612));
#2259=EDGE_LOOP('',(#7613,#7614,#7615,#7616));
#2260=EDGE_LOOP('',(#7617));
#2261=EDGE_LOOP('',(#7618,#7619,#7620,#7621));
#2262=EDGE_LOOP('',(#7622));
#2263=EDGE_LOOP('',(#7623));
#2264=EDGE_LOOP('',(#7624,#7625,#7626,#7627));
#2265=EDGE_LOOP('',(#7628,#7629,#7630,#7631));
#2266=EDGE_LOOP('',(#7632));
#2267=EDGE_LOOP('',(#7633));
#2268=EDGE_LOOP('',(#7634,#7635,#7636,#7637));
#2269=EDGE_LOOP('',(#7638,#7639,#7640,#7641));
#2270=EDGE_LOOP('',(#7642));
#2271=EDGE_LOOP('',(#7643));
#2272=EDGE_LOOP('',(#7644));
#2273=EDGE_LOOP('',(#7645));
#2274=EDGE_LOOP('',(#7646));
#2275=EDGE_LOOP('',(#7647));
#2276=EDGE_LOOP('',(#7648));
#2277=EDGE_LOOP('',(#7649));
#2278=EDGE_LOOP('',(#7650));
#2279=EDGE_LOOP('',(#7651));
#2280=EDGE_LOOP('',(#7652));
#2281=EDGE_LOOP('',(#7653));
#2282=EDGE_LOOP('',(#7654,#7655,#7656,#7657));
#2283=EDGE_LOOP('',(#7658,#7659,#7660,#7661));
#2284=EDGE_LOOP('',(#7662));
#2285=EDGE_LOOP('',(#7663));
#2286=EDGE_LOOP('',(#7664));
#2287=EDGE_LOOP('',(#7665));
#2288=EDGE_LOOP('',(#7666));
#2289=EDGE_LOOP('',(#7667));
#2290=EDGE_LOOP('',(#7668));
#2291=EDGE_LOOP('',(#7669));
#2292=EDGE_LOOP('',(#7670));
#2293=EDGE_LOOP('',(#7671));
#2294=EDGE_LOOP('',(#7672));
#2295=EDGE_LOOP('',(#7673));
#2296=EDGE_LOOP('',(#7674,#7675,#7676,#7677));
#2297=EDGE_LOOP('',(#7678,#7679,#7680,#7681));
#2298=EDGE_LOOP('',(#7682,#7683,#7684,#7685));
#2299=EDGE_LOOP('',(#7686));
#2300=EDGE_LOOP('',(#7687));
#2301=EDGE_LOOP('',(#7688,#7689,#7690,#7691));
#2302=EDGE_LOOP('',(#7692,#7693,#7694,#7695));
#2303=EDGE_LOOP('',(#7696));
#2304=EDGE_LOOP('',(#7697));
#2305=EDGE_LOOP('',(#7698));
#2306=EDGE_LOOP('',(#7699));
#2307=EDGE_LOOP('',(#7700,#7701,#7702,#7703));
#2308=EDGE_LOOP('',(#7704,#7705,#7706,#7707));
#2309=EDGE_LOOP('',(#7708));
#2310=EDGE_LOOP('',(#7709));
#2311=EDGE_LOOP('',(#7710));
#2312=EDGE_LOOP('',(#7711));
#2313=EDGE_LOOP('',(#7712,#7713,#7714,#7715));
#2314=EDGE_LOOP('',(#7716,#7717,#7718,#7719));
#2315=EDGE_LOOP('',(#7720));
#2316=EDGE_LOOP('',(#7721));
#2317=EDGE_LOOP('',(#7722));
#2318=EDGE_LOOP('',(#7723));
#2319=EDGE_LOOP('',(#7724,#7725,#7726,#7727));
#2320=EDGE_LOOP('',(#7728,#7729,#7730,#7731));
#2321=EDGE_LOOP('',(#7732));
#2322=EDGE_LOOP('',(#7733));
#2323=EDGE_LOOP('',(#7734));
#2324=EDGE_LOOP('',(#7735));
#2325=EDGE_LOOP('',(#7736,#7737,#7738,#7739));
#2326=EDGE_LOOP('',(#7740,#7741,#7742,#7743));
#2327=EDGE_LOOP('',(#7744,#7745,#7746,#7747));
#2328=EDGE_LOOP('',(#7748,#7749,#7750,#7751));
#2329=EDGE_LOOP('',(#7752));
#2330=EDGE_LOOP('',(#7753));
#2331=EDGE_LOOP('',(#7754,#7755,#7756,#7757));
#2332=EDGE_LOOP('',(#7758,#7759,#7760,#7761));
#2333=EDGE_LOOP('',(#7762));
#2334=EDGE_LOOP('',(#7763));
#2335=EDGE_LOOP('',(#7764));
#2336=EDGE_LOOP('',(#7765));
#2337=EDGE_LOOP('',(#7766));
#2338=EDGE_LOOP('',(#7767));
#2339=EDGE_LOOP('',(#7768));
#2340=EDGE_LOOP('',(#7769));
#2341=EDGE_LOOP('',(#7770));
#2342=EDGE_LOOP('',(#7771));
#2343=EDGE_LOOP('',(#7772,#7773,#7774,#7775));
#2344=EDGE_LOOP('',(#7776,#7777,#7778,#7779));
#2345=EDGE_LOOP('',(#7780,#7781,#7782,#7783));
#2346=EDGE_LOOP('',(#7784,#7785,#7786,#7787));
#2347=EDGE_LOOP('',(#7788));
#2348=EDGE_LOOP('',(#7789));
#2349=EDGE_LOOP('',(#7790,#7791,#7792,#7793));
#2350=EDGE_LOOP('',(#7794,#7795,#7796,#7797));
#2351=EDGE_LOOP('',(#7798));
#2352=EDGE_LOOP('',(#7799));
#2353=EDGE_LOOP('',(#7800));
#2354=EDGE_LOOP('',(#7801));
#2355=EDGE_LOOP('',(#7802));
#2356=EDGE_LOOP('',(#7803));
#2357=EDGE_LOOP('',(#7804));
#2358=EDGE_LOOP('',(#7805));
#2359=EDGE_LOOP('',(#7806));
#2360=EDGE_LOOP('',(#7807));
#2361=EDGE_LOOP('',(#7808,#7809,#7810,#7811));
#2362=EDGE_LOOP('',(#7812,#7813,#7814,#7815));
#2363=EDGE_LOOP('',(#7816,#7817,#7818,#7819));
#2364=EDGE_LOOP('',(#7820,#7821,#7822,#7823));
#2365=EDGE_LOOP('',(#7824));
#2366=EDGE_LOOP('',(#7825));
#2367=EDGE_LOOP('',(#7826,#7827,#7828,#7829));
#2368=EDGE_LOOP('',(#7830,#7831,#7832,#7833));
#2369=EDGE_LOOP('',(#7834));
#2370=EDGE_LOOP('',(#7835));
#2371=EDGE_LOOP('',(#7836));
#2372=EDGE_LOOP('',(#7837));
#2373=EDGE_LOOP('',(#7838));
#2374=EDGE_LOOP('',(#7839));
#2375=EDGE_LOOP('',(#7840));
#2376=EDGE_LOOP('',(#7841));
#2377=EDGE_LOOP('',(#7842));
#2378=EDGE_LOOP('',(#7843));
#2379=EDGE_LOOP('',(#7844,#7845,#7846,#7847));
#2380=EDGE_LOOP('',(#7848,#7849,#7850,#7851));
#2381=EDGE_LOOP('',(#7852,#7853,#7854,#7855));
#2382=EDGE_LOOP('',(#7856,#7857,#7858,#7859));
#2383=EDGE_LOOP('',(#7860));
#2384=EDGE_LOOP('',(#7861));
#2385=EDGE_LOOP('',(#7862,#7863,#7864,#7865));
#2386=EDGE_LOOP('',(#7866,#7867,#7868,#7869));
#2387=EDGE_LOOP('',(#7870));
#2388=EDGE_LOOP('',(#7871));
#2389=EDGE_LOOP('',(#7872));
#2390=EDGE_LOOP('',(#7873));
#2391=EDGE_LOOP('',(#7874));
#2392=EDGE_LOOP('',(#7875));
#2393=EDGE_LOOP('',(#7876));
#2394=EDGE_LOOP('',(#7877));
#2395=EDGE_LOOP('',(#7878));
#2396=EDGE_LOOP('',(#7879));
#2397=EDGE_LOOP('',(#7880));
#2398=EDGE_LOOP('',(#7881,#7882,#7883,#7884));
#2399=EDGE_LOOP('',(#7885,#7886,#7887,#7888));
#2400=EDGE_LOOP('',(#7889,#7890,#7891,#7892));
#2401=EDGE_LOOP('',(#7893));
#2402=EDGE_LOOP('',(#7894));
#2403=EDGE_LOOP('',(#7895,#7896,#7897,#7898));
#2404=EDGE_LOOP('',(#7899,#7900,#7901,#7902));
#2405=EDGE_LOOP('',(#7903,#7904,#7905,#7906));
#2406=EDGE_LOOP('',(#7907));
#2407=EDGE_LOOP('',(#7908,#7909,#7910,#7911));
#2408=EDGE_LOOP('',(#7912,#7913,#7914,#7915));
#2409=EDGE_LOOP('',(#7916,#7917,#7918,#7919));
#2410=EDGE_LOOP('',(#7920,#7921,#7922,#7923));
#2411=EDGE_LOOP('',(#7924,#7925,#7926,#7927));
#2412=EDGE_LOOP('',(#7928,#7929,#7930,#7931));
#2413=EDGE_LOOP('',(#7932,#7933,#7934,#7935,#7936,#7937));
#2414=EDGE_LOOP('',(#7938,#7939,#7940,#7941,#7942,#7943));
#2415=EDGE_LOOP('',(#7944));
#2416=EDGE_LOOP('',(#7945,#7946,#7947,#7948));
#2417=EDGE_LOOP('',(#7949,#7950,#7951,#7952));
#2418=EDGE_LOOP('',(#7953,#7954,#7955,#7956));
#2419=EDGE_LOOP('',(#7957));
#2420=EDGE_LOOP('',(#7958));
#2421=EDGE_LOOP('',(#7959,#7960,#7961,#7962));
#2422=EDGE_LOOP('',(#7963,#7964,#7965,#7966));
#2423=EDGE_LOOP('',(#7967,#7968,#7969,#7970));
#2424=EDGE_LOOP('',(#7971));
#2425=EDGE_LOOP('',(#7972,#7973,#7974,#7975));
#2426=EDGE_LOOP('',(#7976,#7977,#7978,#7979));
#2427=EDGE_LOOP('',(#7980,#7981,#7982,#7983));
#2428=EDGE_LOOP('',(#7984,#7985,#7986,#7987));
#2429=EDGE_LOOP('',(#7988,#7989,#7990,#7991));
#2430=EDGE_LOOP('',(#7992,#7993,#7994,#7995));
#2431=EDGE_LOOP('',(#7996,#7997,#7998,#7999,#8000,#8001));
#2432=EDGE_LOOP('',(#8002,#8003,#8004,#8005,#8006,#8007));
#2433=EDGE_LOOP('',(#8008,#8009,#8010,#8011,#8012,#8013));
#2434=EDGE_LOOP('',(#8014,#8015,#8016,#8017,#8018));
#2435=EDGE_LOOP('',(#8019,#8020,#8021,#8022));
#2436=EDGE_LOOP('',(#8023,#8024,#8025,#8026));
#2437=EDGE_LOOP('',(#8027));
#2438=EDGE_LOOP('',(#8028));
#2439=EDGE_LOOP('',(#8029,#8030,#8031,#8032,#8033));
#2440=EDGE_LOOP('',(#8034));
#2441=EDGE_LOOP('',(#8035));
#2442=EDGE_LOOP('',(#8036,#8037,#8038,#8039));
#2443=EDGE_LOOP('',(#8040,#8041,#8042,#8043,#8044,#8045));
#2444=EDGE_LOOP('',(#8046,#8047,#8048,#8049,#8050));
#2445=EDGE_LOOP('',(#8051));
#2446=EDGE_LOOP('',(#8052));
#2447=EDGE_LOOP('',(#8053,#8054,#8055,#8056));
#2448=EDGE_LOOP('',(#8057,#8058,#8059,#8060));
#2449=EDGE_LOOP('',(#8061,#8062,#8063,#8064));
#2450=EDGE_LOOP('',(#8065));
#2451=EDGE_LOOP('',(#8066));
#2452=EDGE_LOOP('',(#8067,#8068,#8069,#8070,#8071));
#2453=EDGE_LOOP('',(#8072,#8073));
#2454=EDGE_LOOP('',(#8074,#8075));
#2455=EDGE_LOOP('',(#8076,#8077));
#2456=EDGE_LOOP('',(#8078,#8079));
#2457=EDGE_LOOP('',(#8080,#8081));
#2458=EDGE_LOOP('',(#8082,#8083));
#2459=EDGE_LOOP('',(#8084,#8085));
#2460=EDGE_LOOP('',(#8086,#8087,#8088,#8089));
#2461=EDGE_LOOP('',(#8090,#8091,#8092,#8093,#8094,#8095,#8096,#8097,#8098,
#8099,#8100,#8101,#8102,#8103,#8104,#8105,#8106,#8107));
#2462=EDGE_LOOP('',(#8108,#8109,#8110,#8111));
#2463=EDGE_LOOP('',(#8112,#8113,#8114,#8115));
#2464=EDGE_LOOP('',(#8116,#8117,#8118,#8119));
#2465=EDGE_LOOP('',(#8120,#8121,#8122,#8123));
#2466=EDGE_LOOP('',(#8124,#8125,#8126,#8127,#8128,#8129));
#2467=EDGE_LOOP('',(#8130,#8131,#8132,#8133));
#2468=EDGE_LOOP('',(#8134,#8135,#8136,#8137));
#2469=EDGE_LOOP('',(#8138,#8139,#8140,#8141));
#2470=EDGE_LOOP('',(#8142,#8143,#8144,#8145));
#2471=EDGE_LOOP('',(#8146,#8147,#8148,#8149));
#2472=EDGE_LOOP('',(#8150,#8151,#8152,#8153,#8154,#8155,#8156,#8157,#8158,
#8159,#8160,#8161,#8162,#8163,#8164,#8165,#8166,#8167));
#2473=EDGE_LOOP('',(#8168,#8169,#8170,#8171));
#2474=EDGE_LOOP('',(#8172,#8173,#8174,#8175));
#2475=EDGE_LOOP('',(#8176));
#2476=EDGE_LOOP('',(#8177));
#2477=EDGE_LOOP('',(#8178,#8179,#8180,#8181));
#2478=EDGE_LOOP('',(#8182));
#2479=EDGE_LOOP('',(#8183));
#2480=EDGE_LOOP('',(#8184,#8185,#8186,#8187));
#2481=EDGE_LOOP('',(#8188));
#2482=EDGE_LOOP('',(#8189));
#2483=EDGE_LOOP('',(#8190,#8191,#8192,#8193));
#2484=EDGE_LOOP('',(#8194));
#2485=EDGE_LOOP('',(#8195));
#2486=EDGE_LOOP('',(#8196,#8197,#8198,#8199));
#2487=EDGE_LOOP('',(#8200));
#2488=EDGE_LOOP('',(#8201));
#2489=EDGE_LOOP('',(#8202,#8203,#8204,#8205));
#2490=EDGE_LOOP('',(#8206,#8207,#8208,#8209,#8210,#8211));
#2491=EDGE_LOOP('',(#8212,#8213,#8214,#8215,#8216));
#2492=EDGE_LOOP('',(#8217,#8218,#8219,#8220));
#2493=EDGE_LOOP('',(#8221,#8222,#8223,#8224));
#2494=EDGE_LOOP('',(#8225));
#2495=EDGE_LOOP('',(#8226));
#2496=EDGE_LOOP('',(#8227,#8228,#8229,#8230,#8231));
#2497=EDGE_LOOP('',(#8232));
#2498=EDGE_LOOP('',(#8233));
#2499=EDGE_LOOP('',(#8234,#8235,#8236,#8237));
#2500=EDGE_LOOP('',(#8238,#8239,#8240,#8241,#8242,#8243));
#2501=EDGE_LOOP('',(#8244,#8245,#8246,#8247,#8248));
#2502=EDGE_LOOP('',(#8249));
#2503=EDGE_LOOP('',(#8250));
#2504=EDGE_LOOP('',(#8251,#8252,#8253,#8254));
#2505=EDGE_LOOP('',(#8255,#8256,#8257,#8258));
#2506=EDGE_LOOP('',(#8259,#8260,#8261,#8262));
#2507=EDGE_LOOP('',(#8263));
#2508=EDGE_LOOP('',(#8264));
#2509=EDGE_LOOP('',(#8265,#8266,#8267,#8268,#8269));
#2510=EDGE_LOOP('',(#8270,#8271));
#2511=EDGE_LOOP('',(#8272,#8273));
#2512=EDGE_LOOP('',(#8274,#8275));
#2513=EDGE_LOOP('',(#8276,#8277));
#2514=EDGE_LOOP('',(#8278,#8279));
#2515=EDGE_LOOP('',(#8280,#8281));
#2516=EDGE_LOOP('',(#8282,#8283));
#2517=EDGE_LOOP('',(#8284,#8285));
#2518=EDGE_LOOP('',(#8286,#8287,#8288,#8289));
#2519=EDGE_LOOP('',(#8290,#8291,#8292,#8293,#8294,#8295,#8296,#8297,#8298,
#8299,#8300,#8301,#8302,#8303,#8304,#8305,#8306,#8307,#8308,#8309));
#2520=EDGE_LOOP('',(#8310,#8311,#8312,#8313));
#2521=EDGE_LOOP('',(#8314,#8315,#8316,#8317));
#2522=EDGE_LOOP('',(#8318,#8319,#8320,#8321));
#2523=EDGE_LOOP('',(#8322,#8323,#8324,#8325));
#2524=EDGE_LOOP('',(#8326,#8327,#8328,#8329));
#2525=EDGE_LOOP('',(#8330,#8331,#8332,#8333,#8334,#8335));
#2526=EDGE_LOOP('',(#8336,#8337,#8338,#8339));
#2527=EDGE_LOOP('',(#8340,#8341,#8342,#8343));
#2528=EDGE_LOOP('',(#8344,#8345,#8346,#8347));
#2529=EDGE_LOOP('',(#8348,#8349,#8350,#8351));
#2530=EDGE_LOOP('',(#8352,#8353,#8354,#8355));
#2531=EDGE_LOOP('',(#8356,#8357,#8358,#8359));
#2532=EDGE_LOOP('',(#8360,#8361,#8362,#8363,#8364,#8365,#8366,#8367,#8368,
#8369,#8370,#8371,#8372,#8373,#8374,#8375,#8376,#8377,#8378,#8379));
#2533=EDGE_LOOP('',(#8380,#8381,#8382,#8383));
#2534=EDGE_LOOP('',(#8384,#8385,#8386,#8387));
#2535=EDGE_LOOP('',(#8388));
#2536=EDGE_LOOP('',(#8389));
#2537=EDGE_LOOP('',(#8390,#8391,#8392,#8393));
#2538=EDGE_LOOP('',(#8394));
#2539=EDGE_LOOP('',(#8395));
#2540=EDGE_LOOP('',(#8396,#8397,#8398,#8399));
#2541=EDGE_LOOP('',(#8400));
#2542=EDGE_LOOP('',(#8401));
#2543=EDGE_LOOP('',(#8402,#8403,#8404,#8405));
#2544=EDGE_LOOP('',(#8406));
#2545=EDGE_LOOP('',(#8407));
#2546=EDGE_LOOP('',(#8408,#8409,#8410,#8411));
#2547=EDGE_LOOP('',(#8412));
#2548=EDGE_LOOP('',(#8413));
#2549=EDGE_LOOP('',(#8414,#8415,#8416,#8417));
#2550=EDGE_LOOP('',(#8418));
#2551=EDGE_LOOP('',(#8419,#8420,#8421,#8422));
#2552=EDGE_LOOP('',(#8423,#8424,#8425,#8426));
#2553=EDGE_LOOP('',(#8427,#8428,#8429,#8430));
#2554=EDGE_LOOP('',(#8431));
#2555=EDGE_LOOP('',(#8432));
#2556=EDGE_LOOP('',(#8433,#8434,#8435,#8436));
#2557=EDGE_LOOP('',(#8437,#8438,#8439,#8440));
#2558=EDGE_LOOP('',(#8441,#8442,#8443,#8444));
#2559=EDGE_LOOP('',(#8445));
#2560=EDGE_LOOP('',(#8446,#8447,#8448,#8449));
#2561=EDGE_LOOP('',(#8450,#8451,#8452,#8453));
#2562=EDGE_LOOP('',(#8454,#8455,#8456,#8457));
#2563=EDGE_LOOP('',(#8458,#8459,#8460,#8461));
#2564=EDGE_LOOP('',(#8462,#8463,#8464,#8465));
#2565=EDGE_LOOP('',(#8466,#8467,#8468,#8469));
#2566=EDGE_LOOP('',(#8470,#8471,#8472,#8473,#8474,#8475));
#2567=EDGE_LOOP('',(#8476,#8477,#8478,#8479,#8480,#8481));
#2568=EDGE_LOOP('',(#8482,#8483,#8484,#8485));
#2569=EDGE_LOOP('',(#8486,#8487,#8488,#8489));
#2570=EDGE_LOOP('',(#8490,#8491,#8492,#8493));
#2571=EDGE_LOOP('',(#8494,#8495,#8496,#8497));
#2572=EDGE_LOOP('',(#8498,#8499,#8500,#8501));
#2573=EDGE_LOOP('',(#8502,#8503,#8504,#8505));
#2574=EDGE_LOOP('',(#8506,#8507,#8508,#8509));
#2575=EDGE_LOOP('',(#8510));
#2576=EDGE_LOOP('',(#8511));
#2577=EDGE_LOOP('',(#8512,#8513,#8514,#8515));
#2578=EDGE_LOOP('',(#8516,#8517,#8518,#8519));
#2579=EDGE_LOOP('',(#8520));
#2580=EDGE_LOOP('',(#8521));
#2581=EDGE_LOOP('',(#8522));
#2582=EDGE_LOOP('',(#8523));
#2583=EDGE_LOOP('',(#8524,#8525,#8526,#8527));
#2584=EDGE_LOOP('',(#8528,#8529,#8530,#8531));
#2585=EDGE_LOOP('',(#8532));
#2586=EDGE_LOOP('',(#8533));
#2587=EDGE_LOOP('',(#8534));
#2588=EDGE_LOOP('',(#8535));
#2589=EDGE_LOOP('',(#8536,#8537));
#2590=EDGE_LOOP('',(#8538,#8539,#8540,#8541,#8542,#8543,#8544,#8545,#8546));
#2591=EDGE_LOOP('',(#8547,#8548,#8549));
#2592=EDGE_LOOP('',(#8550,#8551,#8552,#8553));
#2593=EDGE_LOOP('',(#8554,#8555,#8556,#8557));
#2594=EDGE_LOOP('',(#8558,#8559,#8560,#8561));
#2595=EDGE_LOOP('',(#8562,#8563));
#2596=EDGE_LOOP('',(#8564));
#2597=EDGE_LOOP('',(#8565));
#2598=EDGE_LOOP('',(#8566));
#2599=EDGE_LOOP('',(#8567));
#2600=EDGE_LOOP('',(#8568,#8569,#8570,#8571));
#2601=EDGE_LOOP('',(#8572,#8573,#8574,#8575));
#2602=EDGE_LOOP('',(#8576));
#2603=EDGE_LOOP('',(#8577));
#2604=EDGE_LOOP('',(#8578));
#2605=EDGE_LOOP('',(#8579));
#2606=EDGE_LOOP('',(#8580,#8581));
#2607=EDGE_LOOP('',(#8582,#8583,#8584,#8585,#8586,#8587,#8588,#8589,#8590));
#2608=EDGE_LOOP('',(#8591,#8592,#8593));
#2609=EDGE_LOOP('',(#8594,#8595,#8596,#8597));
#2610=EDGE_LOOP('',(#8598,#8599,#8600,#8601));
#2611=EDGE_LOOP('',(#8602,#8603,#8604,#8605));
#2612=EDGE_LOOP('',(#8606,#8607));
#2613=EDGE_LOOP('',(#8608));
#2614=EDGE_LOOP('',(#8609));
#2615=EDGE_LOOP('',(#8610));
#2616=EDGE_LOOP('',(#8611));
#2617=EDGE_LOOP('',(#8612,#8613,#8614,#8615));
#2618=EDGE_LOOP('',(#8616,#8617,#8618,#8619));
#2619=EDGE_LOOP('',(#8620));
#2620=EDGE_LOOP('',(#8621));
#2621=EDGE_LOOP('',(#8622));
#2622=EDGE_LOOP('',(#8623));
#2623=EDGE_LOOP('',(#8624,#8625,#8626,#8627));
#2624=EDGE_LOOP('',(#8628,#8629,#8630,#8631));
#2625=EDGE_LOOP('',(#8632,#8633,#8634,#8635));
#2626=EDGE_LOOP('',(#8636,#8637,#8638,#8639,#8640,#8641,#8642,#8643,#8644,
#8645,#8646,#8647,#8648,#8649,#8650,#8651,#8652,#8653,#8654,#8655,#8656,
#8657,#8658,#8659,#8660,#8661,#8662,#8663,#8664,#8665,#8666,#8667,#8668,
#8669,#8670,#8671,#8672,#8673,#8674,#8675,#8676,#8677,#8678,#8679,#8680,
#8681,#8682,#8683,#8684,#8685,#8686,#8687,#8688,#8689,#8690,#8691,#8692,
#8693,#8694,#8695,#8696,#8697,#8698,#8699,#8700,#8701,#8702,#8703,#8704,
#8705,#8706,#8707,#8708,#8709,#8710,#8711,#8712,#8713,#8714,#8715));
#2627=EDGE_LOOP('',(#8716,#8717,#8718,#8719));
#2628=EDGE_LOOP('',(#8720,#8721,#8722,#8723));
#2629=EDGE_LOOP('',(#8724,#8725,#8726,#8727));
#2630=EDGE_LOOP('',(#8728));
#2631=EDGE_LOOP('',(#8729,#8730,#8731,#8732));
#2632=EDGE_LOOP('',(#8733,#8734,#8735,#8736));
#2633=EDGE_LOOP('',(#8737,#8738,#8739,#8740));
#2634=EDGE_LOOP('',(#8741,#8742,#8743,#8744));
#2635=EDGE_LOOP('',(#8745,#8746,#8747,#8748));
#2636=EDGE_LOOP('',(#8749,#8750,#8751,#8752));
#2637=EDGE_LOOP('',(#8753,#8754,#8755,#8756));
#2638=EDGE_LOOP('',(#8757,#8758,#8759,#8760));
#2639=EDGE_LOOP('',(#8761,#8762,#8763,#8764));
#2640=EDGE_LOOP('',(#8765,#8766,#8767,#8768));
#2641=EDGE_LOOP('',(#8769,#8770,#8771,#8772));
#2642=EDGE_LOOP('',(#8773,#8774,#8775,#8776));
#2643=EDGE_LOOP('',(#8777,#8778,#8779,#8780));
#2644=EDGE_LOOP('',(#8781,#8782,#8783,#8784));
#2645=EDGE_LOOP('',(#8785,#8786,#8787,#8788));
#2646=EDGE_LOOP('',(#8789,#8790,#8791,#8792));
#2647=EDGE_LOOP('',(#8793,#8794,#8795,#8796));
#2648=EDGE_LOOP('',(#8797,#8798,#8799,#8800));
#2649=EDGE_LOOP('',(#8801,#8802,#8803,#8804));
#2650=EDGE_LOOP('',(#8805,#8806,#8807,#8808));
#2651=EDGE_LOOP('',(#8809,#8810,#8811,#8812));
#2652=EDGE_LOOP('',(#8813,#8814,#8815,#8816));
#2653=EDGE_LOOP('',(#8817,#8818,#8819,#8820));
#2654=EDGE_LOOP('',(#8821,#8822,#8823,#8824));
#2655=EDGE_LOOP('',(#8825,#8826,#8827,#8828));
#2656=EDGE_LOOP('',(#8829,#8830,#8831,#8832));
#2657=EDGE_LOOP('',(#8833,#8834,#8835,#8836));
#2658=EDGE_LOOP('',(#8837,#8838,#8839,#8840));
#2659=EDGE_LOOP('',(#8841,#8842,#8843,#8844));
#2660=EDGE_LOOP('',(#8845,#8846,#8847,#8848));
#2661=EDGE_LOOP('',(#8849,#8850,#8851,#8852));
#2662=EDGE_LOOP('',(#8853,#8854,#8855,#8856));
#2663=EDGE_LOOP('',(#8857,#8858,#8859,#8860));
#2664=EDGE_LOOP('',(#8861,#8862,#8863,#8864));
#2665=EDGE_LOOP('',(#8865,#8866,#8867,#8868));
#2666=EDGE_LOOP('',(#8869,#8870,#8871,#8872));
#2667=EDGE_LOOP('',(#8873,#8874,#8875,#8876));
#2668=EDGE_LOOP('',(#8877,#8878,#8879,#8880));
#2669=EDGE_LOOP('',(#8881,#8882,#8883,#8884));
#2670=EDGE_LOOP('',(#8885,#8886,#8887,#8888));
#2671=EDGE_LOOP('',(#8889,#8890,#8891,#8892));
#2672=EDGE_LOOP('',(#8893,#8894,#8895,#8896));
#2673=EDGE_LOOP('',(#8897,#8898,#8899,#8900));
#2674=EDGE_LOOP('',(#8901,#8902,#8903,#8904));
#2675=EDGE_LOOP('',(#8905,#8906,#8907,#8908));
#2676=EDGE_LOOP('',(#8909,#8910,#8911,#8912));
#2677=EDGE_LOOP('',(#8913,#8914,#8915,#8916));
#2678=EDGE_LOOP('',(#8917,#8918,#8919,#8920));
#2679=EDGE_LOOP('',(#8921,#8922,#8923,#8924));
#2680=EDGE_LOOP('',(#8925,#8926,#8927,#8928));
#2681=EDGE_LOOP('',(#8929,#8930,#8931,#8932));
#2682=EDGE_LOOP('',(#8933,#8934,#8935,#8936));
#2683=EDGE_LOOP('',(#8937,#8938,#8939,#8940));
#2684=EDGE_LOOP('',(#8941,#8942,#8943,#8944));
#2685=EDGE_LOOP('',(#8945,#8946,#8947,#8948));
#2686=EDGE_LOOP('',(#8949,#8950,#8951,#8952));
#2687=EDGE_LOOP('',(#8953,#8954,#8955,#8956));
#2688=EDGE_LOOP('',(#8957,#8958,#8959,#8960));
#2689=EDGE_LOOP('',(#8961,#8962,#8963,#8964));
#2690=EDGE_LOOP('',(#8965,#8966,#8967,#8968));
#2691=EDGE_LOOP('',(#8969,#8970,#8971,#8972));
#2692=EDGE_LOOP('',(#8973,#8974,#8975,#8976));
#2693=EDGE_LOOP('',(#8977,#8978,#8979,#8980));
#2694=EDGE_LOOP('',(#8981,#8982,#8983,#8984));
#2695=EDGE_LOOP('',(#8985,#8986,#8987,#8988));
#2696=EDGE_LOOP('',(#8989,#8990,#8991,#8992));
#2697=EDGE_LOOP('',(#8993,#8994,#8995,#8996));
#2698=EDGE_LOOP('',(#8997,#8998,#8999,#9000));
#2699=EDGE_LOOP('',(#9001,#9002,#9003,#9004));
#2700=EDGE_LOOP('',(#9005,#9006,#9007,#9008));
#2701=EDGE_LOOP('',(#9009,#9010,#9011,#9012));
#2702=EDGE_LOOP('',(#9013,#9014,#9015,#9016));
#2703=EDGE_LOOP('',(#9017,#9018,#9019,#9020));
#2704=EDGE_LOOP('',(#9021,#9022,#9023,#9024));
#2705=EDGE_LOOP('',(#9025,#9026,#9027,#9028));
#2706=EDGE_LOOP('',(#9029,#9030,#9031,#9032));
#2707=EDGE_LOOP('',(#9033,#9034,#9035,#9036));
#2708=EDGE_LOOP('',(#9037,#9038,#9039,#9040));
#2709=EDGE_LOOP('',(#9041,#9042,#9043,#9044));
#2710=EDGE_LOOP('',(#9045,#9046,#9047,#9048));
#2711=EDGE_LOOP('',(#9049,#9050,#9051,#9052,#9053,#9054,#9055,#9056,#9057,
#9058,#9059,#9060,#9061,#9062,#9063,#9064,#9065,#9066,#9067,#9068,#9069,
#9070,#9071,#9072,#9073,#9074,#9075,#9076,#9077,#9078,#9079,#9080,#9081,
#9082,#9083,#9084,#9085,#9086,#9087,#9088,#9089,#9090,#9091,#9092,#9093,
#9094,#9095,#9096,#9097,#9098,#9099,#9100,#9101,#9102,#9103,#9104,#9105,
#9106,#9107,#9108,#9109,#9110,#9111,#9112,#9113,#9114,#9115,#9116,#9117,
#9118,#9119,#9120,#9121,#9122,#9123,#9124,#9125,#9126,#9127,#9128));
#2712=EDGE_LOOP('',(#9129));
#2713=EDGE_LOOP('',(#9130,#9131,#9132,#9133));
#2714=EDGE_LOOP('',(#9134,#9135,#9136,#9137));
#2715=EDGE_LOOP('',(#9138,#9139,#9140,#9141));
#2716=EDGE_LOOP('',(#9142,#9143,#9144,#9145));
#2717=EDGE_LOOP('',(#9146,#9147,#9148,#9149));
#2718=EDGE_LOOP('',(#9150,#9151,#9152,#9153));
#2719=EDGE_LOOP('',(#9154,#9155,#9156,#9157));
#2720=EDGE_LOOP('',(#9158,#9159,#9160,#9161));
#2721=EDGE_LOOP('',(#9162,#9163,#9164,#9165));
#2722=EDGE_LOOP('',(#9166,#9167,#9168,#9169));
#2723=EDGE_LOOP('',(#9170,#9171,#9172,#9173));
#2724=EDGE_LOOP('',(#9174,#9175,#9176,#9177));
#2725=EDGE_LOOP('',(#9178,#9179,#9180,#9181));
#2726=EDGE_LOOP('',(#9182,#9183,#9184,#9185));
#2727=EDGE_LOOP('',(#9186,#9187,#9188,#9189));
#2728=EDGE_LOOP('',(#9190,#9191,#9192,#9193));
#2729=EDGE_LOOP('',(#9194,#9195,#9196,#9197));
#2730=EDGE_LOOP('',(#9198,#9199,#9200,#9201));
#2731=EDGE_LOOP('',(#9202,#9203,#9204,#9205));
#2732=EDGE_LOOP('',(#9206,#9207,#9208,#9209));
#2733=EDGE_LOOP('',(#9210,#9211,#9212,#9213));
#2734=EDGE_LOOP('',(#9214,#9215,#9216,#9217));
#2735=EDGE_LOOP('',(#9218));
#2736=EDGE_LOOP('',(#9219));
#2737=EDGE_LOOP('',(#9220,#9221,#9222,#9223));
#2738=EDGE_LOOP('',(#9224,#9225,#9226,#9227));
#2739=EDGE_LOOP('',(#9228));
#2740=EDGE_LOOP('',(#9229));
#2741=EDGE_LOOP('',(#9230));
#2742=EDGE_LOOP('',(#9231));
#2743=EDGE_LOOP('',(#9232,#9233,#9234,#9235));
#2744=EDGE_LOOP('',(#9236,#9237,#9238,#9239));
#2745=EDGE_LOOP('',(#9240));
#2746=EDGE_LOOP('',(#9241));
#2747=EDGE_LOOP('',(#9242));
#2748=EDGE_LOOP('',(#9243));
#2749=EDGE_LOOP('',(#9244,#9245));
#2750=EDGE_LOOP('',(#9246,#9247,#9248,#9249,#9250,#9251,#9252,#9253,#9254));
#2751=EDGE_LOOP('',(#9255,#9256,#9257));
#2752=EDGE_LOOP('',(#9258,#9259,#9260,#9261));
#2753=EDGE_LOOP('',(#9262,#9263,#9264,#9265));
#2754=EDGE_LOOP('',(#9266,#9267,#9268,#9269));
#2755=EDGE_LOOP('',(#9270,#9271));
#2756=EDGE_LOOP('',(#9272));
#2757=EDGE_LOOP('',(#9273));
#2758=EDGE_LOOP('',(#9274));
#2759=EDGE_LOOP('',(#9275));
#2760=EDGE_LOOP('',(#9276,#9277,#9278,#9279));
#2761=EDGE_LOOP('',(#9280,#9281,#9282,#9283));
#2762=EDGE_LOOP('',(#9284));
#2763=EDGE_LOOP('',(#9285));
#2764=EDGE_LOOP('',(#9286));
#2765=EDGE_LOOP('',(#9287));
#2766=EDGE_LOOP('',(#9288,#9289));
#2767=EDGE_LOOP('',(#9290,#9291,#9292,#9293,#9294,#9295,#9296,#9297,#9298));
#2768=EDGE_LOOP('',(#9299,#9300,#9301));
#2769=EDGE_LOOP('',(#9302,#9303,#9304,#9305));
#2770=EDGE_LOOP('',(#9306,#9307,#9308,#9309));
#2771=EDGE_LOOP('',(#9310,#9311,#9312,#9313));
#2772=EDGE_LOOP('',(#9314,#9315));
#2773=EDGE_LOOP('',(#9316));
#2774=EDGE_LOOP('',(#9317));
#2775=EDGE_LOOP('',(#9318));
#2776=EDGE_LOOP('',(#9319));
#2777=EDGE_LOOP('',(#9320,#9321,#9322,#9323));
#2778=EDGE_LOOP('',(#9324,#9325,#9326,#9327));
#2779=EDGE_LOOP('',(#9328));
#2780=EDGE_LOOP('',(#9329));
#2781=EDGE_LOOP('',(#9330));
#2782=EDGE_LOOP('',(#9331));
#2783=EDGE_LOOP('',(#9332,#9333,#9334,#9335));
#2784=EDGE_LOOP('',(#9336,#9337,#9338,#9339));
#2785=EDGE_LOOP('',(#9340,#9341,#9342,#9343));
#2786=EDGE_LOOP('',(#9344,#9345,#9346,#9347,#9348,#9349,#9350,#9351,#9352,
#9353,#9354,#9355,#9356,#9357,#9358,#9359,#9360,#9361,#9362,#9363,#9364,
#9365,#9366,#9367,#9368,#9369,#9370,#9371,#9372,#9373,#9374,#9375,#9376,
#9377,#9378,#9379,#9380,#9381,#9382,#9383,#9384,#9385,#9386,#9387,#9388,
#9389,#9390,#9391,#9392,#9393,#9394,#9395,#9396,#9397,#9398,#9399,#9400,
#9401,#9402,#9403,#9404,#9405,#9406,#9407,#9408,#9409,#9410,#9411,#9412,
#9413,#9414,#9415,#9416,#9417,#9418,#9419,#9420,#9421,#9422,#9423,#9424,
#9425,#9426,#9427,#9428,#9429,#9430,#9431,#9432,#9433,#9434,#9435,#9436,
#9437,#9438,#9439,#9440,#9441,#9442,#9443,#9444,#9445,#9446,#9447,#9448,
#9449,#9450,#9451,#9452,#9453,#9454,#9455,#9456,#9457,#9458,#9459,#9460,
#9461,#9462,#9463,#9464,#9465,#9466,#9467,#9468,#9469,#9470,#9471,#9472,
#9473,#9474,#9475,#9476,#9477,#9478,#9479,#9480,#9481,#9482,#9483,#9484,
#9485,#9486,#9487,#9488,#9489,#9490,#9491,#9492,#9493,#9494,#9495,#9496,
#9497,#9498,#9499,#9500,#9501,#9502,#9503));
#2787=EDGE_LOOP('',(#9504,#9505,#9506,#9507));
#2788=EDGE_LOOP('',(#9508,#9509,#9510,#9511));
#2789=EDGE_LOOP('',(#9512,#9513,#9514,#9515));
#2790=EDGE_LOOP('',(#9516));
#2791=EDGE_LOOP('',(#9517,#9518,#9519,#9520));
#2792=EDGE_LOOP('',(#9521,#9522,#9523,#9524));
#2793=EDGE_LOOP('',(#9525,#9526,#9527,#9528));
#2794=EDGE_LOOP('',(#9529,#9530,#9531,#9532));
#2795=EDGE_LOOP('',(#9533,#9534,#9535,#9536));
#2796=EDGE_LOOP('',(#9537,#9538,#9539,#9540));
#2797=EDGE_LOOP('',(#9541,#9542,#9543,#9544));
#2798=EDGE_LOOP('',(#9545,#9546,#9547,#9548));
#2799=EDGE_LOOP('',(#9549,#9550,#9551,#9552));
#2800=EDGE_LOOP('',(#9553,#9554,#9555,#9556));
#2801=EDGE_LOOP('',(#9557,#9558,#9559,#9560));
#2802=EDGE_LOOP('',(#9561,#9562,#9563,#9564));
#2803=EDGE_LOOP('',(#9565,#9566,#9567,#9568));
#2804=EDGE_LOOP('',(#9569,#9570,#9571,#9572));
#2805=EDGE_LOOP('',(#9573,#9574,#9575,#9576));
#2806=EDGE_LOOP('',(#9577,#9578,#9579,#9580));
#2807=EDGE_LOOP('',(#9581,#9582,#9583,#9584));
#2808=EDGE_LOOP('',(#9585,#9586,#9587,#9588));
#2809=EDGE_LOOP('',(#9589,#9590,#9591,#9592));
#2810=EDGE_LOOP('',(#9593,#9594,#9595,#9596));
#2811=EDGE_LOOP('',(#9597,#9598,#9599,#9600));
#2812=EDGE_LOOP('',(#9601,#9602,#9603,#9604));
#2813=EDGE_LOOP('',(#9605,#9606,#9607,#9608));
#2814=EDGE_LOOP('',(#9609,#9610,#9611,#9612));
#2815=EDGE_LOOP('',(#9613,#9614,#9615,#9616));
#2816=EDGE_LOOP('',(#9617,#9618,#9619,#9620));
#2817=EDGE_LOOP('',(#9621,#9622,#9623,#9624));
#2818=EDGE_LOOP('',(#9625,#9626,#9627,#9628));
#2819=EDGE_LOOP('',(#9629,#9630,#9631,#9632));
#2820=EDGE_LOOP('',(#9633,#9634,#9635,#9636));
#2821=EDGE_LOOP('',(#9637,#9638,#9639,#9640));
#2822=EDGE_LOOP('',(#9641,#9642,#9643,#9644));
#2823=EDGE_LOOP('',(#9645,#9646,#9647,#9648));
#2824=EDGE_LOOP('',(#9649,#9650,#9651,#9652));
#2825=EDGE_LOOP('',(#9653,#9654,#9655,#9656));
#2826=EDGE_LOOP('',(#9657,#9658,#9659,#9660));
#2827=EDGE_LOOP('',(#9661,#9662,#9663,#9664));
#2828=EDGE_LOOP('',(#9665,#9666,#9667,#9668));
#2829=EDGE_LOOP('',(#9669,#9670,#9671,#9672));
#2830=EDGE_LOOP('',(#9673,#9674,#9675,#9676));
#2831=EDGE_LOOP('',(#9677,#9678,#9679,#9680));
#2832=EDGE_LOOP('',(#9681,#9682,#9683,#9684));
#2833=EDGE_LOOP('',(#9685,#9686,#9687,#9688));
#2834=EDGE_LOOP('',(#9689,#9690,#9691,#9692));
#2835=EDGE_LOOP('',(#9693,#9694,#9695,#9696));
#2836=EDGE_LOOP('',(#9697,#9698,#9699,#9700));
#2837=EDGE_LOOP('',(#9701,#9702,#9703,#9704));
#2838=EDGE_LOOP('',(#9705,#9706,#9707,#9708));
#2839=EDGE_LOOP('',(#9709,#9710,#9711,#9712));
#2840=EDGE_LOOP('',(#9713,#9714,#9715,#9716));
#2841=EDGE_LOOP('',(#9717,#9718,#9719,#9720));
#2842=EDGE_LOOP('',(#9721,#9722,#9723,#9724));
#2843=EDGE_LOOP('',(#9725,#9726,#9727,#9728));
#2844=EDGE_LOOP('',(#9729,#9730,#9731,#9732));
#2845=EDGE_LOOP('',(#9733,#9734,#9735,#9736));
#2846=EDGE_LOOP('',(#9737,#9738,#9739,#9740));
#2847=EDGE_LOOP('',(#9741,#9742,#9743,#9744));
#2848=EDGE_LOOP('',(#9745,#9746,#9747,#9748));
#2849=EDGE_LOOP('',(#9749,#9750,#9751,#9752));
#2850=EDGE_LOOP('',(#9753,#9754,#9755,#9756));
#2851=EDGE_LOOP('',(#9757,#9758,#9759,#9760));
#2852=EDGE_LOOP('',(#9761,#9762,#9763,#9764));
#2853=EDGE_LOOP('',(#9765,#9766,#9767,#9768));
#2854=EDGE_LOOP('',(#9769,#9770,#9771,#9772));
#2855=EDGE_LOOP('',(#9773,#9774,#9775,#9776));
#2856=EDGE_LOOP('',(#9777,#9778,#9779,#9780));
#2857=EDGE_LOOP('',(#9781,#9782,#9783,#9784));
#2858=EDGE_LOOP('',(#9785,#9786,#9787,#9788));
#2859=EDGE_LOOP('',(#9789,#9790,#9791,#9792));
#2860=EDGE_LOOP('',(#9793,#9794,#9795,#9796));
#2861=EDGE_LOOP('',(#9797,#9798,#9799,#9800));
#2862=EDGE_LOOP('',(#9801,#9802,#9803,#9804));
#2863=EDGE_LOOP('',(#9805,#9806,#9807,#9808));
#2864=EDGE_LOOP('',(#9809,#9810,#9811,#9812));
#2865=EDGE_LOOP('',(#9813,#9814,#9815,#9816));
#2866=EDGE_LOOP('',(#9817,#9818,#9819,#9820));
#2867=EDGE_LOOP('',(#9821,#9822,#9823,#9824));
#2868=EDGE_LOOP('',(#9825,#9826,#9827,#9828));
#2869=EDGE_LOOP('',(#9829,#9830,#9831,#9832));
#2870=EDGE_LOOP('',(#9833,#9834,#9835,#9836));
#2871=EDGE_LOOP('',(#9837,#9838,#9839,#9840));
#2872=EDGE_LOOP('',(#9841,#9842,#9843,#9844));
#2873=EDGE_LOOP('',(#9845,#9846,#9847,#9848));
#2874=EDGE_LOOP('',(#9849,#9850,#9851,#9852));
#2875=EDGE_LOOP('',(#9853,#9854,#9855,#9856));
#2876=EDGE_LOOP('',(#9857,#9858,#9859,#9860));
#2877=EDGE_LOOP('',(#9861,#9862,#9863,#9864));
#2878=EDGE_LOOP('',(#9865,#9866,#9867,#9868));
#2879=EDGE_LOOP('',(#9869,#9870,#9871,#9872));
#2880=EDGE_LOOP('',(#9873,#9874,#9875,#9876));
#2881=EDGE_LOOP('',(#9877,#9878,#9879,#9880));
#2882=EDGE_LOOP('',(#9881,#9882,#9883,#9884));
#2883=EDGE_LOOP('',(#9885,#9886,#9887,#9888));
#2884=EDGE_LOOP('',(#9889,#9890,#9891,#9892));
#2885=EDGE_LOOP('',(#9893,#9894,#9895,#9896));
#2886=EDGE_LOOP('',(#9897,#9898,#9899,#9900));
#2887=EDGE_LOOP('',(#9901,#9902,#9903,#9904));
#2888=EDGE_LOOP('',(#9905,#9906,#9907,#9908));
#2889=EDGE_LOOP('',(#9909,#9910,#9911,#9912));
#2890=EDGE_LOOP('',(#9913,#9914,#9915,#9916));
#2891=EDGE_LOOP('',(#9917,#9918,#9919,#9920));
#2892=EDGE_LOOP('',(#9921,#9922,#9923,#9924));
#2893=EDGE_LOOP('',(#9925,#9926,#9927,#9928));
#2894=EDGE_LOOP('',(#9929,#9930,#9931,#9932));
#2895=EDGE_LOOP('',(#9933,#9934,#9935,#9936));
#2896=EDGE_LOOP('',(#9937,#9938,#9939,#9940));
#2897=EDGE_LOOP('',(#9941,#9942,#9943,#9944));
#2898=EDGE_LOOP('',(#9945,#9946,#9947,#9948));
#2899=EDGE_LOOP('',(#9949,#9950,#9951,#9952));
#2900=EDGE_LOOP('',(#9953,#9954,#9955,#9956));
#2901=EDGE_LOOP('',(#9957,#9958,#9959,#9960));
#2902=EDGE_LOOP('',(#9961,#9962,#9963,#9964));
#2903=EDGE_LOOP('',(#9965,#9966,#9967,#9968));
#2904=EDGE_LOOP('',(#9969,#9970,#9971,#9972));
#2905=EDGE_LOOP('',(#9973,#9974,#9975,#9976));
#2906=EDGE_LOOP('',(#9977,#9978,#9979,#9980));
#2907=EDGE_LOOP('',(#9981,#9982,#9983,#9984));
#2908=EDGE_LOOP('',(#9985,#9986,#9987,#9988));
#2909=EDGE_LOOP('',(#9989,#9990,#9991,#9992));
#2910=EDGE_LOOP('',(#9993,#9994,#9995,#9996));
#2911=EDGE_LOOP('',(#9997,#9998,#9999,#10000));
#2912=EDGE_LOOP('',(#10001,#10002,#10003,#10004));
#2913=EDGE_LOOP('',(#10005,#10006,#10007,#10008));
#2914=EDGE_LOOP('',(#10009,#10010,#10011,#10012));
#2915=EDGE_LOOP('',(#10013,#10014,#10015,#10016));
#2916=EDGE_LOOP('',(#10017,#10018,#10019,#10020));
#2917=EDGE_LOOP('',(#10021,#10022,#10023,#10024));
#2918=EDGE_LOOP('',(#10025,#10026,#10027,#10028));
#2919=EDGE_LOOP('',(#10029,#10030,#10031,#10032));
#2920=EDGE_LOOP('',(#10033,#10034,#10035,#10036));
#2921=EDGE_LOOP('',(#10037,#10038,#10039,#10040));
#2922=EDGE_LOOP('',(#10041,#10042,#10043,#10044));
#2923=EDGE_LOOP('',(#10045,#10046,#10047,#10048));
#2924=EDGE_LOOP('',(#10049,#10050,#10051,#10052));
#2925=EDGE_LOOP('',(#10053,#10054,#10055,#10056));
#2926=EDGE_LOOP('',(#10057,#10058,#10059,#10060));
#2927=EDGE_LOOP('',(#10061,#10062,#10063,#10064));
#2928=EDGE_LOOP('',(#10065,#10066,#10067,#10068));
#2929=EDGE_LOOP('',(#10069,#10070,#10071,#10072));
#2930=EDGE_LOOP('',(#10073,#10074,#10075,#10076));
#2931=EDGE_LOOP('',(#10077,#10078,#10079,#10080));
#2932=EDGE_LOOP('',(#10081,#10082,#10083,#10084));
#2933=EDGE_LOOP('',(#10085,#10086,#10087,#10088));
#2934=EDGE_LOOP('',(#10089,#10090,#10091,#10092));
#2935=EDGE_LOOP('',(#10093,#10094,#10095,#10096));
#2936=EDGE_LOOP('',(#10097,#10098,#10099,#10100));
#2937=EDGE_LOOP('',(#10101,#10102,#10103,#10104));
#2938=EDGE_LOOP('',(#10105,#10106,#10107,#10108));
#2939=EDGE_LOOP('',(#10109,#10110,#10111,#10112));
#2940=EDGE_LOOP('',(#10113,#10114,#10115,#10116));
#2941=EDGE_LOOP('',(#10117,#10118,#10119,#10120));
#2942=EDGE_LOOP('',(#10121,#10122,#10123,#10124));
#2943=EDGE_LOOP('',(#10125,#10126,#10127,#10128));
#2944=EDGE_LOOP('',(#10129,#10130,#10131,#10132));
#2945=EDGE_LOOP('',(#10133,#10134,#10135,#10136));
#2946=EDGE_LOOP('',(#10137,#10138,#10139,#10140));
#2947=EDGE_LOOP('',(#10141,#10142,#10143,#10144));
#2948=EDGE_LOOP('',(#10145,#10146,#10147,#10148));
#2949=EDGE_LOOP('',(#10149,#10150,#10151,#10152));
#2950=EDGE_LOOP('',(#10153,#10154,#10155,#10156));
#2951=EDGE_LOOP('',(#10157,#10158,#10159,#10160,#10161,#10162,#10163,#10164,
#10165,#10166,#10167,#10168,#10169,#10170,#10171,#10172,#10173,#10174,#10175,
#10176,#10177,#10178,#10179,#10180,#10181,#10182,#10183,#10184,#10185,#10186,
#10187,#10188,#10189,#10190,#10191,#10192,#10193,#10194,#10195,#10196,#10197,
#10198,#10199,#10200,#10201,#10202,#10203,#10204,#10205,#10206,#10207,#10208,
#10209,#10210,#10211,#10212,#10213,#10214,#10215,#10216,#10217,#10218,#10219,
#10220,#10221,#10222,#10223,#10224,#10225,#10226,#10227,#10228,#10229,#10230,
#10231,#10232,#10233,#10234,#10235,#10236,#10237,#10238,#10239,#10240,#10241,
#10242,#10243,#10244,#10245,#10246,#10247,#10248,#10249,#10250,#10251,#10252,
#10253,#10254,#10255,#10256,#10257,#10258,#10259,#10260,#10261,#10262,#10263,
#10264,#10265,#10266,#10267,#10268,#10269,#10270,#10271,#10272,#10273,#10274,
#10275,#10276,#10277,#10278,#10279,#10280,#10281,#10282,#10283,#10284,#10285,
#10286,#10287,#10288,#10289,#10290,#10291,#10292,#10293,#10294,#10295,#10296,
#10297,#10298,#10299,#10300,#10301,#10302,#10303,#10304,#10305,#10306,#10307,
#10308,#10309,#10310,#10311,#10312,#10313,#10314,#10315,#10316));
#2952=EDGE_LOOP('',(#10317));
#2953=EDGE_LOOP('',(#10318,#10319,#10320,#10321));
#2954=EDGE_LOOP('',(#10322,#10323,#10324,#10325,#10326,#10327,#10328,#10329));
#2955=EDGE_LOOP('',(#10330,#10331,#10332,#10333));
#2956=EDGE_LOOP('',(#10334,#10335,#10336,#10337));
#2957=EDGE_LOOP('',(#10338,#10339,#10340,#10341));
#2958=EDGE_LOOP('',(#10342,#10343,#10344,#10345));
#2959=EDGE_LOOP('',(#10346,#10347,#10348,#10349,#10350,#10351,#10352,#10353));
#2960=EDGE_LOOP('',(#10354,#10355,#10356,#10357));
#2961=EDGE_LOOP('',(#10358,#10359,#10360,#10361));
#2962=EDGE_LOOP('',(#10362,#10363,#10364,#10365));
#2963=EDGE_LOOP('',(#10366,#10367,#10368,#10369));
#2964=EDGE_LOOP('',(#10370,#10371,#10372,#10373));
#2965=EDGE_LOOP('',(#10374,#10375,#10376,#10377));
#2966=EDGE_LOOP('',(#10378,#10379,#10380,#10381));
#2967=EDGE_LOOP('',(#10382,#10383,#10384,#10385));
#2968=EDGE_LOOP('',(#10386,#10387,#10388,#10389));
#2969=EDGE_LOOP('',(#10390,#10391,#10392,#10393));
#2970=EDGE_LOOP('',(#10394,#10395,#10396,#10397,#10398,#10399));
#2971=EDGE_LOOP('',(#10400));
#2972=EDGE_LOOP('',(#10401,#10402,#10403,#10404,#10405,#10406));
#2973=EDGE_LOOP('',(#10407,#10408,#10409,#10410));
#2974=EDGE_LOOP('',(#10411,#10412,#10413,#10414));
#2975=EDGE_LOOP('',(#10415,#10416,#10417,#10418));
#2976=EDGE_LOOP('',(#10419));
#2977=LINE('',#15982,#3618);
#2978=LINE('',#15988,#3619);
#2979=LINE('',#15994,#3620);
#2980=LINE('',#16000,#3621);
#2981=LINE('',#16005,#3622);
#2982=LINE('',#16007,#3623);
#2983=LINE('',#16009,#3624);
#2984=LINE('',#16010,#3625);
#2985=LINE('',#16013,#3626);
#2986=LINE('',#16015,#3627);
#2987=LINE('',#16016,#3628);
#2988=LINE('',#16019,#3629);
#2989=LINE('',#16021,#3630);
#2990=LINE('',#16022,#3631);
#2991=LINE('',#16024,#3632);
#2992=LINE('',#16025,#3633);
#2993=LINE('',#16033,#3634);
#2994=LINE('',#16039,#3635);
#2995=LINE('',#16045,#3636);
#2996=LINE('',#16051,#3637);
#2997=LINE('',#16057,#3638);
#2998=LINE('',#16063,#3639);
#2999=LINE('',#16069,#3640);
#3000=LINE('',#16078,#3641);
#3001=LINE('',#16087,#3642);
#3002=LINE('',#16096,#3643);
#3003=LINE('',#16103,#3644);
#3004=LINE('',#16107,#3645);
#3005=LINE('',#16111,#3646);
#3006=LINE('',#16115,#3647);
#3007=LINE('',#16121,#3648);
#3008=LINE('',#16128,#3649);
#3009=LINE('',#16135,#3650);
#3010=LINE('',#16142,#3651);
#3011=LINE('',#16148,#3652);
#3012=LINE('',#16155,#3653);
#3013=LINE('',#16160,#3654);
#3014=LINE('',#16162,#3655);
#3015=LINE('',#16164,#3656);
#3016=LINE('',#16165,#3657);
#3017=LINE('',#16168,#3658);
#3018=LINE('',#16170,#3659);
#3019=LINE('',#16171,#3660);
#3020=LINE('',#16174,#3661);
#3021=LINE('',#16176,#3662);
#3022=LINE('',#16177,#3663);
#3023=LINE('',#16179,#3664);
#3024=LINE('',#16180,#3665);
#3025=LINE('',#16188,#3666);
#3026=LINE('',#16194,#3667);
#3027=LINE('',#16200,#3668);
#3028=LINE('',#16206,#3669);
#3029=LINE('',#16212,#3670);
#3030=LINE('',#16218,#3671);
#3031=LINE('',#16224,#3672);
#3032=LINE('',#16233,#3673);
#3033=LINE('',#16242,#3674);
#3034=LINE('',#16251,#3675);
#3035=LINE('',#16259,#3676);
#3036=LINE('',#16263,#3677);
#3037=LINE('',#16267,#3678);
#3038=LINE('',#16271,#3679);
#3039=LINE('',#16276,#3680);
#3040=LINE('',#16283,#3681);
#3041=LINE('',#16290,#3682);
#3042=LINE('',#16298,#3683);
#3043=LINE('',#16303,#3684);
#3044=LINE('',#16311,#3685);
#3045=LINE('',#16315,#3686);
#3046=LINE('',#16317,#3687);
#3047=LINE('',#16319,#3688);
#3048=LINE('',#16320,#3689);
#3049=LINE('',#16323,#3690);
#3050=LINE('',#16325,#3691);
#3051=LINE('',#16326,#3692);
#3052=LINE('',#16329,#3693);
#3053=LINE('',#16331,#3694);
#3054=LINE('',#16332,#3695);
#3055=LINE('',#16334,#3696);
#3056=LINE('',#16335,#3697);
#3057=LINE('',#16343,#3698);
#3058=LINE('',#16349,#3699);
#3059=LINE('',#16358,#3700);
#3060=LINE('',#16364,#3701);
#3061=LINE('',#16373,#3702);
#3062=LINE('',#16379,#3703);
#3063=LINE('',#16388,#3704);
#3064=LINE('',#16394,#3705);
#3065=LINE('',#16403,#3706);
#3066=LINE('',#16409,#3707);
#3067=LINE('',#16415,#3708);
#3068=LINE('',#16421,#3709);
#3069=LINE('',#16428,#3710);
#3070=LINE('',#16434,#3711);
#3071=LINE('',#16443,#3712);
#3072=LINE('',#16449,#3713);
#3073=LINE('',#16455,#3714);
#3074=LINE('',#16461,#3715);
#3075=LINE('',#16468,#3716);
#3076=LINE('',#16474,#3717);
#3077=LINE('',#16483,#3718);
#3078=LINE('',#16489,#3719);
#3079=LINE('',#16495,#3720);
#3080=LINE('',#16501,#3721);
#3081=LINE('',#16509,#3722);
#3082=LINE('',#16514,#3723);
#3083=LINE('',#16523,#3724);
#3084=LINE('',#16529,#3725);
#3085=LINE('',#16535,#3726);
#3086=LINE('',#16541,#3727);
#3087=LINE('',#16549,#3728);
#3088=LINE('',#16554,#3729);
#3089=LINE('',#16565,#3730);
#3090=LINE('',#16569,#3731);
#3091=LINE('',#16573,#3732);
#3092=LINE('',#16580,#3733);
#3093=LINE('',#16584,#3734);
#3094=LINE('',#16588,#3735);
#3095=LINE('',#16593,#3736);
#3096=LINE('',#16595,#3737);
#3097=LINE('',#16597,#3738);
#3098=LINE('',#16598,#3739);
#3099=LINE('',#16601,#3740);
#3100=LINE('',#16603,#3741);
#3101=LINE('',#16604,#3742);
#3102=LINE('',#16607,#3743);
#3103=LINE('',#16609,#3744);
#3104=LINE('',#16610,#3745);
#3105=LINE('',#16613,#3746);
#3106=LINE('',#16615,#3747);
#3107=LINE('',#16616,#3748);
#3108=LINE('',#16619,#3749);
#3109=LINE('',#16621,#3750);
#3110=LINE('',#16622,#3751);
#3111=LINE('',#16624,#3752);
#3112=LINE('',#16625,#3753);
#3113=LINE('',#16635,#3754);
#3114=LINE('',#16639,#3755);
#3115=LINE('',#16643,#3756);
#3116=LINE('',#16650,#3757);
#3117=LINE('',#16654,#3758);
#3118=LINE('',#16658,#3759);
#3119=LINE('',#16663,#3760);
#3120=LINE('',#16665,#3761);
#3121=LINE('',#16667,#3762);
#3122=LINE('',#16668,#3763);
#3123=LINE('',#16671,#3764);
#3124=LINE('',#16673,#3765);
#3125=LINE('',#16674,#3766);
#3126=LINE('',#16677,#3767);
#3127=LINE('',#16679,#3768);
#3128=LINE('',#16680,#3769);
#3129=LINE('',#16683,#3770);
#3130=LINE('',#16685,#3771);
#3131=LINE('',#16686,#3772);
#3132=LINE('',#16689,#3773);
#3133=LINE('',#16691,#3774);
#3134=LINE('',#16692,#3775);
#3135=LINE('',#16694,#3776);
#3136=LINE('',#16695,#3777);
#3137=LINE('',#16712,#3778);
#3138=LINE('',#16718,#3779);
#3139=LINE('',#16722,#3780);
#3140=LINE('',#16728,#3781);
#3141=LINE('',#16733,#3782);
#3142=LINE('',#16748,#3783);
#3143=LINE('',#16757,#3784);
#3144=LINE('',#16761,#3785);
#3145=LINE('',#16765,#3786);
#3146=LINE('',#16768,#3787);
#3147=LINE('',#16904,#3788);
#3148=LINE('',#17157,#3789);
#3149=LINE('',#17199,#3790);
#3150=LINE('',#17204,#3791);
#3151=LINE('',#17213,#3792);
#3152=LINE('',#17218,#3793);
#3153=LINE('',#17238,#3794);
#3154=LINE('',#17244,#3795);
#3155=LINE('',#17248,#3796);
#3156=LINE('',#17254,#3797);
#3157=LINE('',#17259,#3798);
#3158=LINE('',#17274,#3799);
#3159=LINE('',#17283,#3800);
#3160=LINE('',#17287,#3801);
#3161=LINE('',#17291,#3802);
#3162=LINE('',#17294,#3803);
#3163=LINE('',#17447,#3804);
#3164=LINE('',#17743,#3805);
#3165=LINE('',#17785,#3806);
#3166=LINE('',#17790,#3807);
#3167=LINE('',#17799,#3808);
#3168=LINE('',#17804,#3809);
#3169=LINE('',#17817,#3810);
#3170=LINE('',#17821,#3811);
#3171=LINE('',#17825,#3812);
#3172=LINE('',#17832,#3813);
#3173=LINE('',#17836,#3814);
#3174=LINE('',#17840,#3815);
#3175=LINE('',#17845,#3816);
#3176=LINE('',#17847,#3817);
#3177=LINE('',#17849,#3818);
#3178=LINE('',#17850,#3819);
#3179=LINE('',#17853,#3820);
#3180=LINE('',#17855,#3821);
#3181=LINE('',#17856,#3822);
#3182=LINE('',#17859,#3823);
#3183=LINE('',#17861,#3824);
#3184=LINE('',#17862,#3825);
#3185=LINE('',#17865,#3826);
#3186=LINE('',#17867,#3827);
#3187=LINE('',#17868,#3828);
#3188=LINE('',#17871,#3829);
#3189=LINE('',#17873,#3830);
#3190=LINE('',#17874,#3831);
#3191=LINE('',#17876,#3832);
#3192=LINE('',#17877,#3833);
#3193=LINE('',#17924,#3834);
#3194=LINE('',#17926,#3835);
#3195=LINE('',#17928,#3836);
#3196=LINE('',#17929,#3837);
#3197=LINE('',#17934,#3838);
#3198=LINE('',#17935,#3839);
#3199=LINE('',#17938,#3840);
#3200=LINE('',#17940,#3841);
#3201=LINE('',#17941,#3842);
#3202=LINE('',#17943,#3843);
#3203=LINE('',#17950,#3844);
#3204=LINE('',#17959,#3845);
#3205=LINE('',#17965,#3846);
#3206=LINE('',#17974,#3847);
#3207=LINE('',#17980,#3848);
#3208=LINE('',#17988,#3849);
#3209=LINE('',#18005,#3850);
#3210=LINE('',#18056,#3851);
#3211=LINE('',#18061,#3852);
#3212=LINE('',#18067,#3853);
#3213=LINE('',#18076,#3854);
#3214=LINE('',#18082,#3855);
#3215=LINE('',#18090,#3856);
#3216=LINE('',#18107,#3857);
#3217=LINE('',#18158,#3858);
#3218=LINE('',#18163,#3859);
#3219=LINE('',#18169,#3860);
#3220=LINE('',#18178,#3861);
#3221=LINE('',#18184,#3862);
#3222=LINE('',#18192,#3863);
#3223=LINE('',#18194,#3864);
#3224=LINE('',#18196,#3865);
#3225=LINE('',#18197,#3866);
#3226=LINE('',#18200,#3867);
#3227=LINE('',#18202,#3868);
#3228=LINE('',#18203,#3869);
#3229=LINE('',#18206,#3870);
#3230=LINE('',#18208,#3871);
#3231=LINE('',#18209,#3872);
#3232=LINE('',#18286,#3873);
#3233=LINE('',#18432,#3874);
#3234=LINE('',#18578,#3875);
#3235=LINE('',#18724,#3876);
#3236=LINE('',#18870,#3877);
#3237=LINE('',#19016,#3878);
#3238=LINE('',#19162,#3879);
#3239=LINE('',#19308,#3880);
#3240=LINE('',#19454,#3881);
#3241=LINE('',#19600,#3882);
#3242=LINE('',#19746,#3883);
#3243=LINE('',#19892,#3884);
#3244=LINE('',#20038,#3885);
#3245=LINE('',#20184,#3886);
#3246=LINE('',#20330,#3887);
#3247=LINE('',#20476,#3888);
#3248=LINE('',#20622,#3889);
#3249=LINE('',#20768,#3890);
#3250=LINE('',#20914,#3891);
#3251=LINE('',#21060,#3892);
#3252=LINE('',#21138,#3893);
#3253=LINE('',#21282,#3894);
#3254=LINE('',#21354,#3895);
#3255=LINE('',#21357,#3896);
#3256=LINE('',#21358,#3897);
#3257=LINE('',#21570,#3898);
#3258=LINE('',#21574,#3899);
#3259=LINE('',#21786,#3900);
#3260=LINE('',#21789,#3901);
#3261=LINE('',#21790,#3902);
#3262=LINE('',#22002,#3903);
#3263=LINE('',#22006,#3904);
#3264=LINE('',#22218,#3905);
#3265=LINE('',#22221,#3906);
#3266=LINE('',#22222,#3907);
#3267=LINE('',#22434,#3908);
#3268=LINE('',#22438,#3909);
#3269=LINE('',#22650,#3910);
#3270=LINE('',#22653,#3911);
#3271=LINE('',#22654,#3912);
#3272=LINE('',#22866,#3913);
#3273=LINE('',#22870,#3914);
#3274=LINE('',#23082,#3915);
#3275=LINE('',#23085,#3916);
#3276=LINE('',#23086,#3917);
#3277=LINE('',#23298,#3918);
#3278=LINE('',#23302,#3919);
#3279=LINE('',#23514,#3920);
#3280=LINE('',#23517,#3921);
#3281=LINE('',#23518,#3922);
#3282=LINE('',#23730,#3923);
#3283=LINE('',#23734,#3924);
#3284=LINE('',#23946,#3925);
#3285=LINE('',#23949,#3926);
#3286=LINE('',#23950,#3927);
#3287=LINE('',#24162,#3928);
#3288=LINE('',#24166,#3929);
#3289=LINE('',#24378,#3930);
#3290=LINE('',#24381,#3931);
#3291=LINE('',#24382,#3932);
#3292=LINE('',#24594,#3933);
#3293=LINE('',#24598,#3934);
#3294=LINE('',#24810,#3935);
#3295=LINE('',#24813,#3936);
#3296=LINE('',#24814,#3937);
#3297=LINE('',#25026,#3938);
#3298=LINE('',#25030,#3939);
#3299=LINE('',#25242,#3940);
#3300=LINE('',#25245,#3941);
#3301=LINE('',#25246,#3942);
#3302=LINE('',#25458,#3943);
#3303=LINE('',#25462,#3944);
#3304=LINE('',#25674,#3945);
#3305=LINE('',#25677,#3946);
#3306=LINE('',#25678,#3947);
#3307=LINE('',#25890,#3948);
#3308=LINE('',#25894,#3949);
#3309=LINE('',#26106,#3950);
#3310=LINE('',#26109,#3951);
#3311=LINE('',#26110,#3952);
#3312=LINE('',#26322,#3953);
#3313=LINE('',#26326,#3954);
#3314=LINE('',#26538,#3955);
#3315=LINE('',#26541,#3956);
#3316=LINE('',#26542,#3957);
#3317=LINE('',#26754,#3958);
#3318=LINE('',#26758,#3959);
#3319=LINE('',#26970,#3960);
#3320=LINE('',#26973,#3961);
#3321=LINE('',#26974,#3962);
#3322=LINE('',#27186,#3963);
#3323=LINE('',#27190,#3964);
#3324=LINE('',#27402,#3965);
#3325=LINE('',#27405,#3966);
#3326=LINE('',#27406,#3967);
#3327=LINE('',#27618,#3968);
#3328=LINE('',#27622,#3969);
#3329=LINE('',#27834,#3970);
#3330=LINE('',#27837,#3971);
#3331=LINE('',#27838,#3972);
#3332=LINE('',#28050,#3973);
#3333=LINE('',#28054,#3974);
#3334=LINE('',#28266,#3975);
#3335=LINE('',#28269,#3976);
#3336=LINE('',#28270,#3977);
#3337=LINE('',#28482,#3978);
#3338=LINE('',#28486,#3979);
#3339=LINE('',#28698,#3980);
#3340=LINE('',#28701,#3981);
#3341=LINE('',#28702,#3982);
#3342=LINE('',#28914,#3983);
#3343=LINE('',#28918,#3984);
#3344=LINE('',#29130,#3985);
#3345=LINE('',#29133,#3986);
#3346=LINE('',#29134,#3987);
#3347=LINE('',#29346,#3988);
#3348=LINE('',#29350,#3989);
#3349=LINE('',#29562,#3990);
#3350=LINE('',#29565,#3991);
#3351=LINE('',#29566,#3992);
#3352=LINE('',#29778,#3993);
#3353=LINE('',#29786,#3994);
#3354=LINE('',#29788,#3995);
#3355=LINE('',#29790,#3996);
#3356=LINE('',#29791,#3997);
#3357=LINE('',#29795,#3998);
#3358=LINE('',#29801,#3999);
#3359=LINE('',#29802,#4000);
#3360=LINE('',#29803,#4001);
#3361=LINE('',#29809,#4002);
#3362=LINE('',#29812,#4003);
#3363=LINE('',#29815,#4004);
#3364=LINE('',#29816,#4005);
#3365=LINE('',#29820,#4006);
#3366=LINE('',#29822,#4007);
#3367=LINE('',#29823,#4008);
#3368=LINE('',#29826,#4009);
#3369=LINE('',#29831,#4010);
#3370=LINE('',#29832,#4011);
#3371=LINE('',#29833,#4012);
#3372=LINE('',#29838,#4013);
#3373=LINE('',#29846,#4014);
#3374=LINE('',#29848,#4015);
#3375=LINE('',#29850,#4016);
#3376=LINE('',#29851,#4017);
#3377=LINE('',#29856,#4018);
#3378=LINE('',#29857,#4019);
#3379=LINE('',#29860,#4020);
#3380=LINE('',#29862,#4021);
#3381=LINE('',#29863,#4022);
#3382=LINE('',#29865,#4023);
#3383=LINE('',#29872,#4024);
#3384=LINE('',#29881,#4025);
#3385=LINE('',#29887,#4026);
#3386=LINE('',#29896,#4027);
#3387=LINE('',#29902,#4028);
#3388=LINE('',#29910,#4029);
#3389=LINE('',#29931,#4030);
#3390=LINE('',#29986,#4031);
#3391=LINE('',#29991,#4032);
#3392=LINE('',#29997,#4033);
#3393=LINE('',#30006,#4034);
#3394=LINE('',#30012,#4035);
#3395=LINE('',#30020,#4036);
#3396=LINE('',#30041,#4037);
#3397=LINE('',#30096,#4038);
#3398=LINE('',#30101,#4039);
#3399=LINE('',#30107,#4040);
#3400=LINE('',#30116,#4041);
#3401=LINE('',#30122,#4042);
#3402=LINE('',#30130,#4043);
#3403=LINE('',#30132,#4044);
#3404=LINE('',#30134,#4045);
#3405=LINE('',#30135,#4046);
#3406=LINE('',#30138,#4047);
#3407=LINE('',#30140,#4048);
#3408=LINE('',#30141,#4049);
#3409=LINE('',#30144,#4050);
#3410=LINE('',#30146,#4051);
#3411=LINE('',#30147,#4052);
#3412=LINE('',#30224,#4053);
#3413=LINE('',#30370,#4054);
#3414=LINE('',#30516,#4055);
#3415=LINE('',#30662,#4056);
#3416=LINE('',#30808,#4057);
#3417=LINE('',#30954,#4058);
#3418=LINE('',#31100,#4059);
#3419=LINE('',#31246,#4060);
#3420=LINE('',#31392,#4061);
#3421=LINE('',#31538,#4062);
#3422=LINE('',#31684,#4063);
#3423=LINE('',#31830,#4064);
#3424=LINE('',#31976,#4065);
#3425=LINE('',#32122,#4066);
#3426=LINE('',#32268,#4067);
#3427=LINE('',#32414,#4068);
#3428=LINE('',#32560,#4069);
#3429=LINE('',#32706,#4070);
#3430=LINE('',#32852,#4071);
#3431=LINE('',#32998,#4072);
#3432=LINE('',#33144,#4073);
#3433=LINE('',#33290,#4074);
#3434=LINE('',#33436,#4075);
#3435=LINE('',#33582,#4076);
#3436=LINE('',#33728,#4077);
#3437=LINE('',#33874,#4078);
#3438=LINE('',#34020,#4079);
#3439=LINE('',#34166,#4080);
#3440=LINE('',#34312,#4081);
#3441=LINE('',#34458,#4082);
#3442=LINE('',#34604,#4083);
#3443=LINE('',#34750,#4084);
#3444=LINE('',#34896,#4085);
#3445=LINE('',#35042,#4086);
#3446=LINE('',#35188,#4087);
#3447=LINE('',#35334,#4088);
#3448=LINE('',#35480,#4089);
#3449=LINE('',#35626,#4090);
#3450=LINE('',#35772,#4091);
#3451=LINE('',#35918,#4092);
#3452=LINE('',#35996,#4093);
#3453=LINE('',#36217,#4094);
#3454=LINE('',#36366,#4095);
#3455=LINE('',#36438,#4096);
#3456=LINE('',#36659,#4097);
#3457=LINE('',#36808,#4098);
#3458=LINE('',#36880,#4099);
#3459=LINE('',#37101,#4100);
#3460=LINE('',#37250,#4101);
#3461=LINE('',#37322,#4102);
#3462=LINE('',#37543,#4103);
#3463=LINE('',#37692,#4104);
#3464=LINE('',#37764,#4105);
#3465=LINE('',#37985,#4106);
#3466=LINE('',#38134,#4107);
#3467=LINE('',#38206,#4108);
#3468=LINE('',#38427,#4109);
#3469=LINE('',#38576,#4110);
#3470=LINE('',#38648,#4111);
#3471=LINE('',#38869,#4112);
#3472=LINE('',#39018,#4113);
#3473=LINE('',#39090,#4114);
#3474=LINE('',#39311,#4115);
#3475=LINE('',#39460,#4116);
#3476=LINE('',#39532,#4117);
#3477=LINE('',#39753,#4118);
#3478=LINE('',#39902,#4119);
#3479=LINE('',#39974,#4120);
#3480=LINE('',#40195,#4121);
#3481=LINE('',#40344,#4122);
#3482=LINE('',#40416,#4123);
#3483=LINE('',#40637,#4124);
#3484=LINE('',#40786,#4125);
#3485=LINE('',#40858,#4126);
#3486=LINE('',#41079,#4127);
#3487=LINE('',#41228,#4128);
#3488=LINE('',#41300,#4129);
#3489=LINE('',#41521,#4130);
#3490=LINE('',#41670,#4131);
#3491=LINE('',#41742,#4132);
#3492=LINE('',#41963,#4133);
#3493=LINE('',#42112,#4134);
#3494=LINE('',#42184,#4135);
#3495=LINE('',#42405,#4136);
#3496=LINE('',#42554,#4137);
#3497=LINE('',#42626,#4138);
#3498=LINE('',#42847,#4139);
#3499=LINE('',#42996,#4140);
#3500=LINE('',#43068,#4141);
#3501=LINE('',#43289,#4142);
#3502=LINE('',#43438,#4143);
#3503=LINE('',#43510,#4144);
#3504=LINE('',#43731,#4145);
#3505=LINE('',#43880,#4146);
#3506=LINE('',#43952,#4147);
#3507=LINE('',#44173,#4148);
#3508=LINE('',#44322,#4149);
#3509=LINE('',#44394,#4150);
#3510=LINE('',#44615,#4151);
#3511=LINE('',#44764,#4152);
#3512=LINE('',#44836,#4153);
#3513=LINE('',#45057,#4154);
#3514=LINE('',#45206,#4155);
#3515=LINE('',#45278,#4156);
#3516=LINE('',#45499,#4157);
#3517=LINE('',#45648,#4158);
#3518=LINE('',#45720,#4159);
#3519=LINE('',#45941,#4160);
#3520=LINE('',#46090,#4161);
#3521=LINE('',#46162,#4162);
#3522=LINE('',#46383,#4163);
#3523=LINE('',#46532,#4164);
#3524=LINE('',#46604,#4165);
#3525=LINE('',#46825,#4166);
#3526=LINE('',#46974,#4167);
#3527=LINE('',#47046,#4168);
#3528=LINE('',#47267,#4169);
#3529=LINE('',#47416,#4170);
#3530=LINE('',#47488,#4171);
#3531=LINE('',#47709,#4172);
#3532=LINE('',#47858,#4173);
#3533=LINE('',#47930,#4174);
#3534=LINE('',#48151,#4175);
#3535=LINE('',#48300,#4176);
#3536=LINE('',#48372,#4177);
#3537=LINE('',#48593,#4178);
#3538=LINE('',#48742,#4179);
#3539=LINE('',#48814,#4180);
#3540=LINE('',#49035,#4181);
#3541=LINE('',#49184,#4182);
#3542=LINE('',#49256,#4183);
#3543=LINE('',#49477,#4184);
#3544=LINE('',#49626,#4185);
#3545=LINE('',#49698,#4186);
#3546=LINE('',#49919,#4187);
#3547=LINE('',#50068,#4188);
#3548=LINE('',#50140,#4189);
#3549=LINE('',#50361,#4190);
#3550=LINE('',#50510,#4191);
#3551=LINE('',#50582,#4192);
#3552=LINE('',#50803,#4193);
#3553=LINE('',#50952,#4194);
#3554=LINE('',#51024,#4195);
#3555=LINE('',#51245,#4196);
#3556=LINE('',#51394,#4197);
#3557=LINE('',#51466,#4198);
#3558=LINE('',#51687,#4199);
#3559=LINE('',#51836,#4200);
#3560=LINE('',#51908,#4201);
#3561=LINE('',#52129,#4202);
#3562=LINE('',#52278,#4203);
#3563=LINE('',#52350,#4204);
#3564=LINE('',#52571,#4205);
#3565=LINE('',#52720,#4206);
#3566=LINE('',#52792,#4207);
#3567=LINE('',#53013,#4208);
#3568=LINE('',#53016,#4209);
#3569=LINE('',#53017,#4210);
#3570=LINE('',#53392,#4211);
#3571=LINE('',#53674,#4212);
#3572=LINE('',#53676,#4213);
#3573=LINE('',#53684,#4214);
#3574=LINE('',#53686,#4215);
#3575=LINE('',#53688,#4216);
#3576=LINE('',#53690,#4217);
#3577=LINE('',#53692,#4218);
#3578=LINE('',#53694,#4219);
#3579=LINE('',#53696,#4220);
#3580=LINE('',#53697,#4221);
#3581=LINE('',#53700,#4222);
#3582=LINE('',#53702,#4223);
#3583=LINE('',#53703,#4224);
#3584=LINE('',#53706,#4225);
#3585=LINE('',#53707,#4226);
#3586=LINE('',#53710,#4227);
#3587=LINE('',#53711,#4228);
#3588=LINE('',#53714,#4229);
#3589=LINE('',#53715,#4230);
#3590=LINE('',#53719,#4231);
#3591=LINE('',#53720,#4232);
#3592=LINE('',#53722,#4233);
#3593=LINE('',#53723,#4234);
#3594=LINE('',#53725,#4235);
#3595=LINE('',#53727,#4236);
#3596=LINE('',#53729,#4237);
#3597=LINE('',#53735,#4238);
#3598=LINE('',#53737,#4239);
#3599=LINE('',#53739,#4240);
#3600=LINE('',#53740,#4241);
#3601=LINE('',#53743,#4242);
#3602=LINE('',#53745,#4243);
#3603=LINE('',#53746,#4244);
#3604=LINE('',#53749,#4245);
#3605=LINE('',#53751,#4246);
#3606=LINE('',#53752,#4247);
#3607=LINE('',#53755,#4248);
#3608=LINE('',#53757,#4249);
#3609=LINE('',#53758,#4250);
#3610=LINE('',#53761,#4251);
#3611=LINE('',#53763,#4252);
#3612=LINE('',#53764,#4253);
#3613=LINE('',#53766,#4254);
#3614=LINE('',#53767,#4255);
#3615=LINE('',#53775,#4256);
#3616=LINE('',#53779,#4257);
#3617=LINE('',#53783,#4258);
#3618=VECTOR('',#12992,0.33);
#3619=VECTOR('',#12999,0.33);
#3620=VECTOR('',#13006,0.33);
#3621=VECTOR('',#13013,0.33);
#3622=VECTOR('',#13018,1.);
#3623=VECTOR('',#13019,1.);
#3624=VECTOR('',#13020,1.);
#3625=VECTOR('',#13021,1.);
#3626=VECTOR('',#13024,1.);
#3627=VECTOR('',#13025,1.);
#3628=VECTOR('',#13026,1.);
#3629=VECTOR('',#13029,1.);
#3630=VECTOR('',#13030,1.);
#3631=VECTOR('',#13031,1.);
#3632=VECTOR('',#13034,1.);
#3633=VECTOR('',#13035,1.);
#3634=VECTOR('',#13046,0.165);
#3635=VECTOR('',#13053,0.165);
#3636=VECTOR('',#13060,0.164999999999999);
#3637=VECTOR('',#13067,0.165);
#3638=VECTOR('',#13074,0.165);
#3639=VECTOR('',#13081,0.165);
#3640=VECTOR('',#13088,0.475);
#3641=VECTOR('',#13099,0.475);
#3642=VECTOR('',#13110,0.475);
#3643=VECTOR('',#13121,0.475);
#3644=VECTOR('',#13130,0.275);
#3645=VECTOR('',#13135,0.275);
#3646=VECTOR('',#13140,0.275);
#3647=VECTOR('',#13145,0.275);
#3648=VECTOR('',#13152,0.25);
#3649=VECTOR('',#13161,0.25);
#3650=VECTOR('',#13170,2.35);
#3651=VECTOR('',#13179,2.15);
#3652=VECTOR('',#13186,1.6);
#3653=VECTOR('',#13195,1.4);
#3654=VECTOR('',#13200,1.);
#3655=VECTOR('',#13201,1.);
#3656=VECTOR('',#13202,1.);
#3657=VECTOR('',#13203,1.);
#3658=VECTOR('',#13206,1.);
#3659=VECTOR('',#13207,1.);
#3660=VECTOR('',#13208,1.);
#3661=VECTOR('',#13211,1.);
#3662=VECTOR('',#13212,1.);
#3663=VECTOR('',#13213,1.);
#3664=VECTOR('',#13216,1.);
#3665=VECTOR('',#13217,1.);
#3666=VECTOR('',#13228,0.165);
#3667=VECTOR('',#13235,0.165);
#3668=VECTOR('',#13242,0.164999999999999);
#3669=VECTOR('',#13249,0.165);
#3670=VECTOR('',#13256,0.165);
#3671=VECTOR('',#13263,0.165);
#3672=VECTOR('',#13270,0.475);
#3673=VECTOR('',#13281,0.475);
#3674=VECTOR('',#13292,0.475);
#3675=VECTOR('',#13303,0.475);
#3676=VECTOR('',#13314,0.275);
#3677=VECTOR('',#13319,0.275);
#3678=VECTOR('',#13324,0.275);
#3679=VECTOR('',#13329,0.275);
#3680=VECTOR('',#13334,0.25);
#3681=VECTOR('',#13343,0.25);
#3682=VECTOR('',#13352,2.35);
#3683=VECTOR('',#13363,2.15);
#3684=VECTOR('',#13368,1.6);
#3685=VECTOR('',#13379,1.4);
#3686=VECTOR('',#13382,1.);
#3687=VECTOR('',#13383,1.);
#3688=VECTOR('',#13384,1.);
#3689=VECTOR('',#13385,1.);
#3690=VECTOR('',#13388,1.);
#3691=VECTOR('',#13389,1.);
#3692=VECTOR('',#13390,1.);
#3693=VECTOR('',#13393,1.);
#3694=VECTOR('',#13394,1.);
#3695=VECTOR('',#13395,1.);
#3696=VECTOR('',#13398,1.);
#3697=VECTOR('',#13399,1.);
#3698=VECTOR('',#13410,0.21);
#3699=VECTOR('',#13417,0.5);
#3700=VECTOR('',#13430,0.21);
#3701=VECTOR('',#13437,0.5);
#3702=VECTOR('',#13450,0.210000000000001);
#3703=VECTOR('',#13457,0.5);
#3704=VECTOR('',#13470,0.210000000000001);
#3705=VECTOR('',#13477,0.5);
#3706=VECTOR('',#13490,0.225);
#3707=VECTOR('',#13497,0.225);
#3708=VECTOR('',#13504,0.225);
#3709=VECTOR('',#13511,1.59);
#3710=VECTOR('',#13520,1.2);
#3711=VECTOR('',#13527,2.2);
#3712=VECTOR('',#13540,0.225);
#3713=VECTOR('',#13547,0.225);
#3714=VECTOR('',#13554,0.225);
#3715=VECTOR('',#13561,2.34);
#3716=VECTOR('',#13570,1.8);
#3717=VECTOR('',#13577,3.);
#3718=VECTOR('',#13590,0.225);
#3719=VECTOR('',#13597,0.225);
#3720=VECTOR('',#13604,0.225);
#3721=VECTOR('',#13611,1.59);
#3722=VECTOR('',#13622,1.2);
#3723=VECTOR('',#13627,2.2);
#3724=VECTOR('',#13640,0.225);
#3725=VECTOR('',#13647,0.225);
#3726=VECTOR('',#13654,0.225);
#3727=VECTOR('',#13661,2.34);
#3728=VECTOR('',#13672,1.8);
#3729=VECTOR('',#13677,3.);
#3730=VECTOR('',#13694,0.4);
#3731=VECTOR('',#13699,0.425);
#3732=VECTOR('',#13704,0.41);
#3733=VECTOR('',#13713,0.26);
#3734=VECTOR('',#13718,0.25);
#3735=VECTOR('',#13723,0.225);
#3736=VECTOR('',#13728,1.);
#3737=VECTOR('',#13729,1.);
#3738=VECTOR('',#13730,1.);
#3739=VECTOR('',#13731,1.);
#3740=VECTOR('',#13734,1.);
#3741=VECTOR('',#13735,1.);
#3742=VECTOR('',#13736,1.);
#3743=VECTOR('',#13739,1.);
#3744=VECTOR('',#13740,1.);
#3745=VECTOR('',#13741,1.);
#3746=VECTOR('',#13744,1.);
#3747=VECTOR('',#13745,1.);
#3748=VECTOR('',#13746,1.);
#3749=VECTOR('',#13749,1.);
#3750=VECTOR('',#13750,1.);
#3751=VECTOR('',#13751,1.);
#3752=VECTOR('',#13754,1.);
#3753=VECTOR('',#13755,1.);
#3754=VECTOR('',#13770,0.475);
#3755=VECTOR('',#13775,0.5);
#3756=VECTOR('',#13780,0.485);
#3757=VECTOR('',#13789,0.31);
#3758=VECTOR('',#13794,0.3);
#3759=VECTOR('',#13799,0.27);
#3760=VECTOR('',#13804,1.);
#3761=VECTOR('',#13805,1.);
#3762=VECTOR('',#13806,1.);
#3763=VECTOR('',#13807,1.);
#3764=VECTOR('',#13810,1.);
#3765=VECTOR('',#13811,1.);
#3766=VECTOR('',#13812,1.);
#3767=VECTOR('',#13815,1.);
#3768=VECTOR('',#13816,1.);
#3769=VECTOR('',#13817,1.);
#3770=VECTOR('',#13820,1.);
#3771=VECTOR('',#13821,1.);
#3772=VECTOR('',#13822,1.);
#3773=VECTOR('',#13825,1.);
#3774=VECTOR('',#13826,1.);
#3775=VECTOR('',#13827,1.);
#3776=VECTOR('',#13830,1.);
#3777=VECTOR('',#13831,1.);
#3778=VECTOR('',#13854,1.070235);
#3779=VECTOR('',#13861,0.6);
#3780=VECTOR('',#13866,0.63);
#3781=VECTOR('',#13875,1.070235);
#3782=VECTOR('',#13882,0.63);
#3783=VECTOR('',#13901,1.129765);
#3784=VECTOR('',#13912,1.57);
#3785=VECTOR('',#13917,1.6);
#3786=VECTOR('',#13922,1.57);
#3787=VECTOR('',#13927,1.129765);
#3788=VECTOR('',#13974,1.123812);
#3789=VECTOR('',#14043,1.076188);
#3790=VECTOR('',#14072,1.119765);
#3791=VECTOR('',#14079,1.085235);
#3792=VECTOR('',#14090,1.119765);
#3793=VECTOR('',#14097,1.085235);
#3794=VECTOR('',#14126,1.63531);
#3795=VECTOR('',#14133,1.);
#3796=VECTOR('',#14138,1.05);
#3797=VECTOR('',#14147,1.63531);
#3798=VECTOR('',#14154,1.05);
#3799=VECTOR('',#14173,1.71469);
#3800=VECTOR('',#14184,2.3);
#3801=VECTOR('',#14189,2.35);
#3802=VECTOR('',#14194,2.3);
#3803=VECTOR('',#14199,1.71469);
#3804=VECTOR('',#14250,1.706752);
#3805=VECTOR('',#14327,1.643248);
#3806=VECTOR('',#14356,1.70469);
#3807=VECTOR('',#14363,1.65031);
#3808=VECTOR('',#14374,1.70469);
#3809=VECTOR('',#14381,1.65031);
#3810=VECTOR('',#14402,0.325);
#3811=VECTOR('',#14407,0.35);
#3812=VECTOR('',#14412,0.335);
#3813=VECTOR('',#14421,0.21);
#3814=VECTOR('',#14426,0.2);
#3815=VECTOR('',#14431,0.18);
#3816=VECTOR('',#14436,1.);
#3817=VECTOR('',#14437,1.);
#3818=VECTOR('',#14438,1.);
#3819=VECTOR('',#14439,1.);
#3820=VECTOR('',#14442,1.);
#3821=VECTOR('',#14443,1.);
#3822=VECTOR('',#14444,1.);
#3823=VECTOR('',#14447,1.);
#3824=VECTOR('',#14448,1.);
#3825=VECTOR('',#14449,1.);
#3826=VECTOR('',#14452,1.);
#3827=VECTOR('',#14453,1.);
#3828=VECTOR('',#14454,1.);
#3829=VECTOR('',#14457,1.);
#3830=VECTOR('',#14458,1.);
#3831=VECTOR('',#14459,1.);
#3832=VECTOR('',#14462,1.);
#3833=VECTOR('',#14463,1.);
#3834=VECTOR('',#14552,1.);
#3835=VECTOR('',#14553,1.);
#3836=VECTOR('',#14554,1.);
#3837=VECTOR('',#14555,1.);
#3838=VECTOR('',#14560,1.);
#3839=VECTOR('',#14561,1.);
#3840=VECTOR('',#14564,1.);
#3841=VECTOR('',#14565,1.);
#3842=VECTOR('',#14566,1.);
#3843=VECTOR('',#14569,1.);
#3844=VECTOR('',#14578,0.6);
#3845=VECTOR('',#14591,0.61);
#3846=VECTOR('',#14598,0.9);
#3847=VECTOR('',#14611,0.61);
#3848=VECTOR('',#14618,0.9);
#3849=VECTOR('',#14629,1.);
#3850=VECTOR('',#14636,0.21);
#3851=VECTOR('',#14641,1.);
#3852=VECTOR('',#14646,0.605);
#3853=VECTOR('',#14653,1.1);
#3854=VECTOR('',#14666,0.61);
#3855=VECTOR('',#14673,0.9);
#3856=VECTOR('',#14684,1.);
#3857=VECTOR('',#14691,0.21);
#3858=VECTOR('',#14696,1.);
#3859=VECTOR('',#14701,0.605);
#3860=VECTOR('',#14708,1.1);
#3861=VECTOR('',#14721,0.61);
#3862=VECTOR('',#14728,0.9);
#3863=VECTOR('',#14739,1.);
#3864=VECTOR('',#14740,1.);
#3865=VECTOR('',#14741,1.);
#3866=VECTOR('',#14742,1.);
#3867=VECTOR('',#14745,1.);
#3868=VECTOR('',#14746,1.);
#3869=VECTOR('',#14747,1.);
#3870=VECTOR('',#14750,1.);
#3871=VECTOR('',#14751,1.);
#3872=VECTOR('',#14752,1.);
#3873=VECTOR('',#14757,1.);
#3874=VECTOR('',#14760,1.);
#3875=VECTOR('',#14763,1.);
#3876=VECTOR('',#14766,1.);
#3877=VECTOR('',#14769,1.);
#3878=VECTOR('',#14772,1.);
#3879=VECTOR('',#14775,1.);
#3880=VECTOR('',#14778,1.);
#3881=VECTOR('',#14781,1.);
#3882=VECTOR('',#14784,1.);
#3883=VECTOR('',#14787,1.);
#3884=VECTOR('',#14790,1.);
#3885=VECTOR('',#14793,1.);
#3886=VECTOR('',#14796,1.);
#3887=VECTOR('',#14799,1.);
#3888=VECTOR('',#14802,1.);
#3889=VECTOR('',#14805,1.);
#3890=VECTOR('',#14808,1.);
#3891=VECTOR('',#14811,1.);
#3892=VECTOR('',#14814,1.);
#3893=VECTOR('',#14825,1.4);
#3894=VECTOR('',#14830,1.);
#3895=VECTOR('',#14831,1.);
#3896=VECTOR('',#14834,1.);
#3897=VECTOR('',#14835,1.);
#3898=VECTOR('',#14836,1.);
#3899=VECTOR('',#14841,1.);
#3900=VECTOR('',#14842,1.);
#3901=VECTOR('',#14845,1.);
#3902=VECTOR('',#14846,1.);
#3903=VECTOR('',#14847,1.);
#3904=VECTOR('',#14852,1.);
#3905=VECTOR('',#14853,1.);
#3906=VECTOR('',#14856,1.);
#3907=VECTOR('',#14857,1.);
#3908=VECTOR('',#14858,1.);
#3909=VECTOR('',#14863,1.);
#3910=VECTOR('',#14864,1.);
#3911=VECTOR('',#14867,1.);
#3912=VECTOR('',#14868,1.);
#3913=VECTOR('',#14869,1.);
#3914=VECTOR('',#14874,1.);
#3915=VECTOR('',#14875,1.);
#3916=VECTOR('',#14878,1.);
#3917=VECTOR('',#14879,1.);
#3918=VECTOR('',#14880,1.);
#3919=VECTOR('',#14885,1.);
#3920=VECTOR('',#14886,1.);
#3921=VECTOR('',#14889,1.);
#3922=VECTOR('',#14890,1.);
#3923=VECTOR('',#14891,1.);
#3924=VECTOR('',#14896,1.);
#3925=VECTOR('',#14897,1.);
#3926=VECTOR('',#14900,1.);
#3927=VECTOR('',#14901,1.);
#3928=VECTOR('',#14902,1.);
#3929=VECTOR('',#14907,1.);
#3930=VECTOR('',#14908,1.);
#3931=VECTOR('',#14911,1.);
#3932=VECTOR('',#14912,1.);
#3933=VECTOR('',#14913,1.);
#3934=VECTOR('',#14918,1.);
#3935=VECTOR('',#14919,1.);
#3936=VECTOR('',#14922,1.);
#3937=VECTOR('',#14923,1.);
#3938=VECTOR('',#14924,1.);
#3939=VECTOR('',#14929,1.);
#3940=VECTOR('',#14930,1.);
#3941=VECTOR('',#14933,1.);
#3942=VECTOR('',#14934,1.);
#3943=VECTOR('',#14935,1.);
#3944=VECTOR('',#14940,1.);
#3945=VECTOR('',#14941,1.);
#3946=VECTOR('',#14944,1.);
#3947=VECTOR('',#14945,1.);
#3948=VECTOR('',#14946,1.);
#3949=VECTOR('',#14951,1.);
#3950=VECTOR('',#14952,1.);
#3951=VECTOR('',#14955,1.);
#3952=VECTOR('',#14956,1.);
#3953=VECTOR('',#14957,1.);
#3954=VECTOR('',#14962,1.);
#3955=VECTOR('',#14963,1.);
#3956=VECTOR('',#14966,1.);
#3957=VECTOR('',#14967,1.);
#3958=VECTOR('',#14968,1.);
#3959=VECTOR('',#14973,1.);
#3960=VECTOR('',#14974,1.);
#3961=VECTOR('',#14977,1.);
#3962=VECTOR('',#14978,1.);
#3963=VECTOR('',#14979,1.);
#3964=VECTOR('',#14984,1.);
#3965=VECTOR('',#14985,1.);
#3966=VECTOR('',#14988,1.);
#3967=VECTOR('',#14989,1.);
#3968=VECTOR('',#14990,1.);
#3969=VECTOR('',#14995,1.);
#3970=VECTOR('',#14996,1.);
#3971=VECTOR('',#14999,1.);
#3972=VECTOR('',#15000,1.);
#3973=VECTOR('',#15001,1.);
#3974=VECTOR('',#15006,1.);
#3975=VECTOR('',#15007,1.);
#3976=VECTOR('',#15010,1.);
#3977=VECTOR('',#15011,1.);
#3978=VECTOR('',#15012,1.);
#3979=VECTOR('',#15017,1.);
#3980=VECTOR('',#15018,1.);
#3981=VECTOR('',#15021,1.);
#3982=VECTOR('',#15022,1.);
#3983=VECTOR('',#15023,1.);
#3984=VECTOR('',#15028,1.);
#3985=VECTOR('',#15029,1.);
#3986=VECTOR('',#15032,1.);
#3987=VECTOR('',#15033,1.);
#3988=VECTOR('',#15034,1.);
#3989=VECTOR('',#15039,1.);
#3990=VECTOR('',#15040,1.);
#3991=VECTOR('',#15043,1.);
#3992=VECTOR('',#15044,1.);
#3993=VECTOR('',#15045,1.);
#3994=VECTOR('',#15056,1.);
#3995=VECTOR('',#15057,1.);
#3996=VECTOR('',#15058,1.);
#3997=VECTOR('',#15059,1.);
#3998=VECTOR('',#15062,1.);
#3999=VECTOR('',#15069,1.);
#4000=VECTOR('',#15070,1.);
#4001=VECTOR('',#15071,1.);
#4002=VECTOR('',#15080,1.);
#4003=VECTOR('',#15083,1.);
#4004=VECTOR('',#15086,1.);
#4005=VECTOR('',#15087,1.);
#4006=VECTOR('',#15092,1.);
#4007=VECTOR('',#15093,1.);
#4008=VECTOR('',#15094,1.);
#4009=VECTOR('',#15097,1.);
#4010=VECTOR('',#15102,1.);
#4011=VECTOR('',#15103,1.);
#4012=VECTOR('',#15104,1.);
#4013=VECTOR('',#15113,1.);
#4014=VECTOR('',#15124,1.);
#4015=VECTOR('',#15125,1.);
#4016=VECTOR('',#15126,1.);
#4017=VECTOR('',#15127,1.);
#4018=VECTOR('',#15132,1.);
#4019=VECTOR('',#15133,1.);
#4020=VECTOR('',#15136,1.);
#4021=VECTOR('',#15137,1.);
#4022=VECTOR('',#15138,1.);
#4023=VECTOR('',#15141,1.);
#4024=VECTOR('',#15150,1.);
#4025=VECTOR('',#15163,1.01);
#4026=VECTOR('',#15170,1.35);
#4027=VECTOR('',#15183,1.01);
#4028=VECTOR('',#15190,1.35);
#4029=VECTOR('',#15201,1.);
#4030=VECTOR('',#15208,0.21);
#4031=VECTOR('',#15213,1.);
#4032=VECTOR('',#15218,1.005);
#4033=VECTOR('',#15225,1.6);
#4034=VECTOR('',#15238,1.01);
#4035=VECTOR('',#15245,1.35);
#4036=VECTOR('',#15256,1.);
#4037=VECTOR('',#15263,0.21);
#4038=VECTOR('',#15268,1.);
#4039=VECTOR('',#15273,1.005);
#4040=VECTOR('',#15280,1.6);
#4041=VECTOR('',#15293,1.01);
#4042=VECTOR('',#15300,1.35);
#4043=VECTOR('',#15311,1.);
#4044=VECTOR('',#15312,1.);
#4045=VECTOR('',#15313,1.);
#4046=VECTOR('',#15314,1.);
#4047=VECTOR('',#15317,1.);
#4048=VECTOR('',#15318,1.);
#4049=VECTOR('',#15319,1.);
#4050=VECTOR('',#15322,1.);
#4051=VECTOR('',#15323,1.);
#4052=VECTOR('',#15324,1.);
#4053=VECTOR('',#15329,1.);
#4054=VECTOR('',#15332,1.);
#4055=VECTOR('',#15335,1.);
#4056=VECTOR('',#15338,1.);
#4057=VECTOR('',#15341,1.);
#4058=VECTOR('',#15344,1.);
#4059=VECTOR('',#15347,1.);
#4060=VECTOR('',#15350,1.);
#4061=VECTOR('',#15353,1.);
#4062=VECTOR('',#15356,1.);
#4063=VECTOR('',#15359,1.);
#4064=VECTOR('',#15362,1.);
#4065=VECTOR('',#15365,1.);
#4066=VECTOR('',#15368,1.);
#4067=VECTOR('',#15371,1.);
#4068=VECTOR('',#15374,1.);
#4069=VECTOR('',#15377,1.);
#4070=VECTOR('',#15380,1.);
#4071=VECTOR('',#15383,1.);
#4072=VECTOR('',#15386,1.);
#4073=VECTOR('',#15389,1.);
#4074=VECTOR('',#15392,1.);
#4075=VECTOR('',#15395,1.);
#4076=VECTOR('',#15398,1.);
#4077=VECTOR('',#15401,1.);
#4078=VECTOR('',#15404,1.);
#4079=VECTOR('',#15407,1.);
#4080=VECTOR('',#15410,1.);
#4081=VECTOR('',#15413,1.);
#4082=VECTOR('',#15416,1.);
#4083=VECTOR('',#15419,1.);
#4084=VECTOR('',#15422,1.);
#4085=VECTOR('',#15425,1.);
#4086=VECTOR('',#15428,1.);
#4087=VECTOR('',#15431,1.);
#4088=VECTOR('',#15434,1.);
#4089=VECTOR('',#15437,1.);
#4090=VECTOR('',#15440,1.);
#4091=VECTOR('',#15443,1.);
#4092=VECTOR('',#15446,1.);
#4093=VECTOR('',#15457,2.);
#4094=VECTOR('',#15462,1.);
#4095=VECTOR('',#15463,1.);
#4096=VECTOR('',#15466,1.);
#4097=VECTOR('',#15471,1.);
#4098=VECTOR('',#15472,1.);
#4099=VECTOR('',#15475,1.);
#4100=VECTOR('',#15480,1.);
#4101=VECTOR('',#15481,1.);
#4102=VECTOR('',#15484,1.);
#4103=VECTOR('',#15489,1.);
#4104=VECTOR('',#15490,1.);
#4105=VECTOR('',#15493,1.);
#4106=VECTOR('',#15498,1.);
#4107=VECTOR('',#15499,1.);
#4108=VECTOR('',#15502,1.);
#4109=VECTOR('',#15507,1.);
#4110=VECTOR('',#15508,1.);
#4111=VECTOR('',#15511,1.);
#4112=VECTOR('',#15516,1.);
#4113=VECTOR('',#15517,1.);
#4114=VECTOR('',#15520,1.);
#4115=VECTOR('',#15525,1.);
#4116=VECTOR('',#15526,1.);
#4117=VECTOR('',#15529,1.);
#4118=VECTOR('',#15534,1.);
#4119=VECTOR('',#15535,1.);
#4120=VECTOR('',#15538,1.);
#4121=VECTOR('',#15543,1.);
#4122=VECTOR('',#15544,1.);
#4123=VECTOR('',#15547,1.);
#4124=VECTOR('',#15552,1.);
#4125=VECTOR('',#15553,1.);
#4126=VECTOR('',#15556,1.);
#4127=VECTOR('',#15561,1.);
#4128=VECTOR('',#15562,1.);
#4129=VECTOR('',#15565,1.);
#4130=VECTOR('',#15570,1.);
#4131=VECTOR('',#15571,1.);
#4132=VECTOR('',#15574,1.);
#4133=VECTOR('',#15579,1.);
#4134=VECTOR('',#15580,1.);
#4135=VECTOR('',#15583,1.);
#4136=VECTOR('',#15588,1.);
#4137=VECTOR('',#15589,1.);
#4138=VECTOR('',#15592,1.);
#4139=VECTOR('',#15597,1.);
#4140=VECTOR('',#15598,1.);
#4141=VECTOR('',#15601,1.);
#4142=VECTOR('',#15606,1.);
#4143=VECTOR('',#15607,1.);
#4144=VECTOR('',#15610,1.);
#4145=VECTOR('',#15615,1.);
#4146=VECTOR('',#15616,1.);
#4147=VECTOR('',#15619,1.);
#4148=VECTOR('',#15624,1.);
#4149=VECTOR('',#15625,1.);
#4150=VECTOR('',#15628,1.);
#4151=VECTOR('',#15633,1.);
#4152=VECTOR('',#15634,1.);
#4153=VECTOR('',#15637,1.);
#4154=VECTOR('',#15642,1.);
#4155=VECTOR('',#15643,1.);
#4156=VECTOR('',#15646,1.);
#4157=VECTOR('',#15651,1.);
#4158=VECTOR('',#15652,1.);
#4159=VECTOR('',#15655,1.);
#4160=VECTOR('',#15660,1.);
#4161=VECTOR('',#15661,1.);
#4162=VECTOR('',#15664,1.);
#4163=VECTOR('',#15669,1.);
#4164=VECTOR('',#15670,1.);
#4165=VECTOR('',#15673,1.);
#4166=VECTOR('',#15678,1.);
#4167=VECTOR('',#15679,1.);
#4168=VECTOR('',#15682,1.);
#4169=VECTOR('',#15687,1.);
#4170=VECTOR('',#15688,1.);
#4171=VECTOR('',#15691,1.);
#4172=VECTOR('',#15696,1.);
#4173=VECTOR('',#15697,1.);
#4174=VECTOR('',#15700,1.);
#4175=VECTOR('',#15705,1.);
#4176=VECTOR('',#15706,1.);
#4177=VECTOR('',#15709,1.);
#4178=VECTOR('',#15714,1.);
#4179=VECTOR('',#15715,1.);
#4180=VECTOR('',#15718,1.);
#4181=VECTOR('',#15723,1.);
#4182=VECTOR('',#15724,1.);
#4183=VECTOR('',#15727,1.);
#4184=VECTOR('',#15732,1.);
#4185=VECTOR('',#15733,1.);
#4186=VECTOR('',#15736,1.);
#4187=VECTOR('',#15741,1.);
#4188=VECTOR('',#15742,1.);
#4189=VECTOR('',#15745,1.);
#4190=VECTOR('',#15750,1.);
#4191=VECTOR('',#15751,1.);
#4192=VECTOR('',#15754,1.);
#4193=VECTOR('',#15759,1.);
#4194=VECTOR('',#15760,1.);
#4195=VECTOR('',#15763,1.);
#4196=VECTOR('',#15768,1.);
#4197=VECTOR('',#15769,1.);
#4198=VECTOR('',#15772,1.);
#4199=VECTOR('',#15777,1.);
#4200=VECTOR('',#15778,1.);
#4201=VECTOR('',#15781,1.);
#4202=VECTOR('',#15786,1.);
#4203=VECTOR('',#15787,1.);
#4204=VECTOR('',#15790,1.);
#4205=VECTOR('',#15795,1.);
#4206=VECTOR('',#15796,1.);
#4207=VECTOR('',#15799,1.);
#4208=VECTOR('',#15804,1.);
#4209=VECTOR('',#15807,1.);
#4210=VECTOR('',#15808,1.);
#4211=VECTOR('',#15813,1.);
#4212=VECTOR('',#15814,1.);
#4213=VECTOR('',#15817,1.);
#4214=VECTOR('',#15828,1.);
#4215=VECTOR('',#15829,1.);
#4216=VECTOR('',#15830,1.);
#4217=VECTOR('',#15831,1.);
#4218=VECTOR('',#15832,1.);
#4219=VECTOR('',#15833,1.);
#4220=VECTOR('',#15834,1.);
#4221=VECTOR('',#15835,1.);
#4222=VECTOR('',#15838,1.);
#4223=VECTOR('',#15839,1.);
#4224=VECTOR('',#15840,1.);
#4225=VECTOR('',#15843,1.);
#4226=VECTOR('',#15844,1.);
#4227=VECTOR('',#15847,1.);
#4228=VECTOR('',#15848,1.);
#4229=VECTOR('',#15851,1.);
#4230=VECTOR('',#15852,1.);
#4231=VECTOR('',#15855,1.);
#4232=VECTOR('',#15856,1.);
#4233=VECTOR('',#15857,1.);
#4234=VECTOR('',#15858,1.);
#4235=VECTOR('',#15861,1.);
#4236=VECTOR('',#15864,1.);
#4237=VECTOR('',#15867,1.);
#4238=VECTOR('',#15874,1.);
#4239=VECTOR('',#15875,1.);
#4240=VECTOR('',#15876,1.);
#4241=VECTOR('',#15877,1.);
#4242=VECTOR('',#15880,1.);
#4243=VECTOR('',#15881,1.);
#4244=VECTOR('',#15882,1.);
#4245=VECTOR('',#15885,1.);
#4246=VECTOR('',#15886,1.);
#4247=VECTOR('',#15887,1.);
#4248=VECTOR('',#15890,1.);
#4249=VECTOR('',#15891,1.);
#4250=VECTOR('',#15892,1.);
#4251=VECTOR('',#15895,1.);
#4252=VECTOR('',#15896,1.);
#4253=VECTOR('',#15897,1.);
#4254=VECTOR('',#15900,1.);
#4255=VECTOR('',#15901,1.);
#4256=VECTOR('',#15912,0.235);
#4257=VECTOR('',#15917,0.25);
#4258=VECTOR('',#15922,0.2125);
#4259=CIRCLE('',#11810,0.33);
#4260=CIRCLE('',#11811,0.33);
#4261=CIRCLE('',#11813,0.33);
#4262=CIRCLE('',#11814,0.33);
#4263=CIRCLE('',#11816,0.33);
#4264=CIRCLE('',#11817,0.33);
#4265=CIRCLE('',#11819,0.33);
#4266=CIRCLE('',#11820,0.33);
#4267=CIRCLE('',#11829,0.165);
#4268=CIRCLE('',#11830,0.165);
#4269=CIRCLE('',#11832,0.165);
#4270=CIRCLE('',#11833,0.165);
#4271=CIRCLE('',#11835,0.164999999999999);
#4272=CIRCLE('',#11836,0.164999999999999);
#4273=CIRCLE('',#11838,0.165);
#4274=CIRCLE('',#11839,0.165);
#4275=CIRCLE('',#11841,0.165);
#4276=CIRCLE('',#11842,0.165);
#4277=CIRCLE('',#11844,0.165);
#4278=CIRCLE('',#11845,0.165);
#4279=CIRCLE('',#11847,0.475);
#4280=CIRCLE('',#11848,0.475);
#4281=CIRCLE('',#11850,0.275);
#4282=CIRCLE('',#11852,0.475);
#4283=CIRCLE('',#11853,0.475);
#4284=CIRCLE('',#11855,0.275);
#4285=CIRCLE('',#11857,0.475);
#4286=CIRCLE('',#11858,0.475);
#4287=CIRCLE('',#11860,0.275);
#4288=CIRCLE('',#11862,0.475);
#4289=CIRCLE('',#11863,0.475);
#4290=CIRCLE('',#11865,0.275);
#4291=CIRCLE('',#11867,0.275);
#4292=CIRCLE('',#11869,0.275);
#4293=CIRCLE('',#11871,0.275);
#4294=CIRCLE('',#11873,0.275);
#4295=CIRCLE('',#11875,0.25);
#4296=CIRCLE('',#11876,0.25);
#4297=CIRCLE('',#11879,0.25);
#4298=CIRCLE('',#11880,0.25);
#4299=CIRCLE('',#11883,2.35);
#4300=CIRCLE('',#11884,2.35);
#4301=CIRCLE('',#11886,2.15);
#4302=CIRCLE('',#11888,2.15);
#4303=CIRCLE('',#11890,1.6);
#4304=CIRCLE('',#11891,1.6);
#4305=CIRCLE('',#11893,1.4);
#4306=CIRCLE('',#11895,1.4);
#4307=CIRCLE('',#11904,0.165);
#4308=CIRCLE('',#11905,0.165);
#4309=CIRCLE('',#11907,0.165);
#4310=CIRCLE('',#11908,0.165);
#4311=CIRCLE('',#11910,0.164999999999999);
#4312=CIRCLE('',#11911,0.164999999999999);
#4313=CIRCLE('',#11913,0.165);
#4314=CIRCLE('',#11914,0.165);
#4315=CIRCLE('',#11916,0.165);
#4316=CIRCLE('',#11917,0.165);
#4317=CIRCLE('',#11919,0.165);
#4318=CIRCLE('',#11920,0.165);
#4319=CIRCLE('',#11922,0.475);
#4320=CIRCLE('',#11923,0.475);
#4321=CIRCLE('',#11925,0.275);
#4322=CIRCLE('',#11927,0.475);
#4323=CIRCLE('',#11928,0.475);
#4324=CIRCLE('',#11930,0.275);
#4325=CIRCLE('',#11932,0.475);
#4326=CIRCLE('',#11933,0.475);
#4327=CIRCLE('',#11935,0.275);
#4328=CIRCLE('',#11937,0.475);
#4329=CIRCLE('',#11938,0.475);
#4330=CIRCLE('',#11940,0.275);
#4331=CIRCLE('',#11942,0.275);
#4332=CIRCLE('',#11944,0.275);
#4333=CIRCLE('',#11946,0.275);
#4334=CIRCLE('',#11948,0.275);
#4335=CIRCLE('',#11950,0.25);
#4336=CIRCLE('',#11951,0.25);
#4337=CIRCLE('',#11954,0.25);
#4338=CIRCLE('',#11955,0.25);
#4339=CIRCLE('',#11958,2.35);
#4340=CIRCLE('',#11959,2.35);
#4341=CIRCLE('',#11961,2.15);
#4342=CIRCLE('',#11963,2.15);
#4343=CIRCLE('',#11965,1.6);
#4344=CIRCLE('',#11966,1.6);
#4345=CIRCLE('',#11968,1.4);
#4346=CIRCLE('',#11970,1.4);
#4347=CIRCLE('',#11979,0.21);
#4348=CIRCLE('',#11980,0.21);
#4349=CIRCLE('',#11982,0.5);
#4350=CIRCLE('',#11983,0.5);
#4351=CIRCLE('',#11988,0.21);
#4352=CIRCLE('',#11989,0.21);
#4353=CIRCLE('',#11991,0.5);
#4354=CIRCLE('',#11992,0.5);
#4355=CIRCLE('',#11997,0.210000000000001);
#4356=CIRCLE('',#11998,0.210000000000001);
#4357=CIRCLE('',#12000,0.5);
#4358=CIRCLE('',#12001,0.5);
#4359=CIRCLE('',#12006,0.210000000000001);
#4360=CIRCLE('',#12007,0.210000000000001);
#4361=CIRCLE('',#12009,0.5);
#4362=CIRCLE('',#12010,0.5);
#4363=CIRCLE('',#12015,0.225);
#4364=CIRCLE('',#12016,0.225);
#4365=CIRCLE('',#12018,0.225);
#4366=CIRCLE('',#12019,0.225);
#4367=CIRCLE('',#12021,0.225);
#4368=CIRCLE('',#12022,0.225);
#4369=CIRCLE('',#12024,1.59);
#4370=CIRCLE('',#12025,1.59);
#4371=CIRCLE('',#12027,1.2);
#4372=CIRCLE('',#12029,1.2);
#4373=CIRCLE('',#12031,2.2);
#4374=CIRCLE('',#12032,2.2);
#4375=CIRCLE('',#12037,0.225);
#4376=CIRCLE('',#12038,0.225);
#4377=CIRCLE('',#12040,0.225);
#4378=CIRCLE('',#12041,0.225);
#4379=CIRCLE('',#12043,0.225);
#4380=CIRCLE('',#12044,0.225);
#4381=CIRCLE('',#12046,2.34);
#4382=CIRCLE('',#12047,2.34);
#4383=CIRCLE('',#12049,1.8);
#4384=CIRCLE('',#12051,1.8);
#4385=CIRCLE('',#12053,3.);
#4386=CIRCLE('',#12054,3.);
#4387=CIRCLE('',#12059,0.225);
#4388=CIRCLE('',#12060,0.225);
#4389=CIRCLE('',#12062,0.225);
#4390=CIRCLE('',#12063,0.225);
#4391=CIRCLE('',#12065,0.225);
#4392=CIRCLE('',#12066,0.225);
#4393=CIRCLE('',#12068,1.59);
#4394=CIRCLE('',#12069,1.59);
#4395=CIRCLE('',#12071,1.2);
#4396=CIRCLE('',#12073,1.2);
#4397=CIRCLE('',#12075,2.2);
#4398=CIRCLE('',#12076,2.2);
#4399=CIRCLE('',#12081,0.225);
#4400=CIRCLE('',#12082,0.225);
#4401=CIRCLE('',#12084,0.225);
#4402=CIRCLE('',#12085,0.225);
#4403=CIRCLE('',#12087,0.225);
#4404=CIRCLE('',#12088,0.225);
#4405=CIRCLE('',#12090,2.34);
#4406=CIRCLE('',#12091,2.34);
#4407=CIRCLE('',#12093,1.8);
#4408=CIRCLE('',#12095,1.8);
#4409=CIRCLE('',#12097,3.);
#4410=CIRCLE('',#12098,3.);
#4411=CIRCLE('',#12103,0.375);
#4412=CIRCLE('',#12105,0.425);
#4413=CIRCLE('',#12107,0.425);
#4414=CIRCLE('',#12109,0.395);
#4415=CIRCLE('',#12111,0.27);
#4416=CIRCLE('',#12113,0.24505);
#4417=CIRCLE('',#12115,0.24505);
#4418=CIRCLE('',#12117,0.2);
#4419=CIRCLE('',#12129,0.45);
#4420=CIRCLE('',#12131,0.5);
#4421=CIRCLE('',#12133,0.5);
#4422=CIRCLE('',#12135,0.47);
#4423=CIRCLE('',#12137,0.32);
#4424=CIRCLE('',#12139,0.2942);
#4425=CIRCLE('',#12141,0.2942);
#4426=CIRCLE('',#12143,0.24);
#4427=CIRCLE('',#12156,1.070235);
#4428=CIRCLE('',#12157,1.070235);
#4429=CIRCLE('',#12158,0.309556);
#4430=CIRCLE('',#12159,1.070235);
#4431=CIRCLE('',#12160,1.070235);
#4432=CIRCLE('',#12162,1.070235);
#4433=CIRCLE('',#12164,0.6);
#4434=CIRCLE('',#12165,0.6);
#4435=CIRCLE('',#12167,0.66);
#4436=CIRCLE('',#12170,1.070235);
#4437=CIRCLE('',#12172,0.66);
#4438=CIRCLE('',#12176,1.129765);
#4439=CIRCLE('',#12177,1.129765);
#4440=CIRCLE('',#12178,0.309556);
#4441=CIRCLE('',#12179,1.129765);
#4442=CIRCLE('',#12180,1.129765);
#4443=CIRCLE('',#12182,1.129765);
#4444=CIRCLE('',#12184,1.54);
#4445=CIRCLE('',#12185,1.129765);
#4446=CIRCLE('',#12187,1.6);
#4447=CIRCLE('',#12189,1.6);
#4448=CIRCLE('',#12191,1.54);
#4449=CIRCLE('',#12196,0.29765);
#4450=CIRCLE('',#12198,0.29765);
#4451=CIRCLE('',#12200,0.29765);
#4452=CIRCLE('',#12202,0.29765);
#4453=CIRCLE('',#12204,0.29765);
#4454=CIRCLE('',#12206,0.29765);
#4455=CIRCLE('',#12208,0.29765);
#4456=CIRCLE('',#12211,0.303778037777585);
#4457=CIRCLE('',#12212,0.303778037777585);
#4458=CIRCLE('',#12214,1.123812);
#4459=CIRCLE('',#12215,1.123812);
#4460=CIRCLE('',#12216,1.123812);
#4461=CIRCLE('',#12217,1.123812);
#4462=CIRCLE('',#12218,1.123812);
#4463=CIRCLE('',#12219,1.123812);
#4464=CIRCLE('',#12220,1.123812);
#4465=CIRCLE('',#12221,1.123812);
#4466=CIRCLE('',#12222,1.123812);
#4467=CIRCLE('',#12224,1.076188);
#4468=CIRCLE('',#12225,0.303778037777585);
#4469=CIRCLE('',#12227,0.303778037777585);
#4470=CIRCLE('',#12229,1.076188);
#4471=CIRCLE('',#12230,0.303778037777585);
#4472=CIRCLE('',#12232,0.303778037777585);
#4473=CIRCLE('',#12234,1.076188);
#4474=CIRCLE('',#12235,1.076188);
#4475=CIRCLE('',#12236,0.303778037777585);
#4476=CIRCLE('',#12238,0.303778037777585);
#4477=CIRCLE('',#12240,1.076188);
#4478=CIRCLE('',#12241,0.303778037777585);
#4479=CIRCLE('',#12243,0.303778037777585);
#4480=CIRCLE('',#12245,1.076188);
#4481=CIRCLE('',#12246,0.303778037777585);
#4482=CIRCLE('',#12248,0.303778037777585);
#4483=CIRCLE('',#12250,1.076188);
#4484=CIRCLE('',#12251,1.076188);
#4485=CIRCLE('',#12252,1.076188);
#4486=CIRCLE('',#12254,0.303778037777585);
#4487=CIRCLE('',#12256,0.303778037777585);
#4488=CIRCLE('',#12261,1.119765);
#4489=CIRCLE('',#12262,1.085235);
#4490=CIRCLE('',#12264,1.119765);
#4491=CIRCLE('',#12266,1.085235);
#4492=CIRCLE('',#12269,1.119765);
#4493=CIRCLE('',#12270,1.085235);
#4494=CIRCLE('',#12272,1.119765);
#4495=CIRCLE('',#12274,1.085235);
#4496=CIRCLE('',#12284,1.63531);
#4497=CIRCLE('',#12285,1.63531);
#4498=CIRCLE('',#12286,0.412776);
#4499=CIRCLE('',#12287,1.63531);
#4500=CIRCLE('',#12288,1.63531);
#4501=CIRCLE('',#12290,1.63531);
#4502=CIRCLE('',#12292,1.);
#4503=CIRCLE('',#12293,1.);
#4504=CIRCLE('',#12295,1.1);
#4505=CIRCLE('',#12298,1.63531);
#4506=CIRCLE('',#12300,1.1);
#4507=CIRCLE('',#12304,1.71469);
#4508=CIRCLE('',#12305,1.71469);
#4509=CIRCLE('',#12306,0.412776);
#4510=CIRCLE('',#12307,1.71469);
#4511=CIRCLE('',#12308,1.71469);
#4512=CIRCLE('',#12310,1.71469);
#4513=CIRCLE('',#12312,2.25);
#4514=CIRCLE('',#12313,1.71469);
#4515=CIRCLE('',#12315,2.35);
#4516=CIRCLE('',#12317,2.35);
#4517=CIRCLE('',#12319,2.25);
#4518=CIRCLE('',#12324,0.3969);
#4519=CIRCLE('',#12326,0.3969);
#4520=CIRCLE('',#12328,0.3969);
#4521=CIRCLE('',#12330,0.3969);
#4522=CIRCLE('',#12332,0.3969);
#4523=CIRCLE('',#12334,0.3969);
#4524=CIRCLE('',#12336,0.3969);
#4525=CIRCLE('',#12338,0.3969);
#4526=CIRCLE('',#12341,0.405071403305639);
#4527=CIRCLE('',#12342,0.405071403305639);
#4528=CIRCLE('',#12344,1.706752);
#4529=CIRCLE('',#12345,1.706752);
#4530=CIRCLE('',#12346,1.706752);
#4531=CIRCLE('',#12347,1.706752);
#4532=CIRCLE('',#12348,1.706752);
#4533=CIRCLE('',#12349,1.706752);
#4534=CIRCLE('',#12350,1.706752);
#4535=CIRCLE('',#12351,1.706752);
#4536=CIRCLE('',#12352,1.706752);
#4537=CIRCLE('',#12354,1.643248);
#4538=CIRCLE('',#12355,0.405071403305639);
#4539=CIRCLE('',#12357,0.405071403305639);
#4540=CIRCLE('',#12359,1.643248);
#4541=CIRCLE('',#12360,0.405071403305639);
#4542=CIRCLE('',#12362,0.405071403305639);
#4543=CIRCLE('',#12364,1.643248);
#4544=CIRCLE('',#12365,0.405071403305639);
#4545=CIRCLE('',#12367,0.405071403305639);
#4546=CIRCLE('',#12369,1.643248);
#4547=CIRCLE('',#12370,0.405071403305639);
#4548=CIRCLE('',#12372,0.405071403305639);
#4549=CIRCLE('',#12374,1.643248);
#4550=CIRCLE('',#12375,0.405071403305639);
#4551=CIRCLE('',#12377,0.405071403305639);
#4552=CIRCLE('',#12379,1.643248);
#4553=CIRCLE('',#12380,0.405071403305639);
#4554=CIRCLE('',#12382,0.405071403305639);
#4555=CIRCLE('',#12384,1.643248);
#4556=CIRCLE('',#12385,1.643248);
#4557=CIRCLE('',#12386,1.643248);
#4558=CIRCLE('',#12388,0.405071403305639);
#4559=CIRCLE('',#12390,0.405071403305639);
#4560=CIRCLE('',#12395,1.70469);
#4561=CIRCLE('',#12396,1.65031);
#4562=CIRCLE('',#12398,1.70469);
#4563=CIRCLE('',#12400,1.65031);
#4564=CIRCLE('',#12403,1.70469);
#4565=CIRCLE('',#12404,1.65031);
#4566=CIRCLE('',#12406,1.70469);
#4567=CIRCLE('',#12408,1.65031);
#4568=CIRCLE('',#12417,0.3);
#4569=CIRCLE('',#12419,0.35);
#4570=CIRCLE('',#12421,0.35);
#4571=CIRCLE('',#12423,0.32);
#4572=CIRCLE('',#12425,0.22);
#4573=CIRCLE('',#12427,0.1954);
#4574=CIRCLE('',#12429,0.1954);
#4575=CIRCLE('',#12431,0.16);
#4576=CIRCLE('',#12484,0.6);
#4577=CIRCLE('',#12488,0.6);
#4578=CIRCLE('',#12490,0.6);
#4579=CIRCLE('',#12491,0.6);
#4580=CIRCLE('',#12496,0.61);
#4581=CIRCLE('',#12497,0.61);
#4582=CIRCLE('',#12499,0.9);
#4583=CIRCLE('',#12500,0.9);
#4584=CIRCLE('',#12505,0.61);
#4585=CIRCLE('',#12506,0.61);
#4586=CIRCLE('',#12508,0.9);
#4587=CIRCLE('',#12509,0.9);
#4588=CIRCLE('',#12514,0.21);
#4589=CIRCLE('',#12516,0.21);
#4590=CIRCLE('',#12517,0.21);
#4591=CIRCLE('',#12520,0.605);
#4592=CIRCLE('',#12521,0.605);
#4593=CIRCLE('',#12523,1.1);
#4594=CIRCLE('',#12524,1.1);
#4595=CIRCLE('',#12529,0.61);
#4596=CIRCLE('',#12530,0.61);
#4597=CIRCLE('',#12532,0.9);
#4598=CIRCLE('',#12533,0.9);
#4599=CIRCLE('',#12538,0.21);
#4600=CIRCLE('',#12540,0.21);
#4601=CIRCLE('',#12541,0.21);
#4602=CIRCLE('',#12544,0.605);
#4603=CIRCLE('',#12545,0.605);
#4604=CIRCLE('',#12547,1.1);
#4605=CIRCLE('',#12548,1.1);
#4606=CIRCLE('',#12553,0.61);
#4607=CIRCLE('',#12554,0.61);
#4608=CIRCLE('',#12556,0.9);
#4609=CIRCLE('',#12557,0.9);
#4610=CIRCLE('',#12565,1.75);
#4611=CIRCLE('',#12566,1.75);
#4612=CIRCLE('',#12567,1.75);
#4613=CIRCLE('',#12568,1.75);
#4614=CIRCLE('',#12569,1.75);
#4615=CIRCLE('',#12570,1.75);
#4616=CIRCLE('',#12571,1.75);
#4617=CIRCLE('',#12572,1.75);
#4618=CIRCLE('',#12573,1.75);
#4619=CIRCLE('',#12574,1.75);
#4620=CIRCLE('',#12575,1.75);
#4621=CIRCLE('',#12576,1.75);
#4622=CIRCLE('',#12577,1.75);
#4623=CIRCLE('',#12578,1.75);
#4624=CIRCLE('',#12579,1.75);
#4625=CIRCLE('',#12580,1.75);
#4626=CIRCLE('',#12581,1.75);
#4627=CIRCLE('',#12582,1.75);
#4628=CIRCLE('',#12583,1.75);
#4629=CIRCLE('',#12584,1.75);
#4630=CIRCLE('',#12585,0.6);
#4631=CIRCLE('',#12587,0.6);
#4632=CIRCLE('',#12589,1.4);
#4633=CIRCLE('',#12590,1.4);
#4634=CIRCLE('',#12594,1.75);
#4635=CIRCLE('',#12597,1.75);
#4636=CIRCLE('',#12600,1.75);
#4637=CIRCLE('',#12603,1.75);
#4638=CIRCLE('',#12606,1.75);
#4639=CIRCLE('',#12609,1.75);
#4640=CIRCLE('',#12612,1.75);
#4641=CIRCLE('',#12615,1.75);
#4642=CIRCLE('',#12618,1.75);
#4643=CIRCLE('',#12621,1.75);
#4644=CIRCLE('',#12624,1.75);
#4645=CIRCLE('',#12627,1.75);
#4646=CIRCLE('',#12630,1.75);
#4647=CIRCLE('',#12633,1.75);
#4648=CIRCLE('',#12636,1.75);
#4649=CIRCLE('',#12639,1.75);
#4650=CIRCLE('',#12642,1.75);
#4651=CIRCLE('',#12645,1.75);
#4652=CIRCLE('',#12648,1.75);
#4653=CIRCLE('',#12651,1.75);
#4654=CIRCLE('',#12656,0.16);
#4655=CIRCLE('',#12657,0.2);
#4656=CIRCLE('',#12660,0.16);
#4657=CIRCLE('',#12661,0.2);
#4658=CIRCLE('',#12663,0.2);
#4659=CIRCLE('',#12668,0.16);
#4660=CIRCLE('',#12671,0.2);
#4661=CIRCLE('',#12672,0.16);
#4662=CIRCLE('',#12680,1.);
#4663=CIRCLE('',#12684,1.);
#4664=CIRCLE('',#12686,1.);
#4665=CIRCLE('',#12687,1.);
#4666=CIRCLE('',#12692,1.01);
#4667=CIRCLE('',#12693,1.01);
#4668=CIRCLE('',#12695,1.35);
#4669=CIRCLE('',#12696,1.35);
#4670=CIRCLE('',#12701,1.01);
#4671=CIRCLE('',#12702,1.01);
#4672=CIRCLE('',#12704,1.35);
#4673=CIRCLE('',#12705,1.35);
#4674=CIRCLE('',#12710,0.21);
#4675=CIRCLE('',#12712,0.21);
#4676=CIRCLE('',#12713,0.21);
#4677=CIRCLE('',#12716,1.005);
#4678=CIRCLE('',#12717,1.005);
#4679=CIRCLE('',#12719,1.6);
#4680=CIRCLE('',#12720,1.6);
#4681=CIRCLE('',#12725,1.01);
#4682=CIRCLE('',#12726,1.01);
#4683=CIRCLE('',#12728,1.35);
#4684=CIRCLE('',#12729,1.35);
#4685=CIRCLE('',#12734,0.21);
#4686=CIRCLE('',#12736,0.21);
#4687=CIRCLE('',#12737,0.21);
#4688=CIRCLE('',#12740,1.005);
#4689=CIRCLE('',#12741,1.005);
#4690=CIRCLE('',#12743,1.6);
#4691=CIRCLE('',#12744,1.6);
#4692=CIRCLE('',#12749,1.01);
#4693=CIRCLE('',#12750,1.01);
#4694=CIRCLE('',#12752,1.35);
#4695=CIRCLE('',#12753,1.35);
#4696=CIRCLE('',#12761,3.75);
#4697=CIRCLE('',#12762,3.75);
#4698=CIRCLE('',#12763,3.75);
#4699=CIRCLE('',#12764,3.75);
#4700=CIRCLE('',#12765,3.75);
#4701=CIRCLE('',#12766,3.75);
#4702=CIRCLE('',#12767,3.75);
#4703=CIRCLE('',#12768,3.75);
#4704=CIRCLE('',#12769,3.75);
#4705=CIRCLE('',#12770,3.75);
#4706=CIRCLE('',#12771,3.75);
#4707=CIRCLE('',#12772,3.75);
#4708=CIRCLE('',#12773,3.75);
#4709=CIRCLE('',#12774,3.75);
#4710=CIRCLE('',#12775,3.75);
#4711=CIRCLE('',#12776,3.75);
#4712=CIRCLE('',#12777,3.75);
#4713=CIRCLE('',#12778,3.75);
#4714=CIRCLE('',#12779,3.75);
#4715=CIRCLE('',#12780,3.75);
#4716=CIRCLE('',#12781,3.75);
#4717=CIRCLE('',#12782,3.75);
#4718=CIRCLE('',#12783,3.75);
#4719=CIRCLE('',#12784,3.75);
#4720=CIRCLE('',#12785,3.75);
#4721=CIRCLE('',#12786,3.75);
#4722=CIRCLE('',#12787,3.75);
#4723=CIRCLE('',#12788,3.75);
#4724=CIRCLE('',#12789,3.75);
#4725=CIRCLE('',#12790,3.75);
#4726=CIRCLE('',#12791,3.75);
#4727=CIRCLE('',#12792,3.75);
#4728=CIRCLE('',#12793,3.75);
#4729=CIRCLE('',#12794,3.75);
#4730=CIRCLE('',#12795,3.75);
#4731=CIRCLE('',#12796,3.75);
#4732=CIRCLE('',#12797,3.75);
#4733=CIRCLE('',#12798,3.75);
#4734=CIRCLE('',#12799,3.75);
#4735=CIRCLE('',#12800,3.75);
#4736=CIRCLE('',#12801,1.);
#4737=CIRCLE('',#12803,1.);
#4738=CIRCLE('',#12805,2.);
#4739=CIRCLE('',#12806,2.);
#4740=CIRCLE('',#12810,3.75);
#4741=CIRCLE('',#12813,3.75);
#4742=CIRCLE('',#12816,3.75);
#4743=CIRCLE('',#12819,3.75);
#4744=CIRCLE('',#12822,3.75);
#4745=CIRCLE('',#12825,3.75);
#4746=CIRCLE('',#12828,3.75);
#4747=CIRCLE('',#12831,3.75);
#4748=CIRCLE('',#12834,3.75);
#4749=CIRCLE('',#12837,3.75);
#4750=CIRCLE('',#12840,3.75);
#4751=CIRCLE('',#12843,3.75);
#4752=CIRCLE('',#12846,3.75);
#4753=CIRCLE('',#12849,3.75);
#4754=CIRCLE('',#12852,3.75);
#4755=CIRCLE('',#12855,3.75);
#4756=CIRCLE('',#12858,3.75);
#4757=CIRCLE('',#12861,3.75);
#4758=CIRCLE('',#12864,3.75);
#4759=CIRCLE('',#12867,3.75);
#4760=CIRCLE('',#12870,3.75);
#4761=CIRCLE('',#12873,3.75);
#4762=CIRCLE('',#12876,3.75);
#4763=CIRCLE('',#12879,3.75);
#4764=CIRCLE('',#12882,3.75);
#4765=CIRCLE('',#12885,3.75);
#4766=CIRCLE('',#12888,3.75);
#4767=CIRCLE('',#12891,3.75);
#4768=CIRCLE('',#12894,3.75);
#4769=CIRCLE('',#12897,3.75);
#4770=CIRCLE('',#12900,3.75);
#4771=CIRCLE('',#12903,3.75);
#4772=CIRCLE('',#12906,3.75);
#4773=CIRCLE('',#12909,3.75);
#4774=CIRCLE('',#12912,3.75);
#4775=CIRCLE('',#12915,3.75);
#4776=CIRCLE('',#12918,3.75);
#4777=CIRCLE('',#12921,3.75);
#4778=CIRCLE('',#12924,3.75);
#4779=CIRCLE('',#12927,3.75);
#4780=CIRCLE('',#12949,0.22);
#4781=CIRCLE('',#12951,0.24505);
#4782=CIRCLE('',#12953,0.24505);
#4783=CIRCLE('',#12955,0.175);
#4784=VERTEX_POINT('',#15979);
#4785=VERTEX_POINT('',#15981);
#4786=VERTEX_POINT('',#15985);
#4787=VERTEX_POINT('',#15987);
#4788=VERTEX_POINT('',#15991);
#4789=VERTEX_POINT('',#15993);
#4790=VERTEX_POINT('',#15997);
#4791=VERTEX_POINT('',#15999);
#4792=VERTEX_POINT('',#16003);
#4793=VERTEX_POINT('',#16004);
#4794=VERTEX_POINT('',#16006);
#4795=VERTEX_POINT('',#16008);
#4796=VERTEX_POINT('',#16012);
#4797=VERTEX_POINT('',#16014);
#4798=VERTEX_POINT('',#16018);
#4799=VERTEX_POINT('',#16020);
#4800=VERTEX_POINT('',#16030);
#4801=VERTEX_POINT('',#16032);
#4802=VERTEX_POINT('',#16036);
#4803=VERTEX_POINT('',#16038);
#4804=VERTEX_POINT('',#16042);
#4805=VERTEX_POINT('',#16044);
#4806=VERTEX_POINT('',#16048);
#4807=VERTEX_POINT('',#16050);
#4808=VERTEX_POINT('',#16054);
#4809=VERTEX_POINT('',#16056);
#4810=VERTEX_POINT('',#16060);
#4811=VERTEX_POINT('',#16062);
#4812=VERTEX_POINT('',#16066);
#4813=VERTEX_POINT('',#16068);
#4814=VERTEX_POINT('',#16072);
#4815=VERTEX_POINT('',#16075);
#4816=VERTEX_POINT('',#16077);
#4817=VERTEX_POINT('',#16081);
#4818=VERTEX_POINT('',#16084);
#4819=VERTEX_POINT('',#16086);
#4820=VERTEX_POINT('',#16090);
#4821=VERTEX_POINT('',#16093);
#4822=VERTEX_POINT('',#16095);
#4823=VERTEX_POINT('',#16099);
#4824=VERTEX_POINT('',#16102);
#4825=VERTEX_POINT('',#16106);
#4826=VERTEX_POINT('',#16110);
#4827=VERTEX_POINT('',#16114);
#4828=VERTEX_POINT('',#16118);
#4829=VERTEX_POINT('',#16120);
#4830=VERTEX_POINT('',#16125);
#4831=VERTEX_POINT('',#16127);
#4832=VERTEX_POINT('',#16132);
#4833=VERTEX_POINT('',#16134);
#4834=VERTEX_POINT('',#16138);
#4835=VERTEX_POINT('',#16141);
#4836=VERTEX_POINT('',#16145);
#4837=VERTEX_POINT('',#16147);
#4838=VERTEX_POINT('',#16151);
#4839=VERTEX_POINT('',#16154);
#4840=VERTEX_POINT('',#16158);
#4841=VERTEX_POINT('',#16159);
#4842=VERTEX_POINT('',#16161);
#4843=VERTEX_POINT('',#16163);
#4844=VERTEX_POINT('',#16167);
#4845=VERTEX_POINT('',#16169);
#4846=VERTEX_POINT('',#16173);
#4847=VERTEX_POINT('',#16175);
#4848=VERTEX_POINT('',#16185);
#4849=VERTEX_POINT('',#16187);
#4850=VERTEX_POINT('',#16191);
#4851=VERTEX_POINT('',#16193);
#4852=VERTEX_POINT('',#16197);
#4853=VERTEX_POINT('',#16199);
#4854=VERTEX_POINT('',#16203);
#4855=VERTEX_POINT('',#16205);
#4856=VERTEX_POINT('',#16209);
#4857=VERTEX_POINT('',#16211);
#4858=VERTEX_POINT('',#16215);
#4859=VERTEX_POINT('',#16217);
#4860=VERTEX_POINT('',#16221);
#4861=VERTEX_POINT('',#16223);
#4862=VERTEX_POINT('',#16227);
#4863=VERTEX_POINT('',#16230);
#4864=VERTEX_POINT('',#16232);
#4865=VERTEX_POINT('',#16236);
#4866=VERTEX_POINT('',#16239);
#4867=VERTEX_POINT('',#16241);
#4868=VERTEX_POINT('',#16245);
#4869=VERTEX_POINT('',#16248);
#4870=VERTEX_POINT('',#16250);
#4871=VERTEX_POINT('',#16254);
#4872=VERTEX_POINT('',#16257);
#4873=VERTEX_POINT('',#16261);
#4874=VERTEX_POINT('',#16265);
#4875=VERTEX_POINT('',#16269);
#4876=VERTEX_POINT('',#16273);
#4877=VERTEX_POINT('',#16275);
#4878=VERTEX_POINT('',#16280);
#4879=VERTEX_POINT('',#16282);
#4880=VERTEX_POINT('',#16287);
#4881=VERTEX_POINT('',#16289);
#4882=VERTEX_POINT('',#16293);
#4883=VERTEX_POINT('',#16296);
#4884=VERTEX_POINT('',#16300);
#4885=VERTEX_POINT('',#16302);
#4886=VERTEX_POINT('',#16306);
#4887=VERTEX_POINT('',#16309);
#4888=VERTEX_POINT('',#16313);
#4889=VERTEX_POINT('',#16314);
#4890=VERTEX_POINT('',#16316);
#4891=VERTEX_POINT('',#16318);
#4892=VERTEX_POINT('',#16322);
#4893=VERTEX_POINT('',#16324);
#4894=VERTEX_POINT('',#16328);
#4895=VERTEX_POINT('',#16330);
#4896=VERTEX_POINT('',#16340);
#4897=VERTEX_POINT('',#16342);
#4898=VERTEX_POINT('',#16346);
#4899=VERTEX_POINT('',#16348);
#4900=VERTEX_POINT('',#16355);
#4901=VERTEX_POINT('',#16357);
#4902=VERTEX_POINT('',#16361);
#4903=VERTEX_POINT('',#16363);
#4904=VERTEX_POINT('',#16370);
#4905=VERTEX_POINT('',#16372);
#4906=VERTEX_POINT('',#16376);
#4907=VERTEX_POINT('',#16378);
#4908=VERTEX_POINT('',#16385);
#4909=VERTEX_POINT('',#16387);
#4910=VERTEX_POINT('',#16391);
#4911=VERTEX_POINT('',#16393);
#4912=VERTEX_POINT('',#16400);
#4913=VERTEX_POINT('',#16402);
#4914=VERTEX_POINT('',#16406);
#4915=VERTEX_POINT('',#16408);
#4916=VERTEX_POINT('',#16412);
#4917=VERTEX_POINT('',#16414);
#4918=VERTEX_POINT('',#16418);
#4919=VERTEX_POINT('',#16420);
#4920=VERTEX_POINT('',#16424);
#4921=VERTEX_POINT('',#16427);
#4922=VERTEX_POINT('',#16431);
#4923=VERTEX_POINT('',#16433);
#4924=VERTEX_POINT('',#16440);
#4925=VERTEX_POINT('',#16442);
#4926=VERTEX_POINT('',#16446);
#4927=VERTEX_POINT('',#16448);
#4928=VERTEX_POINT('',#16452);
#4929=VERTEX_POINT('',#16454);
#4930=VERTEX_POINT('',#16458);
#4931=VERTEX_POINT('',#16460);
#4932=VERTEX_POINT('',#16464);
#4933=VERTEX_POINT('',#16467);
#4934=VERTEX_POINT('',#16471);
#4935=VERTEX_POINT('',#16473);
#4936=VERTEX_POINT('',#16480);
#4937=VERTEX_POINT('',#16482);
#4938=VERTEX_POINT('',#16486);
#4939=VERTEX_POINT('',#16488);
#4940=VERTEX_POINT('',#16492);
#4941=VERTEX_POINT('',#16494);
#4942=VERTEX_POINT('',#16498);
#4943=VERTEX_POINT('',#16500);
#4944=VERTEX_POINT('',#16504);
#4945=VERTEX_POINT('',#16507);
#4946=VERTEX_POINT('',#16511);
#4947=VERTEX_POINT('',#16513);
#4948=VERTEX_POINT('',#16520);
#4949=VERTEX_POINT('',#16522);
#4950=VERTEX_POINT('',#16526);
#4951=VERTEX_POINT('',#16528);
#4952=VERTEX_POINT('',#16532);
#4953=VERTEX_POINT('',#16534);
#4954=VERTEX_POINT('',#16538);
#4955=VERTEX_POINT('',#16540);
#4956=VERTEX_POINT('',#16544);
#4957=VERTEX_POINT('',#16547);
#4958=VERTEX_POINT('',#16551);
#4959=VERTEX_POINT('',#16553);
#4960=VERTEX_POINT('',#16560);
#4961=VERTEX_POINT('',#16563);
#4962=VERTEX_POINT('',#16567);
#4963=VERTEX_POINT('',#16571);
#4964=VERTEX_POINT('',#16575);
#4965=VERTEX_POINT('',#16578);
#4966=VERTEX_POINT('',#16582);
#4967=VERTEX_POINT('',#16586);
#4968=VERTEX_POINT('',#16591);
#4969=VERTEX_POINT('',#16592);
#4970=VERTEX_POINT('',#16594);
#4971=VERTEX_POINT('',#16596);
#4972=VERTEX_POINT('',#16600);
#4973=VERTEX_POINT('',#16602);
#4974=VERTEX_POINT('',#16606);
#4975=VERTEX_POINT('',#16608);
#4976=VERTEX_POINT('',#16612);
#4977=VERTEX_POINT('',#16614);
#4978=VERTEX_POINT('',#16618);
#4979=VERTEX_POINT('',#16620);
#4980=VERTEX_POINT('',#16630);
#4981=VERTEX_POINT('',#16633);
#4982=VERTEX_POINT('',#16637);
#4983=VERTEX_POINT('',#16641);
#4984=VERTEX_POINT('',#16645);
#4985=VERTEX_POINT('',#16648);
#4986=VERTEX_POINT('',#16652);
#4987=VERTEX_POINT('',#16656);
#4988=VERTEX_POINT('',#16661);
#4989=VERTEX_POINT('',#16662);
#4990=VERTEX_POINT('',#16664);
#4991=VERTEX_POINT('',#16666);
#4992=VERTEX_POINT('',#16670);
#4993=VERTEX_POINT('',#16672);
#4994=VERTEX_POINT('',#16676);
#4995=VERTEX_POINT('',#16678);
#4996=VERTEX_POINT('',#16682);
#4997=VERTEX_POINT('',#16684);
#4998=VERTEX_POINT('',#16688);
#4999=VERTEX_POINT('',#16690);
#5000=VERTEX_POINT('',#16701);
#5001=VERTEX_POINT('',#16702);
#5002=VERTEX_POINT('',#16705);
#5003=VERTEX_POINT('',#16707);
#5004=VERTEX_POINT('',#16711);
#5005=VERTEX_POINT('',#16715);
#5006=VERTEX_POINT('',#16717);
#5007=VERTEX_POINT('',#16721);
#5008=VERTEX_POINT('',#16726);
#5009=VERTEX_POINT('',#16730);
#5010=VERTEX_POINT('',#16736);
#5011=VERTEX_POINT('',#16737);
#5012=VERTEX_POINT('',#16740);
#5013=VERTEX_POINT('',#16742);
#5014=VERTEX_POINT('',#16746);
#5015=VERTEX_POINT('',#16750);
#5016=VERTEX_POINT('',#16752);
#5017=VERTEX_POINT('',#16755);
#5018=VERTEX_POINT('',#16759);
#5019=VERTEX_POINT('',#16763);
#5020=VERTEX_POINT('',#16771);
#5021=VERTEX_POINT('',#16772);
#5022=VERTEX_POINT('',#16775);
#5023=VERTEX_POINT('',#16776);
#5024=VERTEX_POINT('',#16779);
#5025=VERTEX_POINT('',#16780);
#5026=VERTEX_POINT('',#16783);
#5027=VERTEX_POINT('',#16784);
#5028=VERTEX_POINT('',#16787);
#5029=VERTEX_POINT('',#16788);
#5030=VERTEX_POINT('',#16791);
#5031=VERTEX_POINT('',#16792);
#5032=VERTEX_POINT('',#16795);
#5033=VERTEX_POINT('',#16796);
#5034=VERTEX_POINT('',#16800);
#5035=VERTEX_POINT('',#16801);
#5036=VERTEX_POINT('',#16824);
#5037=VERTEX_POINT('',#16826);
#5038=VERTEX_POINT('',#16851);
#5039=VERTEX_POINT('',#16853);
#5040=VERTEX_POINT('',#16876);
#5041=VERTEX_POINT('',#16878);
#5042=VERTEX_POINT('',#16901);
#5043=VERTEX_POINT('',#16903);
#5044=VERTEX_POINT('',#16906);
#5045=VERTEX_POINT('',#16908);
#5046=VERTEX_POINT('',#16931);
#5047=VERTEX_POINT('',#16933);
#5048=VERTEX_POINT('',#16956);
#5049=VERTEX_POINT('',#16958);
#5050=VERTEX_POINT('',#16981);
#5051=VERTEX_POINT('',#16983);
#5052=VERTEX_POINT('',#17008);
#5053=VERTEX_POINT('',#17012);
#5054=VERTEX_POINT('',#17037);
#5055=VERTEX_POINT('',#17041);
#5056=VERTEX_POINT('',#17066);
#5057=VERTEX_POINT('',#17068);
#5058=VERTEX_POINT('',#17072);
#5059=VERTEX_POINT('',#17097);
#5060=VERTEX_POINT('',#17101);
#5061=VERTEX_POINT('',#17126);
#5062=VERTEX_POINT('',#17130);
#5063=VERTEX_POINT('',#17155);
#5064=VERTEX_POINT('',#17158);
#5065=VERTEX_POINT('',#17160);
#5066=VERTEX_POINT('',#17192);
#5067=VERTEX_POINT('',#17194);
#5068=VERTEX_POINT('',#17197);
#5069=VERTEX_POINT('',#17201);
#5070=VERTEX_POINT('',#17206);
#5071=VERTEX_POINT('',#17208);
#5072=VERTEX_POINT('',#17211);
#5073=VERTEX_POINT('',#17215);
#5074=VERTEX_POINT('',#17227);
#5075=VERTEX_POINT('',#17228);
#5076=VERTEX_POINT('',#17231);
#5077=VERTEX_POINT('',#17233);
#5078=VERTEX_POINT('',#17237);
#5079=VERTEX_POINT('',#17241);
#5080=VERTEX_POINT('',#17243);
#5081=VERTEX_POINT('',#17247);
#5082=VERTEX_POINT('',#17252);
#5083=VERTEX_POINT('',#17256);
#5084=VERTEX_POINT('',#17262);
#5085=VERTEX_POINT('',#17263);
#5086=VERTEX_POINT('',#17266);
#5087=VERTEX_POINT('',#17268);
#5088=VERTEX_POINT('',#17272);
#5089=VERTEX_POINT('',#17276);
#5090=VERTEX_POINT('',#17278);
#5091=VERTEX_POINT('',#17281);
#5092=VERTEX_POINT('',#17285);
#5093=VERTEX_POINT('',#17289);
#5094=VERTEX_POINT('',#17297);
#5095=VERTEX_POINT('',#17298);
#5096=VERTEX_POINT('',#17301);
#5097=VERTEX_POINT('',#17302);
#5098=VERTEX_POINT('',#17305);
#5099=VERTEX_POINT('',#17306);
#5100=VERTEX_POINT('',#17309);
#5101=VERTEX_POINT('',#17310);
#5102=VERTEX_POINT('',#17313);
#5103=VERTEX_POINT('',#17314);
#5104=VERTEX_POINT('',#17317);
#5105=VERTEX_POINT('',#17318);
#5106=VERTEX_POINT('',#17321);
#5107=VERTEX_POINT('',#17322);
#5108=VERTEX_POINT('',#17325);
#5109=VERTEX_POINT('',#17326);
#5110=VERTEX_POINT('',#17330);
#5111=VERTEX_POINT('',#17331);
#5112=VERTEX_POINT('',#17354);
#5113=VERTEX_POINT('',#17356);
#5114=VERTEX_POINT('',#17381);
#5115=VERTEX_POINT('',#17383);
#5116=VERTEX_POINT('',#17406);
#5117=VERTEX_POINT('',#17408);
#5118=VERTEX_POINT('',#17431);
#5119=VERTEX_POINT('',#17433);
#5120=VERTEX_POINT('',#17446);
#5121=VERTEX_POINT('',#17449);
#5122=VERTEX_POINT('',#17462);
#5123=VERTEX_POINT('',#17464);
#5124=VERTEX_POINT('',#17487);
#5125=VERTEX_POINT('',#17489);
#5126=VERTEX_POINT('',#17512);
#5127=VERTEX_POINT('',#17514);
#5128=VERTEX_POINT('',#17537);
#5129=VERTEX_POINT('',#17539);
#5130=VERTEX_POINT('',#17564);
#5131=VERTEX_POINT('',#17568);
#5132=VERTEX_POINT('',#17593);
#5133=VERTEX_POINT('',#17597);
#5134=VERTEX_POINT('',#17622);
#5135=VERTEX_POINT('',#17626);
#5136=VERTEX_POINT('',#17627);
#5137=VERTEX_POINT('',#17654);
#5138=VERTEX_POINT('',#17658);
#5139=VERTEX_POINT('',#17683);
#5140=VERTEX_POINT('',#17687);
#5141=VERTEX_POINT('',#17712);
#5142=VERTEX_POINT('',#17716);
#5143=VERTEX_POINT('',#17741);
#5144=VERTEX_POINT('',#17744);
#5145=VERTEX_POINT('',#17746);
#5146=VERTEX_POINT('',#17778);
#5147=VERTEX_POINT('',#17780);
#5148=VERTEX_POINT('',#17783);
#5149=VERTEX_POINT('',#17787);
#5150=VERTEX_POINT('',#17792);
#5151=VERTEX_POINT('',#17794);
#5152=VERTEX_POINT('',#17797);
#5153=VERTEX_POINT('',#17801);
#5154=VERTEX_POINT('',#17812);
#5155=VERTEX_POINT('',#17815);
#5156=VERTEX_POINT('',#17819);
#5157=VERTEX_POINT('',#17823);
#5158=VERTEX_POINT('',#17827);
#5159=VERTEX_POINT('',#17830);
#5160=VERTEX_POINT('',#17834);
#5161=VERTEX_POINT('',#17838);
#5162=VERTEX_POINT('',#17843);
#5163=VERTEX_POINT('',#17844);
#5164=VERTEX_POINT('',#17846);
#5165=VERTEX_POINT('',#17848);
#5166=VERTEX_POINT('',#17852);
#5167=VERTEX_POINT('',#17854);
#5168=VERTEX_POINT('',#17858);
#5169=VERTEX_POINT('',#17860);
#5170=VERTEX_POINT('',#17864);
#5171=VERTEX_POINT('',#17866);
#5172=VERTEX_POINT('',#17870);
#5173=VERTEX_POINT('',#17872);
#5174=VERTEX_POINT('',#17922);
#5175=VERTEX_POINT('',#17923);
#5176=VERTEX_POINT('',#17925);
#5177=VERTEX_POINT('',#17927);
#5178=VERTEX_POINT('',#17931);
#5179=VERTEX_POINT('',#17933);
#5180=VERTEX_POINT('',#17937);
#5181=VERTEX_POINT('',#17939);
#5182=VERTEX_POINT('',#17947);
#5183=VERTEX_POINT('',#17949);
#5184=VERTEX_POINT('',#17956);
#5185=VERTEX_POINT('',#17958);
#5186=VERTEX_POINT('',#17962);
#5187=VERTEX_POINT('',#17964);
#5188=VERTEX_POINT('',#17971);
#5189=VERTEX_POINT('',#17973);
#5190=VERTEX_POINT('',#17977);
#5191=VERTEX_POINT('',#17979);
#5192=VERTEX_POINT('',#17986);
#5193=VERTEX_POINT('',#17987);
#5194=VERTEX_POINT('',#17991);
#5195=VERTEX_POINT('',#18002);
#5196=VERTEX_POINT('',#18004);
#5197=VERTEX_POINT('',#18006);
#5198=VERTEX_POINT('',#18043);
#5199=VERTEX_POINT('',#18058);
#5200=VERTEX_POINT('',#18060);
#5201=VERTEX_POINT('',#18064);
#5202=VERTEX_POINT('',#18066);
#5203=VERTEX_POINT('',#18073);
#5204=VERTEX_POINT('',#18075);
#5205=VERTEX_POINT('',#18079);
#5206=VERTEX_POINT('',#18081);
#5207=VERTEX_POINT('',#18088);
#5208=VERTEX_POINT('',#18089);
#5209=VERTEX_POINT('',#18093);
#5210=VERTEX_POINT('',#18104);
#5211=VERTEX_POINT('',#18106);
#5212=VERTEX_POINT('',#18108);
#5213=VERTEX_POINT('',#18145);
#5214=VERTEX_POINT('',#18160);
#5215=VERTEX_POINT('',#18162);
#5216=VERTEX_POINT('',#18166);
#5217=VERTEX_POINT('',#18168);
#5218=VERTEX_POINT('',#18175);
#5219=VERTEX_POINT('',#18177);
#5220=VERTEX_POINT('',#18181);
#5221=VERTEX_POINT('',#18183);
#5222=VERTEX_POINT('',#18190);
#5223=VERTEX_POINT('',#18191);
#5224=VERTEX_POINT('',#18193);
#5225=VERTEX_POINT('',#18195);
#5226=VERTEX_POINT('',#18199);
#5227=VERTEX_POINT('',#18201);
#5228=VERTEX_POINT('',#18205);
#5229=VERTEX_POINT('',#18207);
#5230=VERTEX_POINT('',#18211);
#5231=VERTEX_POINT('',#18212);
#5232=VERTEX_POINT('',#18214);
#5233=VERTEX_POINT('',#18285);
#5234=VERTEX_POINT('',#18287);
#5235=VERTEX_POINT('',#18358);
#5236=VERTEX_POINT('',#18360);
#5237=VERTEX_POINT('',#18431);
#5238=VERTEX_POINT('',#18433);
#5239=VERTEX_POINT('',#18504);
#5240=VERTEX_POINT('',#18506);
#5241=VERTEX_POINT('',#18577);
#5242=VERTEX_POINT('',#18579);
#5243=VERTEX_POINT('',#18650);
#5244=VERTEX_POINT('',#18652);
#5245=VERTEX_POINT('',#18723);
#5246=VERTEX_POINT('',#18725);
#5247=VERTEX_POINT('',#18796);
#5248=VERTEX_POINT('',#18798);
#5249=VERTEX_POINT('',#18869);
#5250=VERTEX_POINT('',#18871);
#5251=VERTEX_POINT('',#18942);
#5252=VERTEX_POINT('',#18944);
#5253=VERTEX_POINT('',#19015);
#5254=VERTEX_POINT('',#19017);
#5255=VERTEX_POINT('',#19088);
#5256=VERTEX_POINT('',#19090);
#5257=VERTEX_POINT('',#19161);
#5258=VERTEX_POINT('',#19163);
#5259=VERTEX_POINT('',#19234);
#5260=VERTEX_POINT('',#19236);
#5261=VERTEX_POINT('',#19307);
#5262=VERTEX_POINT('',#19309);
#5263=VERTEX_POINT('',#19380);
#5264=VERTEX_POINT('',#19382);
#5265=VERTEX_POINT('',#19453);
#5266=VERTEX_POINT('',#19455);
#5267=VERTEX_POINT('',#19526);
#5268=VERTEX_POINT('',#19528);
#5269=VERTEX_POINT('',#19599);
#5270=VERTEX_POINT('',#19601);
#5271=VERTEX_POINT('',#19672);
#5272=VERTEX_POINT('',#19674);
#5273=VERTEX_POINT('',#19745);
#5274=VERTEX_POINT('',#19747);
#5275=VERTEX_POINT('',#19818);
#5276=VERTEX_POINT('',#19820);
#5277=VERTEX_POINT('',#19891);
#5278=VERTEX_POINT('',#19893);
#5279=VERTEX_POINT('',#19964);
#5280=VERTEX_POINT('',#19966);
#5281=VERTEX_POINT('',#20037);
#5282=VERTEX_POINT('',#20039);
#5283=VERTEX_POINT('',#20110);
#5284=VERTEX_POINT('',#20112);
#5285=VERTEX_POINT('',#20183);
#5286=VERTEX_POINT('',#20185);
#5287=VERTEX_POINT('',#20256);
#5288=VERTEX_POINT('',#20258);
#5289=VERTEX_POINT('',#20329);
#5290=VERTEX_POINT('',#20331);
#5291=VERTEX_POINT('',#20402);
#5292=VERTEX_POINT('',#20404);
#5293=VERTEX_POINT('',#20475);
#5294=VERTEX_POINT('',#20477);
#5295=VERTEX_POINT('',#20548);
#5296=VERTEX_POINT('',#20550);
#5297=VERTEX_POINT('',#20621);
#5298=VERTEX_POINT('',#20623);
#5299=VERTEX_POINT('',#20694);
#5300=VERTEX_POINT('',#20696);
#5301=VERTEX_POINT('',#20767);
#5302=VERTEX_POINT('',#20769);
#5303=VERTEX_POINT('',#20840);
#5304=VERTEX_POINT('',#20842);
#5305=VERTEX_POINT('',#20913);
#5306=VERTEX_POINT('',#20915);
#5307=VERTEX_POINT('',#20986);
#5308=VERTEX_POINT('',#20988);
#5309=VERTEX_POINT('',#21059);
#5310=VERTEX_POINT('',#21135);
#5311=VERTEX_POINT('',#21137);
#5312=VERTEX_POINT('',#21281);
#5313=VERTEX_POINT('',#21283);
#5314=VERTEX_POINT('',#21356);
#5315=VERTEX_POINT('',#21499);
#5316=VERTEX_POINT('',#21572);
#5317=VERTEX_POINT('',#21715);
#5318=VERTEX_POINT('',#21788);
#5319=VERTEX_POINT('',#21931);
#5320=VERTEX_POINT('',#22004);
#5321=VERTEX_POINT('',#22147);
#5322=VERTEX_POINT('',#22220);
#5323=VERTEX_POINT('',#22363);
#5324=VERTEX_POINT('',#22436);
#5325=VERTEX_POINT('',#22579);
#5326=VERTEX_POINT('',#22652);
#5327=VERTEX_POINT('',#22795);
#5328=VERTEX_POINT('',#22868);
#5329=VERTEX_POINT('',#23011);
#5330=VERTEX_POINT('',#23084);
#5331=VERTEX_POINT('',#23227);
#5332=VERTEX_POINT('',#23300);
#5333=VERTEX_POINT('',#23443);
#5334=VERTEX_POINT('',#23516);
#5335=VERTEX_POINT('',#23659);
#5336=VERTEX_POINT('',#23732);
#5337=VERTEX_POINT('',#23875);
#5338=VERTEX_POINT('',#23948);
#5339=VERTEX_POINT('',#24091);
#5340=VERTEX_POINT('',#24164);
#5341=VERTEX_POINT('',#24307);
#5342=VERTEX_POINT('',#24380);
#5343=VERTEX_POINT('',#24523);
#5344=VERTEX_POINT('',#24596);
#5345=VERTEX_POINT('',#24739);
#5346=VERTEX_POINT('',#24812);
#5347=VERTEX_POINT('',#24955);
#5348=VERTEX_POINT('',#25028);
#5349=VERTEX_POINT('',#25171);
#5350=VERTEX_POINT('',#25244);
#5351=VERTEX_POINT('',#25387);
#5352=VERTEX_POINT('',#25460);
#5353=VERTEX_POINT('',#25603);
#5354=VERTEX_POINT('',#25676);
#5355=VERTEX_POINT('',#25819);
#5356=VERTEX_POINT('',#25892);
#5357=VERTEX_POINT('',#26035);
#5358=VERTEX_POINT('',#26108);
#5359=VERTEX_POINT('',#26251);
#5360=VERTEX_POINT('',#26324);
#5361=VERTEX_POINT('',#26467);
#5362=VERTEX_POINT('',#26540);
#5363=VERTEX_POINT('',#26683);
#5364=VERTEX_POINT('',#26756);
#5365=VERTEX_POINT('',#26899);
#5366=VERTEX_POINT('',#26972);
#5367=VERTEX_POINT('',#27115);
#5368=VERTEX_POINT('',#27188);
#5369=VERTEX_POINT('',#27331);
#5370=VERTEX_POINT('',#27404);
#5371=VERTEX_POINT('',#27547);
#5372=VERTEX_POINT('',#27620);
#5373=VERTEX_POINT('',#27763);
#5374=VERTEX_POINT('',#27836);
#5375=VERTEX_POINT('',#27979);
#5376=VERTEX_POINT('',#28052);
#5377=VERTEX_POINT('',#28195);
#5378=VERTEX_POINT('',#28268);
#5379=VERTEX_POINT('',#28411);
#5380=VERTEX_POINT('',#28484);
#5381=VERTEX_POINT('',#28627);
#5382=VERTEX_POINT('',#28700);
#5383=VERTEX_POINT('',#28843);
#5384=VERTEX_POINT('',#28916);
#5385=VERTEX_POINT('',#29059);
#5386=VERTEX_POINT('',#29132);
#5387=VERTEX_POINT('',#29275);
#5388=VERTEX_POINT('',#29348);
#5389=VERTEX_POINT('',#29491);
#5390=VERTEX_POINT('',#29564);
#5391=VERTEX_POINT('',#29707);
#5392=VERTEX_POINT('',#29784);
#5393=VERTEX_POINT('',#29785);
#5394=VERTEX_POINT('',#29787);
#5395=VERTEX_POINT('',#29789);
#5396=VERTEX_POINT('',#29793);
#5397=VERTEX_POINT('',#29794);
#5398=VERTEX_POINT('',#29799);
#5399=VERTEX_POINT('',#29800);
#5400=VERTEX_POINT('',#29808);
#5401=VERTEX_POINT('',#29810);
#5402=VERTEX_POINT('',#29814);
#5403=VERTEX_POINT('',#29819);
#5404=VERTEX_POINT('',#29821);
#5405=VERTEX_POINT('',#29825);
#5406=VERTEX_POINT('',#29829);
#5407=VERTEX_POINT('',#29830);
#5408=VERTEX_POINT('',#29844);
#5409=VERTEX_POINT('',#29845);
#5410=VERTEX_POINT('',#29847);
#5411=VERTEX_POINT('',#29849);
#5412=VERTEX_POINT('',#29853);
#5413=VERTEX_POINT('',#29855);
#5414=VERTEX_POINT('',#29859);
#5415=VERTEX_POINT('',#29861);
#5416=VERTEX_POINT('',#29869);
#5417=VERTEX_POINT('',#29871);
#5418=VERTEX_POINT('',#29878);
#5419=VERTEX_POINT('',#29880);
#5420=VERTEX_POINT('',#29884);
#5421=VERTEX_POINT('',#29886);
#5422=VERTEX_POINT('',#29893);
#5423=VERTEX_POINT('',#29895);
#5424=VERTEX_POINT('',#29899);
#5425=VERTEX_POINT('',#29901);
#5426=VERTEX_POINT('',#29908);
#5427=VERTEX_POINT('',#29909);
#5428=VERTEX_POINT('',#29913);
#5429=VERTEX_POINT('',#29928);
#5430=VERTEX_POINT('',#29930);
#5431=VERTEX_POINT('',#29932);
#5432=VERTEX_POINT('',#29969);
#5433=VERTEX_POINT('',#29988);
#5434=VERTEX_POINT('',#29990);
#5435=VERTEX_POINT('',#29994);
#5436=VERTEX_POINT('',#29996);
#5437=VERTEX_POINT('',#30003);
#5438=VERTEX_POINT('',#30005);
#5439=VERTEX_POINT('',#30009);
#5440=VERTEX_POINT('',#30011);
#5441=VERTEX_POINT('',#30018);
#5442=VERTEX_POINT('',#30019);
#5443=VERTEX_POINT('',#30023);
#5444=VERTEX_POINT('',#30038);
#5445=VERTEX_POINT('',#30040);
#5446=VERTEX_POINT('',#30042);
#5447=VERTEX_POINT('',#30079);
#5448=VERTEX_POINT('',#30098);
#5449=VERTEX_POINT('',#30100);
#5450=VERTEX_POINT('',#30104);
#5451=VERTEX_POINT('',#30106);
#5452=VERTEX_POINT('',#30113);
#5453=VERTEX_POINT('',#30115);
#5454=VERTEX_POINT('',#30119);
#5455=VERTEX_POINT('',#30121);
#5456=VERTEX_POINT('',#30128);
#5457=VERTEX_POINT('',#30129);
#5458=VERTEX_POINT('',#30131);
#5459=VERTEX_POINT('',#30133);
#5460=VERTEX_POINT('',#30137);
#5461=VERTEX_POINT('',#30139);
#5462=VERTEX_POINT('',#30143);
#5463=VERTEX_POINT('',#30145);
#5464=VERTEX_POINT('',#30149);
#5465=VERTEX_POINT('',#30150);
#5466=VERTEX_POINT('',#30152);
#5467=VERTEX_POINT('',#30223);
#5468=VERTEX_POINT('',#30225);
#5469=VERTEX_POINT('',#30296);
#5470=VERTEX_POINT('',#30298);
#5471=VERTEX_POINT('',#30369);
#5472=VERTEX_POINT('',#30371);
#5473=VERTEX_POINT('',#30442);
#5474=VERTEX_POINT('',#30444);
#5475=VERTEX_POINT('',#30515);
#5476=VERTEX_POINT('',#30517);
#5477=VERTEX_POINT('',#30588);
#5478=VERTEX_POINT('',#30590);
#5479=VERTEX_POINT('',#30661);
#5480=VERTEX_POINT('',#30663);
#5481=VERTEX_POINT('',#30734);
#5482=VERTEX_POINT('',#30736);
#5483=VERTEX_POINT('',#30807);
#5484=VERTEX_POINT('',#30809);
#5485=VERTEX_POINT('',#30880);
#5486=VERTEX_POINT('',#30882);
#5487=VERTEX_POINT('',#30953);
#5488=VERTEX_POINT('',#30955);
#5489=VERTEX_POINT('',#31026);
#5490=VERTEX_POINT('',#31028);
#5491=VERTEX_POINT('',#31099);
#5492=VERTEX_POINT('',#31101);
#5493=VERTEX_POINT('',#31172);
#5494=VERTEX_POINT('',#31174);
#5495=VERTEX_POINT('',#31245);
#5496=VERTEX_POINT('',#31247);
#5497=VERTEX_POINT('',#31318);
#5498=VERTEX_POINT('',#31320);
#5499=VERTEX_POINT('',#31391);
#5500=VERTEX_POINT('',#31393);
#5501=VERTEX_POINT('',#31464);
#5502=VERTEX_POINT('',#31466);
#5503=VERTEX_POINT('',#31537);
#5504=VERTEX_POINT('',#31539);
#5505=VERTEX_POINT('',#31610);
#5506=VERTEX_POINT('',#31612);
#5507=VERTEX_POINT('',#31683);
#5508=VERTEX_POINT('',#31685);
#5509=VERTEX_POINT('',#31756);
#5510=VERTEX_POINT('',#31758);
#5511=VERTEX_POINT('',#31829);
#5512=VERTEX_POINT('',#31831);
#5513=VERTEX_POINT('',#31902);
#5514=VERTEX_POINT('',#31904);
#5515=VERTEX_POINT('',#31975);
#5516=VERTEX_POINT('',#31977);
#5517=VERTEX_POINT('',#32048);
#5518=VERTEX_POINT('',#32050);
#5519=VERTEX_POINT('',#32121);
#5520=VERTEX_POINT('',#32123);
#5521=VERTEX_POINT('',#32194);
#5522=VERTEX_POINT('',#32196);
#5523=VERTEX_POINT('',#32267);
#5524=VERTEX_POINT('',#32269);
#5525=VERTEX_POINT('',#32340);
#5526=VERTEX_POINT('',#32342);
#5527=VERTEX_POINT('',#32413);
#5528=VERTEX_POINT('',#32415);
#5529=VERTEX_POINT('',#32486);
#5530=VERTEX_POINT('',#32488);
#5531=VERTEX_POINT('',#32559);
#5532=VERTEX_POINT('',#32561);
#5533=VERTEX_POINT('',#32632);
#5534=VERTEX_POINT('',#32634);
#5535=VERTEX_POINT('',#32705);
#5536=VERTEX_POINT('',#32707);
#5537=VERTEX_POINT('',#32778);
#5538=VERTEX_POINT('',#32780);
#5539=VERTEX_POINT('',#32851);
#5540=VERTEX_POINT('',#32853);
#5541=VERTEX_POINT('',#32924);
#5542=VERTEX_POINT('',#32926);
#5543=VERTEX_POINT('',#32997);
#5544=VERTEX_POINT('',#32999);
#5545=VERTEX_POINT('',#33070);
#5546=VERTEX_POINT('',#33072);
#5547=VERTEX_POINT('',#33143);
#5548=VERTEX_POINT('',#33145);
#5549=VERTEX_POINT('',#33216);
#5550=VERTEX_POINT('',#33218);
#5551=VERTEX_POINT('',#33289);
#5552=VERTEX_POINT('',#33291);
#5553=VERTEX_POINT('',#33362);
#5554=VERTEX_POINT('',#33364);
#5555=VERTEX_POINT('',#33435);
#5556=VERTEX_POINT('',#33437);
#5557=VERTEX_POINT('',#33508);
#5558=VERTEX_POINT('',#33510);
#5559=VERTEX_POINT('',#33581);
#5560=VERTEX_POINT('',#33583);
#5561=VERTEX_POINT('',#33654);
#5562=VERTEX_POINT('',#33656);
#5563=VERTEX_POINT('',#33727);
#5564=VERTEX_POINT('',#33729);
#5565=VERTEX_POINT('',#33800);
#5566=VERTEX_POINT('',#33802);
#5567=VERTEX_POINT('',#33873);
#5568=VERTEX_POINT('',#33875);
#5569=VERTEX_POINT('',#33946);
#5570=VERTEX_POINT('',#33948);
#5571=VERTEX_POINT('',#34019);
#5572=VERTEX_POINT('',#34021);
#5573=VERTEX_POINT('',#34092);
#5574=VERTEX_POINT('',#34094);
#5575=VERTEX_POINT('',#34165);
#5576=VERTEX_POINT('',#34167);
#5577=VERTEX_POINT('',#34238);
#5578=VERTEX_POINT('',#34240);
#5579=VERTEX_POINT('',#34311);
#5580=VERTEX_POINT('',#34313);
#5581=VERTEX_POINT('',#34384);
#5582=VERTEX_POINT('',#34386);
#5583=VERTEX_POINT('',#34457);
#5584=VERTEX_POINT('',#34459);
#5585=VERTEX_POINT('',#34530);
#5586=VERTEX_POINT('',#34532);
#5587=VERTEX_POINT('',#34603);
#5588=VERTEX_POINT('',#34605);
#5589=VERTEX_POINT('',#34676);
#5590=VERTEX_POINT('',#34678);
#5591=VERTEX_POINT('',#34749);
#5592=VERTEX_POINT('',#34751);
#5593=VERTEX_POINT('',#34822);
#5594=VERTEX_POINT('',#34824);
#5595=VERTEX_POINT('',#34895);
#5596=VERTEX_POINT('',#34897);
#5597=VERTEX_POINT('',#34968);
#5598=VERTEX_POINT('',#34970);
#5599=VERTEX_POINT('',#35041);
#5600=VERTEX_POINT('',#35043);
#5601=VERTEX_POINT('',#35114);
#5602=VERTEX_POINT('',#35116);
#5603=VERTEX_POINT('',#35187);
#5604=VERTEX_POINT('',#35189);
#5605=VERTEX_POINT('',#35260);
#5606=VERTEX_POINT('',#35262);
#5607=VERTEX_POINT('',#35333);
#5608=VERTEX_POINT('',#35335);
#5609=VERTEX_POINT('',#35406);
#5610=VERTEX_POINT('',#35408);
#5611=VERTEX_POINT('',#35479);
#5612=VERTEX_POINT('',#35481);
#5613=VERTEX_POINT('',#35552);
#5614=VERTEX_POINT('',#35554);
#5615=VERTEX_POINT('',#35625);
#5616=VERTEX_POINT('',#35627);
#5617=VERTEX_POINT('',#35698);
#5618=VERTEX_POINT('',#35700);
#5619=VERTEX_POINT('',#35771);
#5620=VERTEX_POINT('',#35773);
#5621=VERTEX_POINT('',#35844);
#5622=VERTEX_POINT('',#35846);
#5623=VERTEX_POINT('',#35917);
#5624=VERTEX_POINT('',#35993);
#5625=VERTEX_POINT('',#35995);
#5626=VERTEX_POINT('',#36139);
#5627=VERTEX_POINT('',#36146);
#5628=VERTEX_POINT('',#36358);
#5629=VERTEX_POINT('',#36365);
#5630=VERTEX_POINT('',#36440);
#5631=VERTEX_POINT('',#36588);
#5632=VERTEX_POINT('',#36800);
#5633=VERTEX_POINT('',#36807);
#5634=VERTEX_POINT('',#36882);
#5635=VERTEX_POINT('',#37030);
#5636=VERTEX_POINT('',#37242);
#5637=VERTEX_POINT('',#37249);
#5638=VERTEX_POINT('',#37324);
#5639=VERTEX_POINT('',#37472);
#5640=VERTEX_POINT('',#37684);
#5641=VERTEX_POINT('',#37691);
#5642=VERTEX_POINT('',#37766);
#5643=VERTEX_POINT('',#37914);
#5644=VERTEX_POINT('',#38126);
#5645=VERTEX_POINT('',#38133);
#5646=VERTEX_POINT('',#38208);
#5647=VERTEX_POINT('',#38356);
#5648=VERTEX_POINT('',#38568);
#5649=VERTEX_POINT('',#38575);
#5650=VERTEX_POINT('',#38650);
#5651=VERTEX_POINT('',#38798);
#5652=VERTEX_POINT('',#39010);
#5653=VERTEX_POINT('',#39017);
#5654=VERTEX_POINT('',#39092);
#5655=VERTEX_POINT('',#39240);
#5656=VERTEX_POINT('',#39452);
#5657=VERTEX_POINT('',#39459);
#5658=VERTEX_POINT('',#39534);
#5659=VERTEX_POINT('',#39682);
#5660=VERTEX_POINT('',#39894);
#5661=VERTEX_POINT('',#39901);
#5662=VERTEX_POINT('',#39976);
#5663=VERTEX_POINT('',#40124);
#5664=VERTEX_POINT('',#40336);
#5665=VERTEX_POINT('',#40343);
#5666=VERTEX_POINT('',#40418);
#5667=VERTEX_POINT('',#40566);
#5668=VERTEX_POINT('',#40778);
#5669=VERTEX_POINT('',#40785);
#5670=VERTEX_POINT('',#40860);
#5671=VERTEX_POINT('',#41008);
#5672=VERTEX_POINT('',#41220);
#5673=VERTEX_POINT('',#41227);
#5674=VERTEX_POINT('',#41302);
#5675=VERTEX_POINT('',#41450);
#5676=VERTEX_POINT('',#41662);
#5677=VERTEX_POINT('',#41669);
#5678=VERTEX_POINT('',#41744);
#5679=VERTEX_POINT('',#41892);
#5680=VERTEX_POINT('',#42104);
#5681=VERTEX_POINT('',#42111);
#5682=VERTEX_POINT('',#42186);
#5683=VERTEX_POINT('',#42334);
#5684=VERTEX_POINT('',#42546);
#5685=VERTEX_POINT('',#42553);
#5686=VERTEX_POINT('',#42628);
#5687=VERTEX_POINT('',#42776);
#5688=VERTEX_POINT('',#42988);
#5689=VERTEX_POINT('',#42995);
#5690=VERTEX_POINT('',#43070);
#5691=VERTEX_POINT('',#43218);
#5692=VERTEX_POINT('',#43430);
#5693=VERTEX_POINT('',#43437);
#5694=VERTEX_POINT('',#43512);
#5695=VERTEX_POINT('',#43660);
#5696=VERTEX_POINT('',#43872);
#5697=VERTEX_POINT('',#43879);
#5698=VERTEX_POINT('',#43954);
#5699=VERTEX_POINT('',#44102);
#5700=VERTEX_POINT('',#44314);
#5701=VERTEX_POINT('',#44321);
#5702=VERTEX_POINT('',#44396);
#5703=VERTEX_POINT('',#44544);
#5704=VERTEX_POINT('',#44756);
#5705=VERTEX_POINT('',#44763);
#5706=VERTEX_POINT('',#44838);
#5707=VERTEX_POINT('',#44986);
#5708=VERTEX_POINT('',#45198);
#5709=VERTEX_POINT('',#45205);
#5710=VERTEX_POINT('',#45280);
#5711=VERTEX_POINT('',#45428);
#5712=VERTEX_POINT('',#45640);
#5713=VERTEX_POINT('',#45647);
#5714=VERTEX_POINT('',#45722);
#5715=VERTEX_POINT('',#45870);
#5716=VERTEX_POINT('',#46082);
#5717=VERTEX_POINT('',#46089);
#5718=VERTEX_POINT('',#46164);
#5719=VERTEX_POINT('',#46312);
#5720=VERTEX_POINT('',#46524);
#5721=VERTEX_POINT('',#46531);
#5722=VERTEX_POINT('',#46606);
#5723=VERTEX_POINT('',#46754);
#5724=VERTEX_POINT('',#46966);
#5725=VERTEX_POINT('',#46973);
#5726=VERTEX_POINT('',#47048);
#5727=VERTEX_POINT('',#47196);
#5728=VERTEX_POINT('',#47408);
#5729=VERTEX_POINT('',#47415);
#5730=VERTEX_POINT('',#47490);
#5731=VERTEX_POINT('',#47638);
#5732=VERTEX_POINT('',#47850);
#5733=VERTEX_POINT('',#47857);
#5734=VERTEX_POINT('',#47932);
#5735=VERTEX_POINT('',#48080);
#5736=VERTEX_POINT('',#48292);
#5737=VERTEX_POINT('',#48299);
#5738=VERTEX_POINT('',#48374);
#5739=VERTEX_POINT('',#48522);
#5740=VERTEX_POINT('',#48734);
#5741=VERTEX_POINT('',#48741);
#5742=VERTEX_POINT('',#48816);
#5743=VERTEX_POINT('',#48964);
#5744=VERTEX_POINT('',#49176);
#5745=VERTEX_POINT('',#49183);
#5746=VERTEX_POINT('',#49258);
#5747=VERTEX_POINT('',#49406);
#5748=VERTEX_POINT('',#49618);
#5749=VERTEX_POINT('',#49625);
#5750=VERTEX_POINT('',#49700);
#5751=VERTEX_POINT('',#49848);
#5752=VERTEX_POINT('',#50060);
#5753=VERTEX_POINT('',#50067);
#5754=VERTEX_POINT('',#50142);
#5755=VERTEX_POINT('',#50290);
#5756=VERTEX_POINT('',#50502);
#5757=VERTEX_POINT('',#50509);
#5758=VERTEX_POINT('',#50584);
#5759=VERTEX_POINT('',#50732);
#5760=VERTEX_POINT('',#50944);
#5761=VERTEX_POINT('',#50951);
#5762=VERTEX_POINT('',#51026);
#5763=VERTEX_POINT('',#51174);
#5764=VERTEX_POINT('',#51386);
#5765=VERTEX_POINT('',#51393);
#5766=VERTEX_POINT('',#51468);
#5767=VERTEX_POINT('',#51616);
#5768=VERTEX_POINT('',#51828);
#5769=VERTEX_POINT('',#51835);
#5770=VERTEX_POINT('',#51910);
#5771=VERTEX_POINT('',#52058);
#5772=VERTEX_POINT('',#52270);
#5773=VERTEX_POINT('',#52277);
#5774=VERTEX_POINT('',#52352);
#5775=VERTEX_POINT('',#52500);
#5776=VERTEX_POINT('',#52712);
#5777=VERTEX_POINT('',#52719);
#5778=VERTEX_POINT('',#52794);
#5779=VERTEX_POINT('',#52942);
#5780=VERTEX_POINT('',#53015);
#5781=VERTEX_POINT('',#53158);
#5782=VERTEX_POINT('',#53236);
#5783=VERTEX_POINT('',#53384);
#5784=VERTEX_POINT('',#53391);
#5785=VERTEX_POINT('',#53603);
#5786=VERTEX_POINT('',#53682);
#5787=VERTEX_POINT('',#53683);
#5788=VERTEX_POINT('',#53685);
#5789=VERTEX_POINT('',#53687);
#5790=VERTEX_POINT('',#53689);
#5791=VERTEX_POINT('',#53691);
#5792=VERTEX_POINT('',#53693);
#5793=VERTEX_POINT('',#53695);
#5794=VERTEX_POINT('',#53699);
#5795=VERTEX_POINT('',#53701);
#5796=VERTEX_POINT('',#53705);
#5797=VERTEX_POINT('',#53709);
#5798=VERTEX_POINT('',#53713);
#5799=VERTEX_POINT('',#53717);
#5800=VERTEX_POINT('',#53718);
#5801=VERTEX_POINT('',#53721);
#5802=VERTEX_POINT('',#53733);
#5803=VERTEX_POINT('',#53734);
#5804=VERTEX_POINT('',#53736);
#5805=VERTEX_POINT('',#53738);
#5806=VERTEX_POINT('',#53742);
#5807=VERTEX_POINT('',#53744);
#5808=VERTEX_POINT('',#53748);
#5809=VERTEX_POINT('',#53750);
#5810=VERTEX_POINT('',#53754);
#5811=VERTEX_POINT('',#53756);
#5812=VERTEX_POINT('',#53760);
#5813=VERTEX_POINT('',#53762);
#5814=VERTEX_POINT('',#53770);
#5815=VERTEX_POINT('',#53773);
#5816=VERTEX_POINT('',#53777);
#5817=VERTEX_POINT('',#53781);
#5818=EDGE_CURVE('',#4784,#4784,#4259,.T.);
#5819=EDGE_CURVE('',#4784,#4785,#2977,.T.);
#5820=EDGE_CURVE('',#4785,#4785,#4260,.T.);
#5821=EDGE_CURVE('',#4786,#4786,#4261,.T.);
#5822=EDGE_CURVE('',#4786,#4787,#2978,.T.);
#5823=EDGE_CURVE('',#4787,#4787,#4262,.T.);
#5824=EDGE_CURVE('',#4788,#4788,#4263,.T.);
#5825=EDGE_CURVE('',#4788,#4789,#2979,.T.);
#5826=EDGE_CURVE('',#4789,#4789,#4264,.T.);
#5827=EDGE_CURVE('',#4790,#4790,#4265,.T.);
#5828=EDGE_CURVE('',#4790,#4791,#2980,.T.);
#5829=EDGE_CURVE('',#4791,#4791,#4266,.T.);
#5830=EDGE_CURVE('',#4792,#4793,#2981,.T.);
#5831=EDGE_CURVE('',#4793,#4794,#2982,.T.);
#5832=EDGE_CURVE('',#4795,#4794,#2983,.T.);
#5833=EDGE_CURVE('',#4792,#4795,#2984,.T.);
#5834=EDGE_CURVE('',#4796,#4792,#2985,.T.);
#5835=EDGE_CURVE('',#4797,#4795,#2986,.T.);
#5836=EDGE_CURVE('',#4796,#4797,#2987,.T.);
#5837=EDGE_CURVE('',#4798,#4796,#2988,.T.);
#5838=EDGE_CURVE('',#4799,#4797,#2989,.T.);
#5839=EDGE_CURVE('',#4798,#4799,#2990,.T.);
#5840=EDGE_CURVE('',#4793,#4798,#2991,.T.);
#5841=EDGE_CURVE('',#4794,#4799,#2992,.T.);
#5842=EDGE_CURVE('',#4800,#4800,#4267,.T.);
#5843=EDGE_CURVE('',#4800,#4801,#2993,.T.);
#5844=EDGE_CURVE('',#4801,#4801,#4268,.T.);
#5845=EDGE_CURVE('',#4802,#4802,#4269,.T.);
#5846=EDGE_CURVE('',#4802,#4803,#2994,.T.);
#5847=EDGE_CURVE('',#4803,#4803,#4270,.T.);
#5848=EDGE_CURVE('',#4804,#4804,#4271,.T.);
#5849=EDGE_CURVE('',#4804,#4805,#2995,.T.);
#5850=EDGE_CURVE('',#4805,#4805,#4272,.T.);
#5851=EDGE_CURVE('',#4806,#4806,#4273,.T.);
#5852=EDGE_CURVE('',#4806,#4807,#2996,.T.);
#5853=EDGE_CURVE('',#4807,#4807,#4274,.T.);
#5854=EDGE_CURVE('',#4808,#4808,#4275,.T.);
#5855=EDGE_CURVE('',#4808,#4809,#2997,.T.);
#5856=EDGE_CURVE('',#4809,#4809,#4276,.T.);
#5857=EDGE_CURVE('',#4810,#4810,#4277,.T.);
#5858=EDGE_CURVE('',#4810,#4811,#2998,.T.);
#5859=EDGE_CURVE('',#4811,#4811,#4278,.T.);
#5860=EDGE_CURVE('',#4812,#4812,#4279,.T.);
#5861=EDGE_CURVE('',#4812,#4813,#2999,.T.);
#5862=EDGE_CURVE('',#4813,#4813,#4280,.T.);
#5863=EDGE_CURVE('',#4814,#4814,#4281,.T.);
#5864=EDGE_CURVE('',#4815,#4815,#4282,.T.);
#5865=EDGE_CURVE('',#4815,#4816,#3000,.T.);
#5866=EDGE_CURVE('',#4816,#4816,#4283,.T.);
#5867=EDGE_CURVE('',#4817,#4817,#4284,.T.);
#5868=EDGE_CURVE('',#4818,#4818,#4285,.T.);
#5869=EDGE_CURVE('',#4818,#4819,#3001,.T.);
#5870=EDGE_CURVE('',#4819,#4819,#4286,.T.);
#5871=EDGE_CURVE('',#4820,#4820,#4287,.T.);
#5872=EDGE_CURVE('',#4821,#4821,#4288,.T.);
#5873=EDGE_CURVE('',#4821,#4822,#3002,.T.);
#5874=EDGE_CURVE('',#4822,#4822,#4289,.T.);
#5875=EDGE_CURVE('',#4823,#4823,#4290,.T.);
#5876=EDGE_CURVE('',#4814,#4824,#3003,.T.);
#5877=EDGE_CURVE('',#4824,#4824,#4291,.T.);
#5878=EDGE_CURVE('',#4817,#4825,#3004,.T.);
#5879=EDGE_CURVE('',#4825,#4825,#4292,.T.);
#5880=EDGE_CURVE('',#4820,#4826,#3005,.T.);
#5881=EDGE_CURVE('',#4826,#4826,#4293,.T.);
#5882=EDGE_CURVE('',#4823,#4827,#3006,.T.);
#5883=EDGE_CURVE('',#4827,#4827,#4294,.T.);
#5884=EDGE_CURVE('',#4828,#4828,#4295,.T.);
#5885=EDGE_CURVE('',#4828,#4829,#3007,.T.);
#5886=EDGE_CURVE('',#4829,#4829,#4296,.T.);
#5887=EDGE_CURVE('',#4830,#4830,#4297,.T.);
#5888=EDGE_CURVE('',#4830,#4831,#3008,.T.);
#5889=EDGE_CURVE('',#4831,#4831,#4298,.T.);
#5890=EDGE_CURVE('',#4832,#4832,#4299,.T.);
#5891=EDGE_CURVE('',#4832,#4833,#3009,.T.);
#5892=EDGE_CURVE('',#4833,#4833,#4300,.T.);
#5893=EDGE_CURVE('',#4834,#4834,#4301,.T.);
#5894=EDGE_CURVE('',#4834,#4835,#3010,.T.);
#5895=EDGE_CURVE('',#4835,#4835,#4302,.T.);
#5896=EDGE_CURVE('',#4836,#4836,#4303,.T.);
#5897=EDGE_CURVE('',#4836,#4837,#3011,.T.);
#5898=EDGE_CURVE('',#4837,#4837,#4304,.T.);
#5899=EDGE_CURVE('',#4838,#4838,#4305,.T.);
#5900=EDGE_CURVE('',#4838,#4839,#3012,.T.);
#5901=EDGE_CURVE('',#4839,#4839,#4306,.T.);
#5902=EDGE_CURVE('',#4840,#4841,#3013,.T.);
#5903=EDGE_CURVE('',#4841,#4842,#3014,.T.);
#5904=EDGE_CURVE('',#4843,#4842,#3015,.T.);
#5905=EDGE_CURVE('',#4840,#4843,#3016,.T.);
#5906=EDGE_CURVE('',#4844,#4840,#3017,.T.);
#5907=EDGE_CURVE('',#4845,#4843,#3018,.T.);
#5908=EDGE_CURVE('',#4844,#4845,#3019,.T.);
#5909=EDGE_CURVE('',#4846,#4844,#3020,.T.);
#5910=EDGE_CURVE('',#4847,#4845,#3021,.T.);
#5911=EDGE_CURVE('',#4846,#4847,#3022,.T.);
#5912=EDGE_CURVE('',#4841,#4846,#3023,.T.);
#5913=EDGE_CURVE('',#4842,#4847,#3024,.T.);
#5914=EDGE_CURVE('',#4848,#4848,#4307,.T.);
#5915=EDGE_CURVE('',#4848,#4849,#3025,.T.);
#5916=EDGE_CURVE('',#4849,#4849,#4308,.T.);
#5917=EDGE_CURVE('',#4850,#4850,#4309,.T.);
#5918=EDGE_CURVE('',#4850,#4851,#3026,.T.);
#5919=EDGE_CURVE('',#4851,#4851,#4310,.T.);
#5920=EDGE_CURVE('',#4852,#4852,#4311,.T.);
#5921=EDGE_CURVE('',#4852,#4853,#3027,.T.);
#5922=EDGE_CURVE('',#4853,#4853,#4312,.T.);
#5923=EDGE_CURVE('',#4854,#4854,#4313,.T.);
#5924=EDGE_CURVE('',#4854,#4855,#3028,.T.);
#5925=EDGE_CURVE('',#4855,#4855,#4314,.T.);
#5926=EDGE_CURVE('',#4856,#4856,#4315,.T.);
#5927=EDGE_CURVE('',#4856,#4857,#3029,.T.);
#5928=EDGE_CURVE('',#4857,#4857,#4316,.T.);
#5929=EDGE_CURVE('',#4858,#4858,#4317,.T.);
#5930=EDGE_CURVE('',#4858,#4859,#3030,.T.);
#5931=EDGE_CURVE('',#4859,#4859,#4318,.T.);
#5932=EDGE_CURVE('',#4860,#4860,#4319,.T.);
#5933=EDGE_CURVE('',#4860,#4861,#3031,.T.);
#5934=EDGE_CURVE('',#4861,#4861,#4320,.T.);
#5935=EDGE_CURVE('',#4862,#4862,#4321,.T.);
#5936=EDGE_CURVE('',#4863,#4863,#4322,.T.);
#5937=EDGE_CURVE('',#4863,#4864,#3032,.T.);
#5938=EDGE_CURVE('',#4864,#4864,#4323,.T.);
#5939=EDGE_CURVE('',#4865,#4865,#4324,.T.);
#5940=EDGE_CURVE('',#4866,#4866,#4325,.T.);
#5941=EDGE_CURVE('',#4866,#4867,#3033,.T.);
#5942=EDGE_CURVE('',#4867,#4867,#4326,.T.);
#5943=EDGE_CURVE('',#4868,#4868,#4327,.T.);
#5944=EDGE_CURVE('',#4869,#4869,#4328,.T.);
#5945=EDGE_CURVE('',#4869,#4870,#3034,.T.);
#5946=EDGE_CURVE('',#4870,#4870,#4329,.T.);
#5947=EDGE_CURVE('',#4871,#4871,#4330,.T.);
#5948=EDGE_CURVE('',#4872,#4872,#4331,.T.);
#5949=EDGE_CURVE('',#4872,#4862,#3035,.T.);
#5950=EDGE_CURVE('',#4873,#4873,#4332,.T.);
#5951=EDGE_CURVE('',#4873,#4865,#3036,.T.);
#5952=EDGE_CURVE('',#4874,#4874,#4333,.T.);
#5953=EDGE_CURVE('',#4874,#4868,#3037,.T.);
#5954=EDGE_CURVE('',#4875,#4875,#4334,.T.);
#5955=EDGE_CURVE('',#4875,#4871,#3038,.T.);
#5956=EDGE_CURVE('',#4876,#4876,#4335,.T.);
#5957=EDGE_CURVE('',#4876,#4877,#3039,.T.);
#5958=EDGE_CURVE('',#4877,#4877,#4336,.T.);
#5959=EDGE_CURVE('',#4878,#4878,#4337,.T.);
#5960=EDGE_CURVE('',#4878,#4879,#3040,.T.);
#5961=EDGE_CURVE('',#4879,#4879,#4338,.T.);
#5962=EDGE_CURVE('',#4880,#4880,#4339,.T.);
#5963=EDGE_CURVE('',#4880,#4881,#3041,.T.);
#5964=EDGE_CURVE('',#4881,#4881,#4340,.T.);
#5965=EDGE_CURVE('',#4882,#4882,#4341,.T.);
#5966=EDGE_CURVE('',#4883,#4883,#4342,.T.);
#5967=EDGE_CURVE('',#4883,#4882,#3042,.T.);
#5968=EDGE_CURVE('',#4884,#4884,#4343,.T.);
#5969=EDGE_CURVE('',#4884,#4885,#3043,.T.);
#5970=EDGE_CURVE('',#4885,#4885,#4344,.T.);
#5971=EDGE_CURVE('',#4886,#4886,#4345,.T.);
#5972=EDGE_CURVE('',#4887,#4887,#4346,.T.);
#5973=EDGE_CURVE('',#4887,#4886,#3044,.T.);
#5974=EDGE_CURVE('',#4888,#4889,#3045,.T.);
#5975=EDGE_CURVE('',#4889,#4890,#3046,.T.);
#5976=EDGE_CURVE('',#4891,#4890,#3047,.T.);
#5977=EDGE_CURVE('',#4888,#4891,#3048,.T.);
#5978=EDGE_CURVE('',#4892,#4888,#3049,.T.);
#5979=EDGE_CURVE('',#4893,#4891,#3050,.T.);
#5980=EDGE_CURVE('',#4892,#4893,#3051,.T.);
#5981=EDGE_CURVE('',#4894,#4892,#3052,.T.);
#5982=EDGE_CURVE('',#4895,#4893,#3053,.T.);
#5983=EDGE_CURVE('',#4894,#4895,#3054,.T.);
#5984=EDGE_CURVE('',#4889,#4894,#3055,.T.);
#5985=EDGE_CURVE('',#4890,#4895,#3056,.T.);
#5986=EDGE_CURVE('',#4896,#4896,#4347,.T.);
#5987=EDGE_CURVE('',#4896,#4897,#3057,.T.);
#5988=EDGE_CURVE('',#4897,#4897,#4348,.T.);
#5989=EDGE_CURVE('',#4898,#4898,#4349,.T.);
#5990=EDGE_CURVE('',#4898,#4899,#3058,.T.);
#5991=EDGE_CURVE('',#4899,#4899,#4350,.T.);
#5992=EDGE_CURVE('',#4900,#4900,#4351,.T.);
#5993=EDGE_CURVE('',#4900,#4901,#3059,.T.);
#5994=EDGE_CURVE('',#4901,#4901,#4352,.T.);
#5995=EDGE_CURVE('',#4902,#4902,#4353,.T.);
#5996=EDGE_CURVE('',#4902,#4903,#3060,.T.);
#5997=EDGE_CURVE('',#4903,#4903,#4354,.T.);
#5998=EDGE_CURVE('',#4904,#4904,#4355,.T.);
#5999=EDGE_CURVE('',#4904,#4905,#3061,.T.);
#6000=EDGE_CURVE('',#4905,#4905,#4356,.T.);
#6001=EDGE_CURVE('',#4906,#4906,#4357,.T.);
#6002=EDGE_CURVE('',#4906,#4907,#3062,.T.);
#6003=EDGE_CURVE('',#4907,#4907,#4358,.T.);
#6004=EDGE_CURVE('',#4908,#4908,#4359,.T.);
#6005=EDGE_CURVE('',#4908,#4909,#3063,.T.);
#6006=EDGE_CURVE('',#4909,#4909,#4360,.T.);
#6007=EDGE_CURVE('',#4910,#4910,#4361,.T.);
#6008=EDGE_CURVE('',#4910,#4911,#3064,.T.);
#6009=EDGE_CURVE('',#4911,#4911,#4362,.T.);
#6010=EDGE_CURVE('',#4912,#4912,#4363,.T.);
#6011=EDGE_CURVE('',#4912,#4913,#3065,.T.);
#6012=EDGE_CURVE('',#4913,#4913,#4364,.T.);
#6013=EDGE_CURVE('',#4914,#4914,#4365,.T.);
#6014=EDGE_CURVE('',#4914,#4915,#3066,.T.);
#6015=EDGE_CURVE('',#4915,#4915,#4366,.T.);
#6016=EDGE_CURVE('',#4916,#4916,#4367,.T.);
#6017=EDGE_CURVE('',#4916,#4917,#3067,.T.);
#6018=EDGE_CURVE('',#4917,#4917,#4368,.T.);
#6019=EDGE_CURVE('',#4918,#4918,#4369,.T.);
#6020=EDGE_CURVE('',#4918,#4919,#3068,.T.);
#6021=EDGE_CURVE('',#4919,#4919,#4370,.T.);
#6022=EDGE_CURVE('',#4920,#4920,#4371,.T.);
#6023=EDGE_CURVE('',#4920,#4921,#3069,.T.);
#6024=EDGE_CURVE('',#4921,#4921,#4372,.T.);
#6025=EDGE_CURVE('',#4922,#4922,#4373,.T.);
#6026=EDGE_CURVE('',#4922,#4923,#3070,.T.);
#6027=EDGE_CURVE('',#4923,#4923,#4374,.T.);
#6028=EDGE_CURVE('',#4924,#4924,#4375,.T.);
#6029=EDGE_CURVE('',#4924,#4925,#3071,.T.);
#6030=EDGE_CURVE('',#4925,#4925,#4376,.T.);
#6031=EDGE_CURVE('',#4926,#4926,#4377,.T.);
#6032=EDGE_CURVE('',#4926,#4927,#3072,.T.);
#6033=EDGE_CURVE('',#4927,#4927,#4378,.T.);
#6034=EDGE_CURVE('',#4928,#4928,#4379,.T.);
#6035=EDGE_CURVE('',#4928,#4929,#3073,.T.);
#6036=EDGE_CURVE('',#4929,#4929,#4380,.T.);
#6037=EDGE_CURVE('',#4930,#4930,#4381,.T.);
#6038=EDGE_CURVE('',#4930,#4931,#3074,.T.);
#6039=EDGE_CURVE('',#4931,#4931,#4382,.T.);
#6040=EDGE_CURVE('',#4932,#4932,#4383,.T.);
#6041=EDGE_CURVE('',#4932,#4933,#3075,.T.);
#6042=EDGE_CURVE('',#4933,#4933,#4384,.T.);
#6043=EDGE_CURVE('',#4934,#4934,#4385,.T.);
#6044=EDGE_CURVE('',#4934,#4935,#3076,.T.);
#6045=EDGE_CURVE('',#4935,#4935,#4386,.T.);
#6046=EDGE_CURVE('',#4936,#4936,#4387,.T.);
#6047=EDGE_CURVE('',#4936,#4937,#3077,.T.);
#6048=EDGE_CURVE('',#4937,#4937,#4388,.T.);
#6049=EDGE_CURVE('',#4938,#4938,#4389,.T.);
#6050=EDGE_CURVE('',#4938,#4939,#3078,.T.);
#6051=EDGE_CURVE('',#4939,#4939,#4390,.T.);
#6052=EDGE_CURVE('',#4940,#4940,#4391,.T.);
#6053=EDGE_CURVE('',#4940,#4941,#3079,.T.);
#6054=EDGE_CURVE('',#4941,#4941,#4392,.T.);
#6055=EDGE_CURVE('',#4942,#4942,#4393,.T.);
#6056=EDGE_CURVE('',#4942,#4943,#3080,.T.);
#6057=EDGE_CURVE('',#4943,#4943,#4394,.T.);
#6058=EDGE_CURVE('',#4944,#4944,#4395,.T.);
#6059=EDGE_CURVE('',#4945,#4945,#4396,.T.);
#6060=EDGE_CURVE('',#4945,#4944,#3081,.T.);
#6061=EDGE_CURVE('',#4946,#4946,#4397,.T.);
#6062=EDGE_CURVE('',#4946,#4947,#3082,.T.);
#6063=EDGE_CURVE('',#4947,#4947,#4398,.T.);
#6064=EDGE_CURVE('',#4948,#4948,#4399,.T.);
#6065=EDGE_CURVE('',#4948,#4949,#3083,.T.);
#6066=EDGE_CURVE('',#4949,#4949,#4400,.T.);
#6067=EDGE_CURVE('',#4950,#4950,#4401,.T.);
#6068=EDGE_CURVE('',#4950,#4951,#3084,.T.);
#6069=EDGE_CURVE('',#4951,#4951,#4402,.T.);
#6070=EDGE_CURVE('',#4952,#4952,#4403,.T.);
#6071=EDGE_CURVE('',#4952,#4953,#3085,.T.);
#6072=EDGE_CURVE('',#4953,#4953,#4404,.T.);
#6073=EDGE_CURVE('',#4954,#4954,#4405,.T.);
#6074=EDGE_CURVE('',#4954,#4955,#3086,.T.);
#6075=EDGE_CURVE('',#4955,#4955,#4406,.T.);
#6076=EDGE_CURVE('',#4956,#4956,#4407,.T.);
#6077=EDGE_CURVE('',#4957,#4957,#4408,.T.);
#6078=EDGE_CURVE('',#4957,#4956,#3087,.T.);
#6079=EDGE_CURVE('',#4958,#4958,#4409,.T.);
#6080=EDGE_CURVE('',#4958,#4959,#3088,.T.);
#6081=EDGE_CURVE('',#4959,#4959,#4410,.T.);
#6082=EDGE_CURVE('',#4960,#4960,#4411,.T.);
#6083=EDGE_CURVE('',#4961,#4961,#4412,.T.);
#6084=EDGE_CURVE('',#4961,#4960,#3089,.T.);
#6085=EDGE_CURVE('',#4962,#4962,#4413,.T.);
#6086=EDGE_CURVE('',#4962,#4961,#3090,.T.);
#6087=EDGE_CURVE('',#4963,#4963,#4414,.T.);
#6088=EDGE_CURVE('',#4963,#4962,#3091,.T.);
#6089=EDGE_CURVE('',#4964,#4964,#4415,.T.);
#6090=EDGE_CURVE('',#4965,#4965,#4416,.F.);
#6091=EDGE_CURVE('',#4965,#4964,#3092,.T.);
#6092=EDGE_CURVE('',#4966,#4966,#4417,.F.);
#6093=EDGE_CURVE('',#4966,#4965,#3093,.T.);
#6094=EDGE_CURVE('',#4967,#4967,#4418,.T.);
#6095=EDGE_CURVE('',#4967,#4966,#3094,.T.);
#6096=EDGE_CURVE('',#4968,#4969,#3095,.T.);
#6097=EDGE_CURVE('',#4969,#4970,#3096,.T.);
#6098=EDGE_CURVE('',#4970,#4971,#3097,.T.);
#6099=EDGE_CURVE('',#4968,#4971,#3098,.T.);
#6100=EDGE_CURVE('',#4969,#4972,#3099,.T.);
#6101=EDGE_CURVE('',#4972,#4973,#3100,.T.);
#6102=EDGE_CURVE('',#4973,#4970,#3101,.T.);
#6103=EDGE_CURVE('',#4972,#4974,#3102,.T.);
#6104=EDGE_CURVE('',#4974,#4975,#3103,.T.);
#6105=EDGE_CURVE('',#4975,#4973,#3104,.T.);
#6106=EDGE_CURVE('',#4974,#4976,#3105,.T.);
#6107=EDGE_CURVE('',#4976,#4977,#3106,.T.);
#6108=EDGE_CURVE('',#4977,#4975,#3107,.T.);
#6109=EDGE_CURVE('',#4976,#4978,#3108,.T.);
#6110=EDGE_CURVE('',#4978,#4979,#3109,.T.);
#6111=EDGE_CURVE('',#4979,#4977,#3110,.T.);
#6112=EDGE_CURVE('',#4978,#4968,#3111,.T.);
#6113=EDGE_CURVE('',#4971,#4979,#3112,.T.);
#6114=EDGE_CURVE('',#4980,#4980,#4419,.T.);
#6115=EDGE_CURVE('',#4981,#4981,#4420,.T.);
#6116=EDGE_CURVE('',#4981,#4980,#3113,.T.);
#6117=EDGE_CURVE('',#4982,#4982,#4421,.T.);
#6118=EDGE_CURVE('',#4982,#4981,#3114,.T.);
#6119=EDGE_CURVE('',#4983,#4983,#4422,.T.);
#6120=EDGE_CURVE('',#4983,#4982,#3115,.T.);
#6121=EDGE_CURVE('',#4984,#4984,#4423,.T.);
#6122=EDGE_CURVE('',#4985,#4985,#4424,.F.);
#6123=EDGE_CURVE('',#4985,#4984,#3116,.T.);
#6124=EDGE_CURVE('',#4986,#4986,#4425,.F.);
#6125=EDGE_CURVE('',#4986,#4985,#3117,.T.);
#6126=EDGE_CURVE('',#4987,#4987,#4426,.T.);
#6127=EDGE_CURVE('',#4987,#4986,#3118,.T.);
#6128=EDGE_CURVE('',#4988,#4989,#3119,.T.);
#6129=EDGE_CURVE('',#4989,#4990,#3120,.T.);
#6130=EDGE_CURVE('',#4990,#4991,#3121,.T.);
#6131=EDGE_CURVE('',#4988,#4991,#3122,.T.);
#6132=EDGE_CURVE('',#4989,#4992,#3123,.T.);
#6133=EDGE_CURVE('',#4992,#4993,#3124,.T.);
#6134=EDGE_CURVE('',#4993,#4990,#3125,.T.);
#6135=EDGE_CURVE('',#4992,#4994,#3126,.T.);
#6136=EDGE_CURVE('',#4994,#4995,#3127,.T.);
#6137=EDGE_CURVE('',#4995,#4993,#3128,.T.);
#6138=EDGE_CURVE('',#4994,#4996,#3129,.T.);
#6139=EDGE_CURVE('',#4996,#4997,#3130,.T.);
#6140=EDGE_CURVE('',#4997,#4995,#3131,.T.);
#6141=EDGE_CURVE('',#4996,#4998,#3132,.T.);
#6142=EDGE_CURVE('',#4998,#4999,#3133,.T.);
#6143=EDGE_CURVE('',#4999,#4997,#3134,.T.);
#6144=EDGE_CURVE('',#4998,#4988,#3135,.T.);
#6145=EDGE_CURVE('',#4991,#4999,#3136,.T.);
#6146=EDGE_CURVE('',#5000,#5001,#4427,.T.);
#6147=EDGE_CURVE('',#5001,#5000,#4428,.T.);
#6148=EDGE_CURVE('',#5001,#5002,#4429,.T.);
#6149=EDGE_CURVE('',#5003,#5002,#4430,.T.);
#6150=EDGE_CURVE('',#5002,#5003,#4431,.T.);
#6151=EDGE_CURVE('',#5003,#5004,#3137,.T.);
#6152=EDGE_CURVE('',#5004,#5004,#4432,.T.);
#6153=EDGE_CURVE('',#5005,#5005,#4433,.T.);
#6154=EDGE_CURVE('',#5005,#5006,#3138,.T.);
#6155=EDGE_CURVE('',#5006,#5006,#4434,.T.);
#6156=EDGE_CURVE('',#5006,#5007,#3139,.T.);
#6157=EDGE_CURVE('',#5007,#5007,#4435,.T.);
#6158=EDGE_CURVE('',#5008,#5008,#4436,.T.);
#6159=EDGE_CURVE('',#5008,#5000,#3140,.T.);
#6160=EDGE_CURVE('',#5009,#5009,#4437,.T.);
#6161=EDGE_CURVE('',#5009,#5005,#3141,.T.);
#6162=EDGE_CURVE('',#5010,#5011,#4438,.T.);
#6163=EDGE_CURVE('',#5011,#5010,#4439,.T.);
#6164=EDGE_CURVE('',#5011,#5012,#4440,.T.);
#6165=EDGE_CURVE('',#5013,#5012,#4441,.T.);
#6166=EDGE_CURVE('',#5012,#5013,#4442,.T.);
#6167=EDGE_CURVE('',#5014,#5014,#4443,.T.);
#6168=EDGE_CURVE('',#5014,#5013,#3142,.T.);
#6169=EDGE_CURVE('',#5015,#5015,#4444,.T.);
#6170=EDGE_CURVE('',#5016,#5016,#4445,.T.);
#6171=EDGE_CURVE('',#5017,#5017,#4446,.T.);
#6172=EDGE_CURVE('',#5017,#5015,#3143,.T.);
#6173=EDGE_CURVE('',#5018,#5018,#4447,.T.);
#6174=EDGE_CURVE('',#5018,#5017,#3144,.T.);
#6175=EDGE_CURVE('',#5019,#5019,#4448,.T.);
#6176=EDGE_CURVE('',#5019,#5018,#3145,.T.);
#6177=EDGE_CURVE('',#5010,#5016,#3146,.T.);
#6178=EDGE_CURVE('',#5020,#5021,#4449,.T.);
#6179=EDGE_CURVE('',#5022,#5023,#4450,.T.);
#6180=EDGE_CURVE('',#5024,#5025,#4451,.T.);
#6181=EDGE_CURVE('',#5026,#5027,#4452,.T.);
#6182=EDGE_CURVE('',#5028,#5029,#4453,.T.);
#6183=EDGE_CURVE('',#5030,#5031,#4454,.T.);
#6184=EDGE_CURVE('',#5032,#5033,#4455,.T.);
#6185=EDGE_CURVE('',#5034,#5035,#667,.T.);
#6186=EDGE_CURVE('',#5036,#5034,#4456,.T.);
#6187=EDGE_CURVE('',#5037,#5036,#668,.T.);
#6188=EDGE_CURVE('',#5035,#5037,#4457,.T.);
#6189=EDGE_CURVE('',#5038,#5036,#4458,.T.);
#6190=EDGE_CURVE('',#5038,#5039,#669,.T.);
#6191=EDGE_CURVE('',#5040,#5039,#4459,.T.);
#6192=EDGE_CURVE('',#5040,#5041,#670,.T.);
#6193=EDGE_CURVE('',#5042,#5041,#4460,.T.);
#6194=EDGE_CURVE('',#5042,#5043,#3147,.T.);
#6195=EDGE_CURVE('',#5043,#5043,#4461,.T.);
#6196=EDGE_CURVE('',#5044,#5042,#4462,.T.);
#6197=EDGE_CURVE('',#5044,#5045,#671,.T.);
#6198=EDGE_CURVE('',#5046,#5045,#4463,.T.);
#6199=EDGE_CURVE('',#5046,#5047,#672,.T.);
#6200=EDGE_CURVE('',#5048,#5047,#4464,.T.);
#6201=EDGE_CURVE('',#5048,#5049,#673,.T.);
#6202=EDGE_CURVE('',#5050,#5049,#4465,.T.);
#6203=EDGE_CURVE('',#5050,#5051,#674,.T.);
#6204=EDGE_CURVE('',#5037,#5051,#4466,.T.);
#6205=EDGE_CURVE('',#5034,#5052,#4467,.T.);
#6206=EDGE_CURVE('',#5052,#5038,#4468,.T.);
#6207=EDGE_CURVE('',#5053,#5052,#675,.T.);
#6208=EDGE_CURVE('',#5039,#5053,#4469,.T.);
#6209=EDGE_CURVE('',#5053,#5054,#4470,.T.);
#6210=EDGE_CURVE('',#5054,#5040,#4471,.T.);
#6211=EDGE_CURVE('',#5055,#5054,#676,.T.);
#6212=EDGE_CURVE('',#5041,#5055,#4472,.T.);
#6213=EDGE_CURVE('',#5055,#5056,#4473,.T.);
#6214=EDGE_CURVE('',#5056,#5057,#4474,.T.);
#6215=EDGE_CURVE('',#5057,#5044,#4475,.T.);
#6216=EDGE_CURVE('',#5058,#5057,#677,.T.);
#6217=EDGE_CURVE('',#5045,#5058,#4476,.T.);
#6218=EDGE_CURVE('',#5058,#5059,#4477,.T.);
#6219=EDGE_CURVE('',#5059,#5046,#4478,.T.);
#6220=EDGE_CURVE('',#5060,#5059,#678,.T.);
#6221=EDGE_CURVE('',#5047,#5060,#4479,.T.);
#6222=EDGE_CURVE('',#5060,#5061,#4480,.T.);
#6223=EDGE_CURVE('',#5061,#5048,#4481,.T.);
#6224=EDGE_CURVE('',#5062,#5061,#679,.T.);
#6225=EDGE_CURVE('',#5049,#5062,#4482,.T.);
#6226=EDGE_CURVE('',#5063,#5063,#4483,.T.);
#6227=EDGE_CURVE('',#5063,#5056,#3148,.T.);
#6228=EDGE_CURVE('',#5064,#5035,#4484,.T.);
#6229=EDGE_CURVE('',#5064,#5065,#680,.T.);
#6230=EDGE_CURVE('',#5062,#5065,#4485,.T.);
#6231=EDGE_CURVE('',#5051,#5064,#4486,.T.);
#6232=EDGE_CURVE('',#5065,#5050,#4487,.T.);
#6233=EDGE_CURVE('',#5066,#5066,#4488,.T.);
#6234=EDGE_CURVE('',#5067,#5067,#4489,.T.);
#6235=EDGE_CURVE('',#5068,#5068,#4490,.T.);
#6236=EDGE_CURVE('',#5068,#5066,#3149,.T.);
#6237=EDGE_CURVE('',#5069,#5069,#4491,.T.);
#6238=EDGE_CURVE('',#5069,#5067,#3150,.T.);
#6239=EDGE_CURVE('',#5070,#5070,#4492,.T.);
#6240=EDGE_CURVE('',#5071,#5071,#4493,.T.);
#6241=EDGE_CURVE('',#5072,#5072,#4494,.T.);
#6242=EDGE_CURVE('',#5072,#5070,#3151,.T.);
#6243=EDGE_CURVE('',#5073,#5073,#4495,.T.);
#6244=EDGE_CURVE('',#5073,#5071,#3152,.T.);
#6245=EDGE_CURVE('',#5074,#5075,#4496,.T.);
#6246=EDGE_CURVE('',#5075,#5074,#4497,.T.);
#6247=EDGE_CURVE('',#5075,#5076,#4498,.T.);
#6248=EDGE_CURVE('',#5077,#5076,#4499,.T.);
#6249=EDGE_CURVE('',#5076,#5077,#4500,.T.);
#6250=EDGE_CURVE('',#5077,#5078,#3153,.T.);
#6251=EDGE_CURVE('',#5078,#5078,#4501,.T.);
#6252=EDGE_CURVE('',#5079,#5079,#4502,.T.);
#6253=EDGE_CURVE('',#5079,#5080,#3154,.T.);
#6254=EDGE_CURVE('',#5080,#5080,#4503,.T.);
#6255=EDGE_CURVE('',#5080,#5081,#3155,.T.);
#6256=EDGE_CURVE('',#5081,#5081,#4504,.T.);
#6257=EDGE_CURVE('',#5082,#5082,#4505,.T.);
#6258=EDGE_CURVE('',#5082,#5074,#3156,.T.);
#6259=EDGE_CURVE('',#5083,#5083,#4506,.T.);
#6260=EDGE_CURVE('',#5083,#5079,#3157,.T.);
#6261=EDGE_CURVE('',#5084,#5085,#4507,.T.);
#6262=EDGE_CURVE('',#5085,#5084,#4508,.T.);
#6263=EDGE_CURVE('',#5085,#5086,#4509,.T.);
#6264=EDGE_CURVE('',#5087,#5086,#4510,.T.);
#6265=EDGE_CURVE('',#5086,#5087,#4511,.T.);
#6266=EDGE_CURVE('',#5088,#5088,#4512,.T.);
#6267=EDGE_CURVE('',#5088,#5087,#3158,.T.);
#6268=EDGE_CURVE('',#5089,#5089,#4513,.T.);
#6269=EDGE_CURVE('',#5090,#5090,#4514,.T.);
#6270=EDGE_CURVE('',#5091,#5091,#4515,.T.);
#6271=EDGE_CURVE('',#5091,#5089,#3159,.T.);
#6272=EDGE_CURVE('',#5092,#5092,#4516,.T.);
#6273=EDGE_CURVE('',#5092,#5091,#3160,.T.);
#6274=EDGE_CURVE('',#5093,#5093,#4517,.T.);
#6275=EDGE_CURVE('',#5093,#5092,#3161,.T.);
#6276=EDGE_CURVE('',#5084,#5090,#3162,.T.);
#6277=EDGE_CURVE('',#5094,#5095,#4518,.T.);
#6278=EDGE_CURVE('',#5096,#5097,#4519,.T.);
#6279=EDGE_CURVE('',#5098,#5099,#4520,.T.);
#6280=EDGE_CURVE('',#5100,#5101,#4521,.T.);
#6281=EDGE_CURVE('',#5102,#5103,#4522,.T.);
#6282=EDGE_CURVE('',#5104,#5105,#4523,.T.);
#6283=EDGE_CURVE('',#5106,#5107,#4524,.T.);
#6284=EDGE_CURVE('',#5108,#5109,#4525,.T.);
#6285=EDGE_CURVE('',#5110,#5111,#681,.T.);
#6286=EDGE_CURVE('',#5112,#5110,#4526,.T.);
#6287=EDGE_CURVE('',#5113,#5112,#682,.T.);
#6288=EDGE_CURVE('',#5111,#5113,#4527,.T.);
#6289=EDGE_CURVE('',#5114,#5112,#4528,.T.);
#6290=EDGE_CURVE('',#5114,#5115,#683,.T.);
#6291=EDGE_CURVE('',#5116,#5115,#4529,.T.);
#6292=EDGE_CURVE('',#5116,#5117,#684,.T.);
#6293=EDGE_CURVE('',#5118,#5117,#4530,.T.);
#6294=EDGE_CURVE('',#5118,#5119,#685,.T.);
#6295=EDGE_CURVE('',#5119,#5120,#3163,.T.);
#6296=EDGE_CURVE('',#5120,#5120,#4531,.T.);
#6297=EDGE_CURVE('',#5119,#5121,#686,.T.);
#6298=EDGE_CURVE('',#5122,#5121,#4532,.T.);
#6299=EDGE_CURVE('',#5122,#5123,#687,.T.);
#6300=EDGE_CURVE('',#5124,#5123,#4533,.T.);
#6301=EDGE_CURVE('',#5124,#5125,#688,.T.);
#6302=EDGE_CURVE('',#5126,#5125,#4534,.T.);
#6303=EDGE_CURVE('',#5126,#5127,#689,.T.);
#6304=EDGE_CURVE('',#5128,#5127,#4535,.T.);
#6305=EDGE_CURVE('',#5128,#5129,#690,.T.);
#6306=EDGE_CURVE('',#5113,#5129,#4536,.T.);
#6307=EDGE_CURVE('',#5110,#5130,#4537,.T.);
#6308=EDGE_CURVE('',#5130,#5114,#4538,.T.);
#6309=EDGE_CURVE('',#5131,#5130,#691,.T.);
#6310=EDGE_CURVE('',#5115,#5131,#4539,.T.);
#6311=EDGE_CURVE('',#5131,#5132,#4540,.T.);
#6312=EDGE_CURVE('',#5132,#5116,#4541,.T.);
#6313=EDGE_CURVE('',#5133,#5132,#692,.T.);
#6314=EDGE_CURVE('',#5117,#5133,#4542,.T.);
#6315=EDGE_CURVE('',#5133,#5134,#4543,.T.);
#6316=EDGE_CURVE('',#5134,#5118,#4544,.T.);
#6317=EDGE_CURVE('',#5135,#5136,#693,.T.);
#6318=EDGE_CURVE('',#5121,#5135,#4545,.T.);
#6319=EDGE_CURVE('',#5136,#5134,#694,.T.);
#6320=EDGE_CURVE('',#5135,#5137,#4546,.T.);
#6321=EDGE_CURVE('',#5137,#5122,#4547,.T.);
#6322=EDGE_CURVE('',#5138,#5137,#695,.T.);
#6323=EDGE_CURVE('',#5123,#5138,#4548,.T.);
#6324=EDGE_CURVE('',#5138,#5139,#4549,.T.);
#6325=EDGE_CURVE('',#5139,#5124,#4550,.T.);
#6326=EDGE_CURVE('',#5140,#5139,#696,.T.);
#6327=EDGE_CURVE('',#5125,#5140,#4551,.T.);
#6328=EDGE_CURVE('',#5140,#5141,#4552,.T.);
#6329=EDGE_CURVE('',#5141,#5126,#4553,.T.);
#6330=EDGE_CURVE('',#5142,#5141,#697,.T.);
#6331=EDGE_CURVE('',#5127,#5142,#4554,.T.);
#6332=EDGE_CURVE('',#5143,#5143,#4555,.T.);
#6333=EDGE_CURVE('',#5143,#5136,#3164,.T.);
#6334=EDGE_CURVE('',#5144,#5111,#4556,.T.);
#6335=EDGE_CURVE('',#5144,#5145,#698,.T.);
#6336=EDGE_CURVE('',#5142,#5145,#4557,.T.);
#6337=EDGE_CURVE('',#5129,#5144,#4558,.T.);
#6338=EDGE_CURVE('',#5145,#5128,#4559,.T.);
#6339=EDGE_CURVE('',#5146,#5146,#4560,.T.);
#6340=EDGE_CURVE('',#5147,#5147,#4561,.T.);
#6341=EDGE_CURVE('',#5148,#5148,#4562,.T.);
#6342=EDGE_CURVE('',#5148,#5146,#3165,.T.);
#6343=EDGE_CURVE('',#5149,#5149,#4563,.T.);
#6344=EDGE_CURVE('',#5149,#5147,#3166,.T.);
#6345=EDGE_CURVE('',#5150,#5150,#4564,.T.);
#6346=EDGE_CURVE('',#5151,#5151,#4565,.T.);
#6347=EDGE_CURVE('',#5152,#5152,#4566,.T.);
#6348=EDGE_CURVE('',#5152,#5150,#3167,.T.);
#6349=EDGE_CURVE('',#5153,#5153,#4567,.T.);
#6350=EDGE_CURVE('',#5153,#5151,#3168,.T.);
#6351=EDGE_CURVE('',#5154,#5154,#4568,.T.);
#6352=EDGE_CURVE('',#5155,#5155,#4569,.T.);
#6353=EDGE_CURVE('',#5155,#5154,#3169,.T.);
#6354=EDGE_CURVE('',#5156,#5156,#4570,.T.);
#6355=EDGE_CURVE('',#5156,#5155,#3170,.T.);
#6356=EDGE_CURVE('',#5157,#5157,#4571,.T.);
#6357=EDGE_CURVE('',#5157,#5156,#3171,.T.);
#6358=EDGE_CURVE('',#5158,#5158,#4572,.T.);
#6359=EDGE_CURVE('',#5159,#5159,#4573,.F.);
#6360=EDGE_CURVE('',#5159,#5158,#3172,.T.);
#6361=EDGE_CURVE('',#5160,#5160,#4574,.F.);
#6362=EDGE_CURVE('',#5160,#5159,#3173,.T.);
#6363=EDGE_CURVE('',#5161,#5161,#4575,.T.);
#6364=EDGE_CURVE('',#5161,#5160,#3174,.T.);
#6365=EDGE_CURVE('',#5162,#5163,#3175,.T.);
#6366=EDGE_CURVE('',#5163,#5164,#3176,.T.);
#6367=EDGE_CURVE('',#5164,#5165,#3177,.T.);
#6368=EDGE_CURVE('',#5162,#5165,#3178,.T.);
#6369=EDGE_CURVE('',#5163,#5166,#3179,.T.);
#6370=EDGE_CURVE('',#5166,#5167,#3180,.T.);
#6371=EDGE_CURVE('',#5167,#5164,#3181,.T.);
#6372=EDGE_CURVE('',#5166,#5168,#3182,.T.);
#6373=EDGE_CURVE('',#5168,#5169,#3183,.T.);
#6374=EDGE_CURVE('',#5169,#5167,#3184,.T.);
#6375=EDGE_CURVE('',#5168,#5170,#3185,.T.);
#6376=EDGE_CURVE('',#5170,#5171,#3186,.T.);
#6377=EDGE_CURVE('',#5171,#5169,#3187,.T.);
#6378=EDGE_CURVE('',#5170,#5172,#3188,.T.);
#6379=EDGE_CURVE('',#5172,#5173,#3189,.T.);
#6380=EDGE_CURVE('',#5173,#5171,#3190,.T.);
#6381=EDGE_CURVE('',#5172,#5162,#3191,.T.);
#6382=EDGE_CURVE('',#5165,#5173,#3192,.T.);
#6383=EDGE_CURVE('',#5174,#5175,#3193,.T.);
#6384=EDGE_CURVE('',#5174,#5176,#3194,.T.);
#6385=EDGE_CURVE('',#5177,#5176,#3195,.T.);
#6386=EDGE_CURVE('',#5177,#5175,#3196,.T.);
#6387=EDGE_CURVE('',#5175,#5178,#4576,.T.);
#6388=EDGE_CURVE('',#5179,#5177,#3197,.T.);
#6389=EDGE_CURVE('',#5178,#5179,#3198,.T.);
#6390=EDGE_CURVE('',#5178,#5180,#3199,.T.);
#6391=EDGE_CURVE('',#5179,#5181,#3200,.T.);
#6392=EDGE_CURVE('',#5181,#5180,#3201,.T.);
#6393=EDGE_CURVE('',#5176,#5181,#3202,.T.);
#6394=EDGE_CURVE('',#5180,#5174,#4577,.T.);
#6395=EDGE_CURVE('',#5182,#5182,#4578,.T.);
#6396=EDGE_CURVE('',#5182,#5183,#3203,.T.);
#6397=EDGE_CURVE('',#5183,#5183,#4579,.T.);
#6398=EDGE_CURVE('',#5184,#5184,#4580,.T.);
#6399=EDGE_CURVE('',#5184,#5185,#3204,.T.);
#6400=EDGE_CURVE('',#5185,#5185,#4581,.T.);
#6401=EDGE_CURVE('',#5186,#5186,#4582,.T.);
#6402=EDGE_CURVE('',#5186,#5187,#3205,.T.);
#6403=EDGE_CURVE('',#5187,#5187,#4583,.T.);
#6404=EDGE_CURVE('',#5188,#5188,#4584,.T.);
#6405=EDGE_CURVE('',#5188,#5189,#3206,.T.);
#6406=EDGE_CURVE('',#5189,#5189,#4585,.T.);
#6407=EDGE_CURVE('',#5190,#5190,#4586,.T.);
#6408=EDGE_CURVE('',#5190,#5191,#3207,.T.);
#6409=EDGE_CURVE('',#5191,#5191,#4587,.T.);
#6410=EDGE_CURVE('',#5192,#5193,#3208,.T.);
#6411=EDGE_CURVE('',#5192,#5193,#4588,.T.);
#6412=EDGE_CURVE('',#5194,#5192,#699,.T.);
#6413=EDGE_CURVE('',#5195,#5194,#4589,.T.);
#6414=EDGE_CURVE('',#5195,#5196,#3209,.T.);
#6415=EDGE_CURVE('',#5197,#5196,#700,.T.);
#6416=EDGE_CURVE('',#5196,#5197,#701,.T.);
#6417=EDGE_CURVE('',#5198,#5195,#4590,.T.);
#6418=EDGE_CURVE('',#5193,#5198,#702,.T.);
#6419=EDGE_CURVE('',#5198,#5194,#3210,.T.);
#6420=EDGE_CURVE('',#5199,#5199,#4591,.T.);
#6421=EDGE_CURVE('',#5199,#5200,#3211,.T.);
#6422=EDGE_CURVE('',#5200,#5200,#4592,.T.);
#6423=EDGE_CURVE('',#5201,#5201,#4593,.T.);
#6424=EDGE_CURVE('',#5201,#5202,#3212,.T.);
#6425=EDGE_CURVE('',#5202,#5202,#4594,.T.);
#6426=EDGE_CURVE('',#5203,#5203,#4595,.T.);
#6427=EDGE_CURVE('',#5203,#5204,#3213,.T.);
#6428=EDGE_CURVE('',#5204,#5204,#4596,.T.);
#6429=EDGE_CURVE('',#5205,#5205,#4597,.T.);
#6430=EDGE_CURVE('',#5205,#5206,#3214,.T.);
#6431=EDGE_CURVE('',#5206,#5206,#4598,.T.);
#6432=EDGE_CURVE('',#5207,#5208,#3215,.T.);
#6433=EDGE_CURVE('',#5207,#5208,#4599,.T.);
#6434=EDGE_CURVE('',#5209,#5207,#703,.T.);
#6435=EDGE_CURVE('',#5210,#5209,#4600,.T.);
#6436=EDGE_CURVE('',#5210,#5211,#3216,.T.);
#6437=EDGE_CURVE('',#5212,#5211,#704,.T.);
#6438=EDGE_CURVE('',#5211,#5212,#705,.T.);
#6439=EDGE_CURVE('',#5213,#5210,#4601,.T.);
#6440=EDGE_CURVE('',#5208,#5213,#706,.T.);
#6441=EDGE_CURVE('',#5213,#5209,#3217,.T.);
#6442=EDGE_CURVE('',#5214,#5214,#4602,.T.);
#6443=EDGE_CURVE('',#5214,#5215,#3218,.T.);
#6444=EDGE_CURVE('',#5215,#5215,#4603,.T.);
#6445=EDGE_CURVE('',#5216,#5216,#4604,.T.);
#6446=EDGE_CURVE('',#5216,#5217,#3219,.T.);
#6447=EDGE_CURVE('',#5217,#5217,#4605,.T.);
#6448=EDGE_CURVE('',#5218,#5218,#4606,.T.);
#6449=EDGE_CURVE('',#5218,#5219,#3220,.T.);
#6450=EDGE_CURVE('',#5219,#5219,#4607,.T.);
#6451=EDGE_CURVE('',#5220,#5220,#4608,.T.);
#6452=EDGE_CURVE('',#5220,#5221,#3221,.T.);
#6453=EDGE_CURVE('',#5221,#5221,#4609,.T.);
#6454=EDGE_CURVE('',#5222,#5223,#3222,.T.);
#6455=EDGE_CURVE('',#5224,#5222,#3223,.T.);
#6456=EDGE_CURVE('',#5225,#5224,#3224,.T.);
#6457=EDGE_CURVE('',#5223,#5225,#3225,.T.);
#6458=EDGE_CURVE('',#5226,#5222,#3226,.T.);
#6459=EDGE_CURVE('',#5226,#5227,#3227,.T.);
#6460=EDGE_CURVE('',#5224,#5227,#3228,.T.);
#6461=EDGE_CURVE('',#5228,#5226,#3229,.T.);
#6462=EDGE_CURVE('',#5229,#5228,#3230,.T.);
#6463=EDGE_CURVE('',#5227,#5229,#3231,.T.);
#6464=EDGE_CURVE('',#5230,#5231,#4610,.T.);
#6465=EDGE_CURVE('',#5231,#5232,#131,.T.);
#6466=EDGE_CURVE('',#5232,#5233,#3232,.T.);
#6467=EDGE_CURVE('',#5233,#5234,#132,.T.);
#6468=EDGE_CURVE('',#5234,#5235,#4611,.T.);
#6469=EDGE_CURVE('',#5235,#5236,#133,.T.);
#6470=EDGE_CURVE('',#5236,#5237,#3233,.T.);
#6471=EDGE_CURVE('',#5237,#5238,#134,.T.);
#6472=EDGE_CURVE('',#5238,#5239,#4612,.T.);
#6473=EDGE_CURVE('',#5239,#5240,#135,.T.);
#6474=EDGE_CURVE('',#5240,#5241,#3234,.T.);
#6475=EDGE_CURVE('',#5241,#5242,#136,.T.);
#6476=EDGE_CURVE('',#5242,#5243,#4613,.T.);
#6477=EDGE_CURVE('',#5243,#5244,#137,.T.);
#6478=EDGE_CURVE('',#5244,#5245,#3235,.T.);
#6479=EDGE_CURVE('',#5245,#5246,#138,.T.);
#6480=EDGE_CURVE('',#5246,#5247,#4614,.T.);
#6481=EDGE_CURVE('',#5247,#5248,#139,.T.);
#6482=EDGE_CURVE('',#5248,#5249,#3236,.T.);
#6483=EDGE_CURVE('',#5249,#5250,#140,.T.);
#6484=EDGE_CURVE('',#5250,#5251,#4615,.T.);
#6485=EDGE_CURVE('',#5251,#5252,#141,.T.);
#6486=EDGE_CURVE('',#5252,#5253,#3237,.T.);
#6487=EDGE_CURVE('',#5253,#5254,#142,.T.);
#6488=EDGE_CURVE('',#5254,#5255,#4616,.T.);
#6489=EDGE_CURVE('',#5255,#5256,#143,.T.);
#6490=EDGE_CURVE('',#5256,#5257,#3238,.T.);
#6491=EDGE_CURVE('',#5257,#5258,#144,.T.);
#6492=EDGE_CURVE('',#5258,#5259,#4617,.T.);
#6493=EDGE_CURVE('',#5259,#5260,#145,.T.);
#6494=EDGE_CURVE('',#5260,#5261,#3239,.T.);
#6495=EDGE_CURVE('',#5261,#5262,#146,.T.);
#6496=EDGE_CURVE('',#5262,#5263,#4618,.T.);
#6497=EDGE_CURVE('',#5263,#5264,#147,.T.);
#6498=EDGE_CURVE('',#5264,#5265,#3240,.T.);
#6499=EDGE_CURVE('',#5265,#5266,#148,.T.);
#6500=EDGE_CURVE('',#5266,#5267,#4619,.T.);
#6501=EDGE_CURVE('',#5267,#5268,#149,.T.);
#6502=EDGE_CURVE('',#5268,#5269,#3241,.T.);
#6503=EDGE_CURVE('',#5269,#5270,#150,.T.);
#6504=EDGE_CURVE('',#5270,#5271,#4620,.T.);
#6505=EDGE_CURVE('',#5271,#5272,#151,.T.);
#6506=EDGE_CURVE('',#5272,#5273,#3242,.T.);
#6507=EDGE_CURVE('',#5273,#5274,#152,.T.);
#6508=EDGE_CURVE('',#5274,#5275,#4621,.T.);
#6509=EDGE_CURVE('',#5275,#5276,#153,.T.);
#6510=EDGE_CURVE('',#5276,#5277,#3243,.T.);
#6511=EDGE_CURVE('',#5277,#5278,#154,.T.);
#6512=EDGE_CURVE('',#5278,#5279,#4622,.T.);
#6513=EDGE_CURVE('',#5279,#5280,#155,.T.);
#6514=EDGE_CURVE('',#5280,#5281,#3244,.T.);
#6515=EDGE_CURVE('',#5281,#5282,#156,.T.);
#6516=EDGE_CURVE('',#5282,#5283,#4623,.T.);
#6517=EDGE_CURVE('',#5283,#5284,#157,.T.);
#6518=EDGE_CURVE('',#5284,#5285,#3245,.T.);
#6519=EDGE_CURVE('',#5285,#5286,#158,.T.);
#6520=EDGE_CURVE('',#5286,#5287,#4624,.T.);
#6521=EDGE_CURVE('',#5287,#5288,#159,.T.);
#6522=EDGE_CURVE('',#5288,#5289,#3246,.T.);
#6523=EDGE_CURVE('',#5289,#5290,#160,.T.);
#6524=EDGE_CURVE('',#5290,#5291,#4625,.T.);
#6525=EDGE_CURVE('',#5291,#5292,#161,.T.);
#6526=EDGE_CURVE('',#5292,#5293,#3247,.T.);
#6527=EDGE_CURVE('',#5293,#5294,#162,.T.);
#6528=EDGE_CURVE('',#5294,#5295,#4626,.T.);
#6529=EDGE_CURVE('',#5295,#5296,#163,.T.);
#6530=EDGE_CURVE('',#5296,#5297,#3248,.T.);
#6531=EDGE_CURVE('',#5297,#5298,#164,.T.);
#6532=EDGE_CURVE('',#5298,#5299,#4627,.T.);
#6533=EDGE_CURVE('',#5299,#5300,#165,.T.);
#6534=EDGE_CURVE('',#5300,#5301,#3249,.T.);
#6535=EDGE_CURVE('',#5301,#5302,#166,.T.);
#6536=EDGE_CURVE('',#5302,#5303,#4628,.T.);
#6537=EDGE_CURVE('',#5303,#5304,#167,.T.);
#6538=EDGE_CURVE('',#5304,#5305,#3250,.T.);
#6539=EDGE_CURVE('',#5305,#5306,#168,.T.);
#6540=EDGE_CURVE('',#5306,#5307,#4629,.T.);
#6541=EDGE_CURVE('',#5307,#5308,#169,.T.);
#6542=EDGE_CURVE('',#5308,#5309,#3251,.T.);
#6543=EDGE_CURVE('',#5309,#5230,#170,.T.);
#6544=EDGE_CURVE('',#5229,#5225,#4630,.T.);
#6545=EDGE_CURVE('',#5223,#5228,#4631,.T.);
#6546=EDGE_CURVE('',#5310,#5310,#4632,.T.);
#6547=EDGE_CURVE('',#5310,#5311,#3252,.T.);
#6548=EDGE_CURVE('',#5311,#5311,#4633,.T.);
#6549=EDGE_CURVE('',#5312,#5307,#3253,.T.);
#6550=EDGE_CURVE('',#5313,#5312,#171,.T.);
#6551=EDGE_CURVE('',#5308,#5313,#3254,.T.);
#6552=EDGE_CURVE('',#5314,#5313,#3255,.T.);
#6553=EDGE_CURVE('',#5309,#5314,#3256,.T.);
#6554=EDGE_CURVE('',#5315,#5314,#172,.T.);
#6555=EDGE_CURVE('',#5230,#5315,#3257,.T.);
#6556=EDGE_CURVE('',#5316,#5315,#4634,.T.);
#6557=EDGE_CURVE('',#5316,#5231,#3258,.T.);
#6558=EDGE_CURVE('',#5317,#5316,#173,.T.);
#6559=EDGE_CURVE('',#5232,#5317,#3259,.T.);
#6560=EDGE_CURVE('',#5318,#5317,#3260,.T.);
#6561=EDGE_CURVE('',#5233,#5318,#3261,.T.);
#6562=EDGE_CURVE('',#5319,#5318,#174,.T.);
#6563=EDGE_CURVE('',#5234,#5319,#3262,.T.);
#6564=EDGE_CURVE('',#5320,#5319,#4635,.T.);
#6565=EDGE_CURVE('',#5320,#5235,#3263,.T.);
#6566=EDGE_CURVE('',#5321,#5320,#175,.T.);
#6567=EDGE_CURVE('',#5236,#5321,#3264,.T.);
#6568=EDGE_CURVE('',#5322,#5321,#3265,.T.);
#6569=EDGE_CURVE('',#5237,#5322,#3266,.T.);
#6570=EDGE_CURVE('',#5323,#5322,#176,.T.);
#6571=EDGE_CURVE('',#5238,#5323,#3267,.T.);
#6572=EDGE_CURVE('',#5324,#5323,#4636,.T.);
#6573=EDGE_CURVE('',#5324,#5239,#3268,.T.);
#6574=EDGE_CURVE('',#5325,#5324,#177,.T.);
#6575=EDGE_CURVE('',#5240,#5325,#3269,.T.);
#6576=EDGE_CURVE('',#5326,#5325,#3270,.T.);
#6577=EDGE_CURVE('',#5241,#5326,#3271,.T.);
#6578=EDGE_CURVE('',#5327,#5326,#178,.T.);
#6579=EDGE_CURVE('',#5242,#5327,#3272,.T.);
#6580=EDGE_CURVE('',#5328,#5327,#4637,.T.);
#6581=EDGE_CURVE('',#5328,#5243,#3273,.T.);
#6582=EDGE_CURVE('',#5329,#5328,#179,.T.);
#6583=EDGE_CURVE('',#5244,#5329,#3274,.T.);
#6584=EDGE_CURVE('',#5330,#5329,#3275,.T.);
#6585=EDGE_CURVE('',#5245,#5330,#3276,.T.);
#6586=EDGE_CURVE('',#5331,#5330,#180,.T.);
#6587=EDGE_CURVE('',#5246,#5331,#3277,.T.);
#6588=EDGE_CURVE('',#5332,#5331,#4638,.T.);
#6589=EDGE_CURVE('',#5332,#5247,#3278,.T.);
#6590=EDGE_CURVE('',#5333,#5332,#181,.T.);
#6591=EDGE_CURVE('',#5248,#5333,#3279,.T.);
#6592=EDGE_CURVE('',#5334,#5333,#3280,.T.);
#6593=EDGE_CURVE('',#5249,#5334,#3281,.T.);
#6594=EDGE_CURVE('',#5335,#5334,#182,.T.);
#6595=EDGE_CURVE('',#5250,#5335,#3282,.T.);
#6596=EDGE_CURVE('',#5336,#5335,#4639,.T.);
#6597=EDGE_CURVE('',#5336,#5251,#3283,.T.);
#6598=EDGE_CURVE('',#5337,#5336,#183,.T.);
#6599=EDGE_CURVE('',#5252,#5337,#3284,.T.);
#6600=EDGE_CURVE('',#5338,#5337,#3285,.T.);
#6601=EDGE_CURVE('',#5253,#5338,#3286,.T.);
#6602=EDGE_CURVE('',#5339,#5338,#184,.T.);
#6603=EDGE_CURVE('',#5254,#5339,#3287,.T.);
#6604=EDGE_CURVE('',#5340,#5339,#4640,.T.);
#6605=EDGE_CURVE('',#5340,#5255,#3288,.T.);
#6606=EDGE_CURVE('',#5341,#5340,#185,.T.);
#6607=EDGE_CURVE('',#5256,#5341,#3289,.T.);
#6608=EDGE_CURVE('',#5342,#5341,#3290,.T.);
#6609=EDGE_CURVE('',#5257,#5342,#3291,.T.);
#6610=EDGE_CURVE('',#5343,#5342,#186,.T.);
#6611=EDGE_CURVE('',#5258,#5343,#3292,.T.);
#6612=EDGE_CURVE('',#5344,#5343,#4641,.T.);
#6613=EDGE_CURVE('',#5344,#5259,#3293,.T.);
#6614=EDGE_CURVE('',#5345,#5344,#187,.T.);
#6615=EDGE_CURVE('',#5260,#5345,#3294,.T.);
#6616=EDGE_CURVE('',#5346,#5345,#3295,.T.);
#6617=EDGE_CURVE('',#5261,#5346,#3296,.T.);
#6618=EDGE_CURVE('',#5347,#5346,#188,.T.);
#6619=EDGE_CURVE('',#5262,#5347,#3297,.T.);
#6620=EDGE_CURVE('',#5348,#5347,#4642,.T.);
#6621=EDGE_CURVE('',#5348,#5263,#3298,.T.);
#6622=EDGE_CURVE('',#5349,#5348,#189,.T.);
#6623=EDGE_CURVE('',#5264,#5349,#3299,.T.);
#6624=EDGE_CURVE('',#5350,#5349,#3300,.T.);
#6625=EDGE_CURVE('',#5265,#5350,#3301,.T.);
#6626=EDGE_CURVE('',#5351,#5350,#190,.T.);
#6627=EDGE_CURVE('',#5266,#5351,#3302,.T.);
#6628=EDGE_CURVE('',#5352,#5351,#4643,.T.);
#6629=EDGE_CURVE('',#5352,#5267,#3303,.T.);
#6630=EDGE_CURVE('',#5353,#5352,#191,.T.);
#6631=EDGE_CURVE('',#5268,#5353,#3304,.T.);
#6632=EDGE_CURVE('',#5354,#5353,#3305,.T.);
#6633=EDGE_CURVE('',#5269,#5354,#3306,.T.);
#6634=EDGE_CURVE('',#5355,#5354,#192,.T.);
#6635=EDGE_CURVE('',#5270,#5355,#3307,.T.);
#6636=EDGE_CURVE('',#5356,#5355,#4644,.T.);
#6637=EDGE_CURVE('',#5356,#5271,#3308,.T.);
#6638=EDGE_CURVE('',#5357,#5356,#193,.T.);
#6639=EDGE_CURVE('',#5272,#5357,#3309,.T.);
#6640=EDGE_CURVE('',#5358,#5357,#3310,.T.);
#6641=EDGE_CURVE('',#5273,#5358,#3311,.T.);
#6642=EDGE_CURVE('',#5359,#5358,#194,.T.);
#6643=EDGE_CURVE('',#5274,#5359,#3312,.T.);
#6644=EDGE_CURVE('',#5360,#5359,#4645,.T.);
#6645=EDGE_CURVE('',#5360,#5275,#3313,.T.);
#6646=EDGE_CURVE('',#5361,#5360,#195,.T.);
#6647=EDGE_CURVE('',#5276,#5361,#3314,.T.);
#6648=EDGE_CURVE('',#5362,#5361,#3315,.T.);
#6649=EDGE_CURVE('',#5277,#5362,#3316,.T.);
#6650=EDGE_CURVE('',#5363,#5362,#196,.T.);
#6651=EDGE_CURVE('',#5278,#5363,#3317,.T.);
#6652=EDGE_CURVE('',#5364,#5363,#4646,.T.);
#6653=EDGE_CURVE('',#5364,#5279,#3318,.T.);
#6654=EDGE_CURVE('',#5365,#5364,#197,.T.);
#6655=EDGE_CURVE('',#5280,#5365,#3319,.T.);
#6656=EDGE_CURVE('',#5366,#5365,#3320,.T.);
#6657=EDGE_CURVE('',#5281,#5366,#3321,.T.);
#6658=EDGE_CURVE('',#5367,#5366,#198,.T.);
#6659=EDGE_CURVE('',#5282,#5367,#3322,.T.);
#6660=EDGE_CURVE('',#5368,#5367,#4647,.T.);
#6661=EDGE_CURVE('',#5368,#5283,#3323,.T.);
#6662=EDGE_CURVE('',#5369,#5368,#199,.T.);
#6663=EDGE_CURVE('',#5284,#5369,#3324,.T.);
#6664=EDGE_CURVE('',#5370,#5369,#3325,.T.);
#6665=EDGE_CURVE('',#5285,#5370,#3326,.T.);
#6666=EDGE_CURVE('',#5371,#5370,#200,.T.);
#6667=EDGE_CURVE('',#5286,#5371,#3327,.T.);
#6668=EDGE_CURVE('',#5372,#5371,#4648,.T.);
#6669=EDGE_CURVE('',#5372,#5287,#3328,.T.);
#6670=EDGE_CURVE('',#5373,#5372,#201,.T.);
#6671=EDGE_CURVE('',#5288,#5373,#3329,.T.);
#6672=EDGE_CURVE('',#5374,#5373,#3330,.T.);
#6673=EDGE_CURVE('',#5289,#5374,#3331,.T.);
#6674=EDGE_CURVE('',#5375,#5374,#202,.T.);
#6675=EDGE_CURVE('',#5290,#5375,#3332,.T.);
#6676=EDGE_CURVE('',#5376,#5375,#4649,.T.);
#6677=EDGE_CURVE('',#5376,#5291,#3333,.T.);
#6678=EDGE_CURVE('',#5377,#5376,#203,.T.);
#6679=EDGE_CURVE('',#5292,#5377,#3334,.T.);
#6680=EDGE_CURVE('',#5378,#5377,#3335,.T.);
#6681=EDGE_CURVE('',#5293,#5378,#3336,.T.);
#6682=EDGE_CURVE('',#5379,#5378,#204,.T.);
#6683=EDGE_CURVE('',#5294,#5379,#3337,.T.);
#6684=EDGE_CURVE('',#5380,#5379,#4650,.T.);
#6685=EDGE_CURVE('',#5380,#5295,#3338,.T.);
#6686=EDGE_CURVE('',#5381,#5380,#205,.T.);
#6687=EDGE_CURVE('',#5296,#5381,#3339,.T.);
#6688=EDGE_CURVE('',#5382,#5381,#3340,.T.);
#6689=EDGE_CURVE('',#5297,#5382,#3341,.T.);
#6690=EDGE_CURVE('',#5383,#5382,#206,.T.);
#6691=EDGE_CURVE('',#5298,#5383,#3342,.T.);
#6692=EDGE_CURVE('',#5384,#5383,#4651,.T.);
#6693=EDGE_CURVE('',#5384,#5299,#3343,.T.);
#6694=EDGE_CURVE('',#5385,#5384,#207,.T.);
#6695=EDGE_CURVE('',#5300,#5385,#3344,.T.);
#6696=EDGE_CURVE('',#5386,#5385,#3345,.T.);
#6697=EDGE_CURVE('',#5301,#5386,#3346,.T.);
#6698=EDGE_CURVE('',#5387,#5386,#208,.T.);
#6699=EDGE_CURVE('',#5302,#5387,#3347,.T.);
#6700=EDGE_CURVE('',#5388,#5387,#4652,.T.);
#6701=EDGE_CURVE('',#5388,#5303,#3348,.T.);
#6702=EDGE_CURVE('',#5389,#5388,#209,.T.);
#6703=EDGE_CURVE('',#5304,#5389,#3349,.T.);
#6704=EDGE_CURVE('',#5390,#5389,#3350,.T.);
#6705=EDGE_CURVE('',#5305,#5390,#3351,.T.);
#6706=EDGE_CURVE('',#5391,#5390,#210,.T.);
#6707=EDGE_CURVE('',#5306,#5391,#3352,.T.);
#6708=EDGE_CURVE('',#5312,#5391,#4653,.T.);
#6709=EDGE_CURVE('',#5392,#5393,#3353,.T.);
#6710=EDGE_CURVE('',#5393,#5394,#3354,.T.);
#6711=EDGE_CURVE('',#5394,#5395,#3355,.T.);
#6712=EDGE_CURVE('',#5395,#5392,#3356,.T.);
#6713=EDGE_CURVE('',#5396,#5397,#3357,.T.);
#6714=EDGE_CURVE('',#5397,#5393,#4654,.T.);
#6715=EDGE_CURVE('',#5392,#5396,#4655,.T.);
#6716=EDGE_CURVE('',#5398,#5399,#3358,.T.);
#6717=EDGE_CURVE('',#5399,#5397,#3359,.T.);
#6718=EDGE_CURVE('',#5396,#5398,#3360,.T.);
#6719=EDGE_CURVE('',#5394,#5399,#4656,.T.);
#6720=EDGE_CURVE('',#5398,#5395,#4657,.T.);
#6721=EDGE_CURVE('',#5400,#5392,#3361,.T.);
#6722=EDGE_CURVE('',#5401,#5400,#4658,.T.);
#6723=EDGE_CURVE('',#5401,#5396,#3362,.T.);
#6724=EDGE_CURVE('',#5402,#5395,#3363,.T.);
#6725=EDGE_CURVE('',#5400,#5402,#3364,.T.);
#6726=EDGE_CURVE('',#5403,#5400,#3365,.T.);
#6727=EDGE_CURVE('',#5402,#5404,#3366,.T.);
#6728=EDGE_CURVE('',#5404,#5403,#3367,.T.);
#6729=EDGE_CURVE('',#5405,#5401,#3368,.T.);
#6730=EDGE_CURVE('',#5403,#5405,#4659,.T.);
#6731=EDGE_CURVE('',#5406,#5407,#3369,.T.);
#6732=EDGE_CURVE('',#5407,#5401,#3370,.T.);
#6733=EDGE_CURVE('',#5405,#5406,#3371,.T.);
#6734=EDGE_CURVE('',#5402,#5407,#4660,.T.);
#6735=EDGE_CURVE('',#5406,#5404,#4661,.T.);
#6736=EDGE_CURVE('',#5407,#5398,#3372,.T.);
#6737=EDGE_CURVE('',#5408,#5409,#3373,.T.);
#6738=EDGE_CURVE('',#5408,#5410,#3374,.T.);
#6739=EDGE_CURVE('',#5411,#5410,#3375,.T.);
#6740=EDGE_CURVE('',#5411,#5409,#3376,.T.);
#6741=EDGE_CURVE('',#5409,#5412,#4662,.T.);
#6742=EDGE_CURVE('',#5413,#5411,#3377,.T.);
#6743=EDGE_CURVE('',#5412,#5413,#3378,.T.);
#6744=EDGE_CURVE('',#5412,#5414,#3379,.T.);
#6745=EDGE_CURVE('',#5413,#5415,#3380,.T.);
#6746=EDGE_CURVE('',#5415,#5414,#3381,.T.);
#6747=EDGE_CURVE('',#5410,#5415,#3382,.T.);
#6748=EDGE_CURVE('',#5414,#5408,#4663,.T.);
#6749=EDGE_CURVE('',#5416,#5416,#4664,.T.);
#6750=EDGE_CURVE('',#5416,#5417,#3383,.T.);
#6751=EDGE_CURVE('',#5417,#5417,#4665,.T.);
#6752=EDGE_CURVE('',#5418,#5418,#4666,.T.);
#6753=EDGE_CURVE('',#5418,#5419,#3384,.T.);
#6754=EDGE_CURVE('',#5419,#5419,#4667,.T.);
#6755=EDGE_CURVE('',#5420,#5420,#4668,.T.);
#6756=EDGE_CURVE('',#5420,#5421,#3385,.T.);
#6757=EDGE_CURVE('',#5421,#5421,#4669,.T.);
#6758=EDGE_CURVE('',#5422,#5422,#4670,.T.);
#6759=EDGE_CURVE('',#5422,#5423,#3386,.T.);
#6760=EDGE_CURVE('',#5423,#5423,#4671,.T.);
#6761=EDGE_CURVE('',#5424,#5424,#4672,.T.);
#6762=EDGE_CURVE('',#5424,#5425,#3387,.T.);
#6763=EDGE_CURVE('',#5425,#5425,#4673,.T.);
#6764=EDGE_CURVE('',#5426,#5427,#3388,.T.);
#6765=EDGE_CURVE('',#5426,#5427,#4674,.T.);
#6766=EDGE_CURVE('',#5428,#5426,#707,.T.);
#6767=EDGE_CURVE('',#5429,#5428,#4675,.T.);
#6768=EDGE_CURVE('',#5429,#5430,#3389,.T.);
#6769=EDGE_CURVE('',#5431,#5430,#708,.T.);
#6770=EDGE_CURVE('',#5430,#5431,#709,.T.);
#6771=EDGE_CURVE('',#5432,#5429,#4676,.T.);
#6772=EDGE_CURVE('',#5427,#5432,#710,.T.);
#6773=EDGE_CURVE('',#5432,#5428,#3390,.T.);
#6774=EDGE_CURVE('',#5433,#5433,#4677,.T.);
#6775=EDGE_CURVE('',#5433,#5434,#3391,.T.);
#6776=EDGE_CURVE('',#5434,#5434,#4678,.T.);
#6777=EDGE_CURVE('',#5435,#5435,#4679,.T.);
#6778=EDGE_CURVE('',#5435,#5436,#3392,.T.);
#6779=EDGE_CURVE('',#5436,#5436,#4680,.T.);
#6780=EDGE_CURVE('',#5437,#5437,#4681,.T.);
#6781=EDGE_CURVE('',#5437,#5438,#3393,.T.);
#6782=EDGE_CURVE('',#5438,#5438,#4682,.T.);
#6783=EDGE_CURVE('',#5439,#5439,#4683,.T.);
#6784=EDGE_CURVE('',#5439,#5440,#3394,.T.);
#6785=EDGE_CURVE('',#5440,#5440,#4684,.T.);
#6786=EDGE_CURVE('',#5441,#5442,#3395,.T.);
#6787=EDGE_CURVE('',#5441,#5442,#4685,.T.);
#6788=EDGE_CURVE('',#5443,#5441,#711,.T.);
#6789=EDGE_CURVE('',#5444,#5443,#4686,.T.);
#6790=EDGE_CURVE('',#5444,#5445,#3396,.T.);
#6791=EDGE_CURVE('',#5446,#5445,#712,.T.);
#6792=EDGE_CURVE('',#5445,#5446,#713,.T.);
#6793=EDGE_CURVE('',#5447,#5444,#4687,.T.);
#6794=EDGE_CURVE('',#5442,#5447,#714,.T.);
#6795=EDGE_CURVE('',#5447,#5443,#3397,.T.);
#6796=EDGE_CURVE('',#5448,#5448,#4688,.T.);
#6797=EDGE_CURVE('',#5448,#5449,#3398,.T.);
#6798=EDGE_CURVE('',#5449,#5449,#4689,.T.);
#6799=EDGE_CURVE('',#5450,#5450,#4690,.T.);
#6800=EDGE_CURVE('',#5450,#5451,#3399,.T.);
#6801=EDGE_CURVE('',#5451,#5451,#4691,.T.);
#6802=EDGE_CURVE('',#5452,#5452,#4692,.T.);
#6803=EDGE_CURVE('',#5452,#5453,#3400,.T.);
#6804=EDGE_CURVE('',#5453,#5453,#4693,.T.);
#6805=EDGE_CURVE('',#5454,#5454,#4694,.T.);
#6806=EDGE_CURVE('',#5454,#5455,#3401,.T.);
#6807=EDGE_CURVE('',#5455,#5455,#4695,.T.);
#6808=EDGE_CURVE('',#5456,#5457,#3402,.T.);
#6809=EDGE_CURVE('',#5458,#5456,#3403,.T.);
#6810=EDGE_CURVE('',#5459,#5458,#3404,.T.);
#6811=EDGE_CURVE('',#5457,#5459,#3405,.T.);
#6812=EDGE_CURVE('',#5460,#5456,#3406,.T.);
#6813=EDGE_CURVE('',#5460,#5461,#3407,.T.);
#6814=EDGE_CURVE('',#5458,#5461,#3408,.T.);
#6815=EDGE_CURVE('',#5462,#5460,#3409,.T.);
#6816=EDGE_CURVE('',#5463,#5462,#3410,.T.);
#6817=EDGE_CURVE('',#5461,#5463,#3411,.T.);
#6818=EDGE_CURVE('',#5464,#5465,#4696,.T.);
#6819=EDGE_CURVE('',#5465,#5466,#211,.T.);
#6820=EDGE_CURVE('',#5466,#5467,#3412,.T.);
#6821=EDGE_CURVE('',#5467,#5468,#212,.T.);
#6822=EDGE_CURVE('',#5468,#5469,#4697,.T.);
#6823=EDGE_CURVE('',#5469,#5470,#213,.T.);
#6824=EDGE_CURVE('',#5470,#5471,#3413,.T.);
#6825=EDGE_CURVE('',#5471,#5472,#214,.T.);
#6826=EDGE_CURVE('',#5472,#5473,#4698,.T.);
#6827=EDGE_CURVE('',#5473,#5474,#215,.T.);
#6828=EDGE_CURVE('',#5474,#5475,#3414,.T.);
#6829=EDGE_CURVE('',#5475,#5476,#216,.T.);
#6830=EDGE_CURVE('',#5476,#5477,#4699,.T.);
#6831=EDGE_CURVE('',#5477,#5478,#217,.T.);
#6832=EDGE_CURVE('',#5478,#5479,#3415,.T.);
#6833=EDGE_CURVE('',#5479,#5480,#218,.T.);
#6834=EDGE_CURVE('',#5480,#5481,#4700,.T.);
#6835=EDGE_CURVE('',#5481,#5482,#219,.T.);
#6836=EDGE_CURVE('',#5482,#5483,#3416,.T.);
#6837=EDGE_CURVE('',#5483,#5484,#220,.T.);
#6838=EDGE_CURVE('',#5484,#5485,#4701,.T.);
#6839=EDGE_CURVE('',#5485,#5486,#221,.T.);
#6840=EDGE_CURVE('',#5486,#5487,#3417,.T.);
#6841=EDGE_CURVE('',#5487,#5488,#222,.T.);
#6842=EDGE_CURVE('',#5488,#5489,#4702,.T.);
#6843=EDGE_CURVE('',#5489,#5490,#223,.T.);
#6844=EDGE_CURVE('',#5490,#5491,#3418,.T.);
#6845=EDGE_CURVE('',#5491,#5492,#224,.T.);
#6846=EDGE_CURVE('',#5492,#5493,#4703,.T.);
#6847=EDGE_CURVE('',#5493,#5494,#225,.T.);
#6848=EDGE_CURVE('',#5494,#5495,#3419,.T.);
#6849=EDGE_CURVE('',#5495,#5496,#226,.T.);
#6850=EDGE_CURVE('',#5496,#5497,#4704,.T.);
#6851=EDGE_CURVE('',#5497,#5498,#227,.T.);
#6852=EDGE_CURVE('',#5498,#5499,#3420,.T.);
#6853=EDGE_CURVE('',#5499,#5500,#228,.T.);
#6854=EDGE_CURVE('',#5500,#5501,#4705,.T.);
#6855=EDGE_CURVE('',#5501,#5502,#229,.T.);
#6856=EDGE_CURVE('',#5502,#5503,#3421,.T.);
#6857=EDGE_CURVE('',#5503,#5504,#230,.T.);
#6858=EDGE_CURVE('',#5504,#5505,#4706,.T.);
#6859=EDGE_CURVE('',#5505,#5506,#231,.T.);
#6860=EDGE_CURVE('',#5506,#5507,#3422,.T.);
#6861=EDGE_CURVE('',#5507,#5508,#232,.T.);
#6862=EDGE_CURVE('',#5508,#5509,#4707,.T.);
#6863=EDGE_CURVE('',#5509,#5510,#233,.T.);
#6864=EDGE_CURVE('',#5510,#5511,#3423,.T.);
#6865=EDGE_CURVE('',#5511,#5512,#234,.T.);
#6866=EDGE_CURVE('',#5512,#5513,#4708,.T.);
#6867=EDGE_CURVE('',#5513,#5514,#235,.T.);
#6868=EDGE_CURVE('',#5514,#5515,#3424,.T.);
#6869=EDGE_CURVE('',#5515,#5516,#236,.T.);
#6870=EDGE_CURVE('',#5516,#5517,#4709,.T.);
#6871=EDGE_CURVE('',#5517,#5518,#237,.T.);
#6872=EDGE_CURVE('',#5518,#5519,#3425,.T.);
#6873=EDGE_CURVE('',#5519,#5520,#238,.T.);
#6874=EDGE_CURVE('',#5520,#5521,#4710,.T.);
#6875=EDGE_CURVE('',#5521,#5522,#239,.T.);
#6876=EDGE_CURVE('',#5522,#5523,#3426,.T.);
#6877=EDGE_CURVE('',#5523,#5524,#240,.T.);
#6878=EDGE_CURVE('',#5524,#5525,#4711,.T.);
#6879=EDGE_CURVE('',#5525,#5526,#241,.T.);
#6880=EDGE_CURVE('',#5526,#5527,#3427,.T.);
#6881=EDGE_CURVE('',#5527,#5528,#242,.T.);
#6882=EDGE_CURVE('',#5528,#5529,#4712,.T.);
#6883=EDGE_CURVE('',#5529,#5530,#243,.T.);
#6884=EDGE_CURVE('',#5530,#5531,#3428,.T.);
#6885=EDGE_CURVE('',#5531,#5532,#244,.T.);
#6886=EDGE_CURVE('',#5532,#5533,#4713,.T.);
#6887=EDGE_CURVE('',#5533,#5534,#245,.T.);
#6888=EDGE_CURVE('',#5534,#5535,#3429,.T.);
#6889=EDGE_CURVE('',#5535,#5536,#246,.T.);
#6890=EDGE_CURVE('',#5536,#5537,#4714,.T.);
#6891=EDGE_CURVE('',#5537,#5538,#247,.T.);
#6892=EDGE_CURVE('',#5538,#5539,#3430,.T.);
#6893=EDGE_CURVE('',#5539,#5540,#248,.T.);
#6894=EDGE_CURVE('',#5540,#5541,#4715,.T.);
#6895=EDGE_CURVE('',#5541,#5542,#249,.T.);
#6896=EDGE_CURVE('',#5542,#5543,#3431,.T.);
#6897=EDGE_CURVE('',#5543,#5544,#250,.T.);
#6898=EDGE_CURVE('',#5544,#5545,#4716,.T.);
#6899=EDGE_CURVE('',#5545,#5546,#251,.T.);
#6900=EDGE_CURVE('',#5546,#5547,#3432,.T.);
#6901=EDGE_CURVE('',#5547,#5548,#252,.T.);
#6902=EDGE_CURVE('',#5548,#5549,#4717,.T.);
#6903=EDGE_CURVE('',#5549,#5550,#253,.T.);
#6904=EDGE_CURVE('',#5550,#5551,#3433,.T.);
#6905=EDGE_CURVE('',#5551,#5552,#254,.T.);
#6906=EDGE_CURVE('',#5552,#5553,#4718,.T.);
#6907=EDGE_CURVE('',#5553,#5554,#255,.T.);
#6908=EDGE_CURVE('',#5554,#5555,#3434,.T.);
#6909=EDGE_CURVE('',#5555,#5556,#256,.T.);
#6910=EDGE_CURVE('',#5556,#5557,#4719,.T.);
#6911=EDGE_CURVE('',#5557,#5558,#257,.T.);
#6912=EDGE_CURVE('',#5558,#5559,#3435,.T.);
#6913=EDGE_CURVE('',#5559,#5560,#258,.T.);
#6914=EDGE_CURVE('',#5560,#5561,#4720,.T.);
#6915=EDGE_CURVE('',#5561,#5562,#259,.T.);
#6916=EDGE_CURVE('',#5562,#5563,#3436,.T.);
#6917=EDGE_CURVE('',#5563,#5564,#260,.T.);
#6918=EDGE_CURVE('',#5564,#5565,#4721,.T.);
#6919=EDGE_CURVE('',#5565,#5566,#261,.T.);
#6920=EDGE_CURVE('',#5566,#5567,#3437,.T.);
#6921=EDGE_CURVE('',#5567,#5568,#262,.T.);
#6922=EDGE_CURVE('',#5568,#5569,#4722,.T.);
#6923=EDGE_CURVE('',#5569,#5570,#263,.T.);
#6924=EDGE_CURVE('',#5570,#5571,#3438,.T.);
#6925=EDGE_CURVE('',#5571,#5572,#264,.T.);
#6926=EDGE_CURVE('',#5572,#5573,#4723,.T.);
#6927=EDGE_CURVE('',#5573,#5574,#265,.T.);
#6928=EDGE_CURVE('',#5574,#5575,#3439,.T.);
#6929=EDGE_CURVE('',#5575,#5576,#266,.T.);
#6930=EDGE_CURVE('',#5576,#5577,#4724,.T.);
#6931=EDGE_CURVE('',#5577,#5578,#267,.T.);
#6932=EDGE_CURVE('',#5578,#5579,#3440,.T.);
#6933=EDGE_CURVE('',#5579,#5580,#268,.T.);
#6934=EDGE_CURVE('',#5580,#5581,#4725,.T.);
#6935=EDGE_CURVE('',#5581,#5582,#269,.T.);
#6936=EDGE_CURVE('',#5582,#5583,#3441,.T.);
#6937=EDGE_CURVE('',#5583,#5584,#270,.T.);
#6938=EDGE_CURVE('',#5584,#5585,#4726,.T.);
#6939=EDGE_CURVE('',#5585,#5586,#271,.T.);
#6940=EDGE_CURVE('',#5586,#5587,#3442,.T.);
#6941=EDGE_CURVE('',#5587,#5588,#272,.T.);
#6942=EDGE_CURVE('',#5588,#5589,#4727,.T.);
#6943=EDGE_CURVE('',#5589,#5590,#273,.T.);
#6944=EDGE_CURVE('',#5590,#5591,#3443,.T.);
#6945=EDGE_CURVE('',#5591,#5592,#274,.T.);
#6946=EDGE_CURVE('',#5592,#5593,#4728,.T.);
#6947=EDGE_CURVE('',#5593,#5594,#275,.T.);
#6948=EDGE_CURVE('',#5594,#5595,#3444,.T.);
#6949=EDGE_CURVE('',#5595,#5596,#276,.T.);
#6950=EDGE_CURVE('',#5596,#5597,#4729,.T.);
#6951=EDGE_CURVE('',#5597,#5598,#277,.T.);
#6952=EDGE_CURVE('',#5598,#5599,#3445,.T.);
#6953=EDGE_CURVE('',#5599,#5600,#278,.T.);
#6954=EDGE_CURVE('',#5600,#5601,#4730,.T.);
#6955=EDGE_CURVE('',#5601,#5602,#279,.T.);
#6956=EDGE_CURVE('',#5602,#5603,#3446,.T.);
#6957=EDGE_CURVE('',#5603,#5604,#280,.T.);
#6958=EDGE_CURVE('',#5604,#5605,#4731,.T.);
#6959=EDGE_CURVE('',#5605,#5606,#281,.T.);
#6960=EDGE_CURVE('',#5606,#5607,#3447,.T.);
#6961=EDGE_CURVE('',#5607,#5608,#282,.T.);
#6962=EDGE_CURVE('',#5608,#5609,#4732,.T.);
#6963=EDGE_CURVE('',#5609,#5610,#283,.T.);
#6964=EDGE_CURVE('',#5610,#5611,#3448,.T.);
#6965=EDGE_CURVE('',#5611,#5612,#284,.T.);
#6966=EDGE_CURVE('',#5612,#5613,#4733,.T.);
#6967=EDGE_CURVE('',#5613,#5614,#285,.T.);
#6968=EDGE_CURVE('',#5614,#5615,#3449,.T.);
#6969=EDGE_CURVE('',#5615,#5616,#286,.T.);
#6970=EDGE_CURVE('',#5616,#5617,#4734,.T.);
#6971=EDGE_CURVE('',#5617,#5618,#287,.T.);
#6972=EDGE_CURVE('',#5618,#5619,#3450,.T.);
#6973=EDGE_CURVE('',#5619,#5620,#288,.T.);
#6974=EDGE_CURVE('',#5620,#5621,#4735,.T.);
#6975=EDGE_CURVE('',#5621,#5622,#289,.T.);
#6976=EDGE_CURVE('',#5622,#5623,#3451,.T.);
#6977=EDGE_CURVE('',#5623,#5464,#290,.T.);
#6978=EDGE_CURVE('',#5463,#5459,#4736,.T.);
#6979=EDGE_CURVE('',#5457,#5462,#4737,.T.);
#6980=EDGE_CURVE('',#5624,#5624,#4738,.T.);
#6981=EDGE_CURVE('',#5624,#5625,#3452,.T.);
#6982=EDGE_CURVE('',#5625,#5625,#4739,.T.);
#6983=EDGE_CURVE('',#5626,#5621,#715,.T.);
#6984=EDGE_CURVE('',#5627,#5626,#291,.T.);
#6985=EDGE_CURVE('',#5622,#5627,#3453,.T.);
#6986=EDGE_CURVE('',#5464,#5628,#716,.T.);
#6987=EDGE_CURVE('',#5623,#5629,#3454,.T.);
#6988=EDGE_CURVE('',#5628,#5629,#292,.T.);
#6989=EDGE_CURVE('',#5629,#5627,#3455,.T.);
#6990=EDGE_CURVE('',#5630,#5628,#4740,.T.);
#6991=EDGE_CURVE('',#5630,#5465,#717,.T.);
#6992=EDGE_CURVE('',#5631,#5630,#293,.T.);
#6993=EDGE_CURVE('',#5466,#5631,#3456,.T.);
#6994=EDGE_CURVE('',#5468,#5632,#718,.T.);
#6995=EDGE_CURVE('',#5467,#5633,#3457,.T.);
#6996=EDGE_CURVE('',#5632,#5633,#294,.T.);
#6997=EDGE_CURVE('',#5633,#5631,#3458,.T.);
#6998=EDGE_CURVE('',#5634,#5632,#4741,.T.);
#6999=EDGE_CURVE('',#5634,#5469,#719,.T.);
#7000=EDGE_CURVE('',#5635,#5634,#295,.T.);
#7001=EDGE_CURVE('',#5470,#5635,#3459,.T.);
#7002=EDGE_CURVE('',#5472,#5636,#720,.T.);
#7003=EDGE_CURVE('',#5471,#5637,#3460,.T.);
#7004=EDGE_CURVE('',#5636,#5637,#296,.T.);
#7005=EDGE_CURVE('',#5637,#5635,#3461,.T.);
#7006=EDGE_CURVE('',#5638,#5636,#4742,.T.);
#7007=EDGE_CURVE('',#5638,#5473,#721,.T.);
#7008=EDGE_CURVE('',#5639,#5638,#297,.T.);
#7009=EDGE_CURVE('',#5474,#5639,#3462,.T.);
#7010=EDGE_CURVE('',#5476,#5640,#722,.T.);
#7011=EDGE_CURVE('',#5475,#5641,#3463,.T.);
#7012=EDGE_CURVE('',#5640,#5641,#298,.T.);
#7013=EDGE_CURVE('',#5641,#5639,#3464,.T.);
#7014=EDGE_CURVE('',#5642,#5640,#4743,.T.);
#7015=EDGE_CURVE('',#5642,#5477,#723,.T.);
#7016=EDGE_CURVE('',#5643,#5642,#299,.T.);
#7017=EDGE_CURVE('',#5478,#5643,#3465,.T.);
#7018=EDGE_CURVE('',#5480,#5644,#724,.T.);
#7019=EDGE_CURVE('',#5479,#5645,#3466,.T.);
#7020=EDGE_CURVE('',#5644,#5645,#300,.T.);
#7021=EDGE_CURVE('',#5645,#5643,#3467,.T.);
#7022=EDGE_CURVE('',#5646,#5644,#4744,.T.);
#7023=EDGE_CURVE('',#5646,#5481,#725,.T.);
#7024=EDGE_CURVE('',#5647,#5646,#301,.T.);
#7025=EDGE_CURVE('',#5482,#5647,#3468,.T.);
#7026=EDGE_CURVE('',#5484,#5648,#726,.T.);
#7027=EDGE_CURVE('',#5483,#5649,#3469,.T.);
#7028=EDGE_CURVE('',#5648,#5649,#302,.T.);
#7029=EDGE_CURVE('',#5649,#5647,#3470,.T.);
#7030=EDGE_CURVE('',#5650,#5648,#4745,.T.);
#7031=EDGE_CURVE('',#5650,#5485,#727,.T.);
#7032=EDGE_CURVE('',#5651,#5650,#303,.T.);
#7033=EDGE_CURVE('',#5486,#5651,#3471,.T.);
#7034=EDGE_CURVE('',#5488,#5652,#728,.T.);
#7035=EDGE_CURVE('',#5487,#5653,#3472,.T.);
#7036=EDGE_CURVE('',#5652,#5653,#304,.T.);
#7037=EDGE_CURVE('',#5653,#5651,#3473,.T.);
#7038=EDGE_CURVE('',#5654,#5652,#4746,.T.);
#7039=EDGE_CURVE('',#5654,#5489,#729,.T.);
#7040=EDGE_CURVE('',#5655,#5654,#305,.T.);
#7041=EDGE_CURVE('',#5490,#5655,#3474,.T.);
#7042=EDGE_CURVE('',#5492,#5656,#730,.T.);
#7043=EDGE_CURVE('',#5491,#5657,#3475,.T.);
#7044=EDGE_CURVE('',#5656,#5657,#306,.T.);
#7045=EDGE_CURVE('',#5657,#5655,#3476,.T.);
#7046=EDGE_CURVE('',#5658,#5656,#4747,.T.);
#7047=EDGE_CURVE('',#5658,#5493,#731,.T.);
#7048=EDGE_CURVE('',#5659,#5658,#307,.T.);
#7049=EDGE_CURVE('',#5494,#5659,#3477,.T.);
#7050=EDGE_CURVE('',#5496,#5660,#732,.T.);
#7051=EDGE_CURVE('',#5495,#5661,#3478,.T.);
#7052=EDGE_CURVE('',#5660,#5661,#308,.T.);
#7053=EDGE_CURVE('',#5661,#5659,#3479,.T.);
#7054=EDGE_CURVE('',#5662,#5660,#4748,.T.);
#7055=EDGE_CURVE('',#5662,#5497,#733,.T.);
#7056=EDGE_CURVE('',#5663,#5662,#309,.T.);
#7057=EDGE_CURVE('',#5498,#5663,#3480,.T.);
#7058=EDGE_CURVE('',#5500,#5664,#734,.T.);
#7059=EDGE_CURVE('',#5499,#5665,#3481,.T.);
#7060=EDGE_CURVE('',#5664,#5665,#310,.T.);
#7061=EDGE_CURVE('',#5665,#5663,#3482,.T.);
#7062=EDGE_CURVE('',#5666,#5664,#4749,.T.);
#7063=EDGE_CURVE('',#5666,#5501,#735,.T.);
#7064=EDGE_CURVE('',#5667,#5666,#311,.T.);
#7065=EDGE_CURVE('',#5502,#5667,#3483,.T.);
#7066=EDGE_CURVE('',#5504,#5668,#736,.T.);
#7067=EDGE_CURVE('',#5503,#5669,#3484,.T.);
#7068=EDGE_CURVE('',#5668,#5669,#312,.T.);
#7069=EDGE_CURVE('',#5669,#5667,#3485,.T.);
#7070=EDGE_CURVE('',#5670,#5668,#4750,.T.);
#7071=EDGE_CURVE('',#5670,#5505,#737,.T.);
#7072=EDGE_CURVE('',#5671,#5670,#313,.T.);
#7073=EDGE_CURVE('',#5506,#5671,#3486,.T.);
#7074=EDGE_CURVE('',#5508,#5672,#738,.T.);
#7075=EDGE_CURVE('',#5507,#5673,#3487,.T.);
#7076=EDGE_CURVE('',#5672,#5673,#314,.T.);
#7077=EDGE_CURVE('',#5673,#5671,#3488,.T.);
#7078=EDGE_CURVE('',#5674,#5672,#4751,.T.);
#7079=EDGE_CURVE('',#5674,#5509,#739,.T.);
#7080=EDGE_CURVE('',#5675,#5674,#315,.T.);
#7081=EDGE_CURVE('',#5510,#5675,#3489,.T.);
#7082=EDGE_CURVE('',#5512,#5676,#740,.T.);
#7083=EDGE_CURVE('',#5511,#5677,#3490,.T.);
#7084=EDGE_CURVE('',#5676,#5677,#316,.T.);
#7085=EDGE_CURVE('',#5677,#5675,#3491,.T.);
#7086=EDGE_CURVE('',#5678,#5676,#4752,.T.);
#7087=EDGE_CURVE('',#5678,#5513,#741,.T.);
#7088=EDGE_CURVE('',#5679,#5678,#317,.T.);
#7089=EDGE_CURVE('',#5514,#5679,#3492,.T.);
#7090=EDGE_CURVE('',#5516,#5680,#742,.T.);
#7091=EDGE_CURVE('',#5515,#5681,#3493,.T.);
#7092=EDGE_CURVE('',#5680,#5681,#318,.T.);
#7093=EDGE_CURVE('',#5681,#5679,#3494,.T.);
#7094=EDGE_CURVE('',#5682,#5680,#4753,.T.);
#7095=EDGE_CURVE('',#5682,#5517,#743,.T.);
#7096=EDGE_CURVE('',#5683,#5682,#319,.T.);
#7097=EDGE_CURVE('',#5518,#5683,#3495,.T.);
#7098=EDGE_CURVE('',#5520,#5684,#744,.T.);
#7099=EDGE_CURVE('',#5519,#5685,#3496,.T.);
#7100=EDGE_CURVE('',#5684,#5685,#320,.T.);
#7101=EDGE_CURVE('',#5685,#5683,#3497,.T.);
#7102=EDGE_CURVE('',#5686,#5684,#4754,.T.);
#7103=EDGE_CURVE('',#5686,#5521,#745,.T.);
#7104=EDGE_CURVE('',#5687,#5686,#321,.T.);
#7105=EDGE_CURVE('',#5522,#5687,#3498,.T.);
#7106=EDGE_CURVE('',#5524,#5688,#746,.T.);
#7107=EDGE_CURVE('',#5523,#5689,#3499,.T.);
#7108=EDGE_CURVE('',#5688,#5689,#322,.T.);
#7109=EDGE_CURVE('',#5689,#5687,#3500,.T.);
#7110=EDGE_CURVE('',#5690,#5688,#4755,.T.);
#7111=EDGE_CURVE('',#5690,#5525,#747,.T.);
#7112=EDGE_CURVE('',#5691,#5690,#323,.T.);
#7113=EDGE_CURVE('',#5526,#5691,#3501,.T.);
#7114=EDGE_CURVE('',#5528,#5692,#748,.T.);
#7115=EDGE_CURVE('',#5527,#5693,#3502,.T.);
#7116=EDGE_CURVE('',#5692,#5693,#324,.T.);
#7117=EDGE_CURVE('',#5693,#5691,#3503,.T.);
#7118=EDGE_CURVE('',#5694,#5692,#4756,.T.);
#7119=EDGE_CURVE('',#5694,#5529,#749,.T.);
#7120=EDGE_CURVE('',#5695,#5694,#325,.T.);
#7121=EDGE_CURVE('',#5530,#5695,#3504,.T.);
#7122=EDGE_CURVE('',#5532,#5696,#750,.T.);
#7123=EDGE_CURVE('',#5531,#5697,#3505,.T.);
#7124=EDGE_CURVE('',#5696,#5697,#326,.T.);
#7125=EDGE_CURVE('',#5697,#5695,#3506,.T.);
#7126=EDGE_CURVE('',#5698,#5696,#4757,.T.);
#7127=EDGE_CURVE('',#5698,#5533,#751,.T.);
#7128=EDGE_CURVE('',#5699,#5698,#327,.T.);
#7129=EDGE_CURVE('',#5534,#5699,#3507,.T.);
#7130=EDGE_CURVE('',#5536,#5700,#752,.T.);
#7131=EDGE_CURVE('',#5535,#5701,#3508,.T.);
#7132=EDGE_CURVE('',#5700,#5701,#328,.T.);
#7133=EDGE_CURVE('',#5701,#5699,#3509,.T.);
#7134=EDGE_CURVE('',#5702,#5700,#4758,.T.);
#7135=EDGE_CURVE('',#5702,#5537,#753,.T.);
#7136=EDGE_CURVE('',#5703,#5702,#329,.T.);
#7137=EDGE_CURVE('',#5538,#5703,#3510,.T.);
#7138=EDGE_CURVE('',#5540,#5704,#754,.T.);
#7139=EDGE_CURVE('',#5539,#5705,#3511,.T.);
#7140=EDGE_CURVE('',#5704,#5705,#330,.T.);
#7141=EDGE_CURVE('',#5705,#5703,#3512,.T.);
#7142=EDGE_CURVE('',#5706,#5704,#4759,.T.);
#7143=EDGE_CURVE('',#5706,#5541,#755,.T.);
#7144=EDGE_CURVE('',#5707,#5706,#331,.T.);
#7145=EDGE_CURVE('',#5542,#5707,#3513,.T.);
#7146=EDGE_CURVE('',#5544,#5708,#756,.T.);
#7147=EDGE_CURVE('',#5543,#5709,#3514,.T.);
#7148=EDGE_CURVE('',#5708,#5709,#332,.T.);
#7149=EDGE_CURVE('',#5709,#5707,#3515,.T.);
#7150=EDGE_CURVE('',#5710,#5708,#4760,.T.);
#7151=EDGE_CURVE('',#5710,#5545,#757,.T.);
#7152=EDGE_CURVE('',#5711,#5710,#333,.T.);
#7153=EDGE_CURVE('',#5546,#5711,#3516,.T.);
#7154=EDGE_CURVE('',#5548,#5712,#758,.T.);
#7155=EDGE_CURVE('',#5547,#5713,#3517,.T.);
#7156=EDGE_CURVE('',#5712,#5713,#334,.T.);
#7157=EDGE_CURVE('',#5713,#5711,#3518,.T.);
#7158=EDGE_CURVE('',#5714,#5712,#4761,.T.);
#7159=EDGE_CURVE('',#5714,#5549,#759,.T.);
#7160=EDGE_CURVE('',#5715,#5714,#335,.T.);
#7161=EDGE_CURVE('',#5550,#5715,#3519,.T.);
#7162=EDGE_CURVE('',#5552,#5716,#760,.T.);
#7163=EDGE_CURVE('',#5551,#5717,#3520,.T.);
#7164=EDGE_CURVE('',#5716,#5717,#336,.T.);
#7165=EDGE_CURVE('',#5717,#5715,#3521,.T.);
#7166=EDGE_CURVE('',#5718,#5716,#4762,.T.);
#7167=EDGE_CURVE('',#5718,#5553,#761,.T.);
#7168=EDGE_CURVE('',#5719,#5718,#337,.T.);
#7169=EDGE_CURVE('',#5554,#5719,#3522,.T.);
#7170=EDGE_CURVE('',#5556,#5720,#762,.T.);
#7171=EDGE_CURVE('',#5555,#5721,#3523,.T.);
#7172=EDGE_CURVE('',#5720,#5721,#338,.T.);
#7173=EDGE_CURVE('',#5721,#5719,#3524,.T.);
#7174=EDGE_CURVE('',#5722,#5720,#4763,.T.);
#7175=EDGE_CURVE('',#5722,#5557,#763,.T.);
#7176=EDGE_CURVE('',#5723,#5722,#339,.T.);
#7177=EDGE_CURVE('',#5558,#5723,#3525,.T.);
#7178=EDGE_CURVE('',#5560,#5724,#764,.T.);
#7179=EDGE_CURVE('',#5559,#5725,#3526,.T.);
#7180=EDGE_CURVE('',#5724,#5725,#340,.T.);
#7181=EDGE_CURVE('',#5725,#5723,#3527,.T.);
#7182=EDGE_CURVE('',#5726,#5724,#4764,.T.);
#7183=EDGE_CURVE('',#5726,#5561,#765,.T.);
#7184=EDGE_CURVE('',#5727,#5726,#341,.T.);
#7185=EDGE_CURVE('',#5562,#5727,#3528,.T.);
#7186=EDGE_CURVE('',#5564,#5728,#766,.T.);
#7187=EDGE_CURVE('',#5563,#5729,#3529,.T.);
#7188=EDGE_CURVE('',#5728,#5729,#342,.T.);
#7189=EDGE_CURVE('',#5729,#5727,#3530,.T.);
#7190=EDGE_CURVE('',#5730,#5728,#4765,.T.);
#7191=EDGE_CURVE('',#5730,#5565,#767,.T.);
#7192=EDGE_CURVE('',#5731,#5730,#343,.T.);
#7193=EDGE_CURVE('',#5566,#5731,#3531,.T.);
#7194=EDGE_CURVE('',#5568,#5732,#768,.T.);
#7195=EDGE_CURVE('',#5567,#5733,#3532,.T.);
#7196=EDGE_CURVE('',#5732,#5733,#344,.T.);
#7197=EDGE_CURVE('',#5733,#5731,#3533,.T.);
#7198=EDGE_CURVE('',#5734,#5732,#4766,.T.);
#7199=EDGE_CURVE('',#5734,#5569,#769,.T.);
#7200=EDGE_CURVE('',#5735,#5734,#345,.T.);
#7201=EDGE_CURVE('',#5570,#5735,#3534,.T.);
#7202=EDGE_CURVE('',#5572,#5736,#770,.T.);
#7203=EDGE_CURVE('',#5571,#5737,#3535,.T.);
#7204=EDGE_CURVE('',#5736,#5737,#346,.T.);
#7205=EDGE_CURVE('',#5737,#5735,#3536,.T.);
#7206=EDGE_CURVE('',#5738,#5736,#4767,.T.);
#7207=EDGE_CURVE('',#5738,#5573,#771,.T.);
#7208=EDGE_CURVE('',#5739,#5738,#347,.T.);
#7209=EDGE_CURVE('',#5574,#5739,#3537,.T.);
#7210=EDGE_CURVE('',#5576,#5740,#772,.T.);
#7211=EDGE_CURVE('',#5575,#5741,#3538,.T.);
#7212=EDGE_CURVE('',#5740,#5741,#348,.T.);
#7213=EDGE_CURVE('',#5741,#5739,#3539,.T.);
#7214=EDGE_CURVE('',#5742,#5740,#4768,.T.);
#7215=EDGE_CURVE('',#5742,#5577,#773,.T.);
#7216=EDGE_CURVE('',#5743,#5742,#349,.T.);
#7217=EDGE_CURVE('',#5578,#5743,#3540,.T.);
#7218=EDGE_CURVE('',#5580,#5744,#774,.T.);
#7219=EDGE_CURVE('',#5579,#5745,#3541,.T.);
#7220=EDGE_CURVE('',#5744,#5745,#350,.T.);
#7221=EDGE_CURVE('',#5745,#5743,#3542,.T.);
#7222=EDGE_CURVE('',#5746,#5744,#4769,.T.);
#7223=EDGE_CURVE('',#5746,#5581,#775,.T.);
#7224=EDGE_CURVE('',#5747,#5746,#351,.T.);
#7225=EDGE_CURVE('',#5582,#5747,#3543,.T.);
#7226=EDGE_CURVE('',#5584,#5748,#776,.T.);
#7227=EDGE_CURVE('',#5583,#5749,#3544,.T.);
#7228=EDGE_CURVE('',#5748,#5749,#352,.T.);
#7229=EDGE_CURVE('',#5749,#5747,#3545,.T.);
#7230=EDGE_CURVE('',#5750,#5748,#4770,.T.);
#7231=EDGE_CURVE('',#5750,#5585,#777,.T.);
#7232=EDGE_CURVE('',#5751,#5750,#353,.T.);
#7233=EDGE_CURVE('',#5586,#5751,#3546,.T.);
#7234=EDGE_CURVE('',#5588,#5752,#778,.T.);
#7235=EDGE_CURVE('',#5587,#5753,#3547,.T.);
#7236=EDGE_CURVE('',#5752,#5753,#354,.T.);
#7237=EDGE_CURVE('',#5753,#5751,#3548,.T.);
#7238=EDGE_CURVE('',#5754,#5752,#4771,.T.);
#7239=EDGE_CURVE('',#5754,#5589,#779,.T.);
#7240=EDGE_CURVE('',#5755,#5754,#355,.T.);
#7241=EDGE_CURVE('',#5590,#5755,#3549,.T.);
#7242=EDGE_CURVE('',#5592,#5756,#780,.T.);
#7243=EDGE_CURVE('',#5591,#5757,#3550,.T.);
#7244=EDGE_CURVE('',#5756,#5757,#356,.T.);
#7245=EDGE_CURVE('',#5757,#5755,#3551,.T.);
#7246=EDGE_CURVE('',#5758,#5756,#4772,.T.);
#7247=EDGE_CURVE('',#5758,#5593,#781,.T.);
#7248=EDGE_CURVE('',#5759,#5758,#357,.T.);
#7249=EDGE_CURVE('',#5594,#5759,#3552,.T.);
#7250=EDGE_CURVE('',#5596,#5760,#782,.T.);
#7251=EDGE_CURVE('',#5595,#5761,#3553,.T.);
#7252=EDGE_CURVE('',#5760,#5761,#358,.T.);
#7253=EDGE_CURVE('',#5761,#5759,#3554,.T.);
#7254=EDGE_CURVE('',#5762,#5760,#4773,.T.);
#7255=EDGE_CURVE('',#5762,#5597,#783,.T.);
#7256=EDGE_CURVE('',#5763,#5762,#359,.T.);
#7257=EDGE_CURVE('',#5598,#5763,#3555,.T.);
#7258=EDGE_CURVE('',#5600,#5764,#784,.T.);
#7259=EDGE_CURVE('',#5599,#5765,#3556,.T.);
#7260=EDGE_CURVE('',#5764,#5765,#360,.T.);
#7261=EDGE_CURVE('',#5765,#5763,#3557,.T.);
#7262=EDGE_CURVE('',#5766,#5764,#4774,.T.);
#7263=EDGE_CURVE('',#5766,#5601,#785,.T.);
#7264=EDGE_CURVE('',#5767,#5766,#361,.T.);
#7265=EDGE_CURVE('',#5602,#5767,#3558,.T.);
#7266=EDGE_CURVE('',#5604,#5768,#786,.T.);
#7267=EDGE_CURVE('',#5603,#5769,#3559,.T.);
#7268=EDGE_CURVE('',#5768,#5769,#362,.T.);
#7269=EDGE_CURVE('',#5769,#5767,#3560,.T.);
#7270=EDGE_CURVE('',#5770,#5768,#4775,.T.);
#7271=EDGE_CURVE('',#5770,#5605,#787,.T.);
#7272=EDGE_CURVE('',#5771,#5770,#363,.T.);
#7273=EDGE_CURVE('',#5606,#5771,#3561,.T.);
#7274=EDGE_CURVE('',#5608,#5772,#788,.T.);
#7275=EDGE_CURVE('',#5607,#5773,#3562,.T.);
#7276=EDGE_CURVE('',#5772,#5773,#364,.T.);
#7277=EDGE_CURVE('',#5773,#5771,#3563,.T.);
#7278=EDGE_CURVE('',#5774,#5772,#4776,.T.);
#7279=EDGE_CURVE('',#5774,#5609,#789,.T.);
#7280=EDGE_CURVE('',#5775,#5774,#365,.T.);
#7281=EDGE_CURVE('',#5610,#5775,#3564,.T.);
#7282=EDGE_CURVE('',#5612,#5776,#790,.T.);
#7283=EDGE_CURVE('',#5611,#5777,#3565,.T.);
#7284=EDGE_CURVE('',#5776,#5777,#366,.T.);
#7285=EDGE_CURVE('',#5777,#5775,#3566,.T.);
#7286=EDGE_CURVE('',#5778,#5776,#4777,.T.);
#7287=EDGE_CURVE('',#5778,#5613,#791,.T.);
#7288=EDGE_CURVE('',#5779,#5778,#367,.T.);
#7289=EDGE_CURVE('',#5614,#5779,#3567,.T.);
#7290=EDGE_CURVE('',#5780,#5779,#3568,.T.);
#7291=EDGE_CURVE('',#5615,#5780,#3569,.T.);
#7292=EDGE_CURVE('',#5616,#5781,#792,.T.);
#7293=EDGE_CURVE('',#5781,#5780,#368,.T.);
#7294=EDGE_CURVE('',#5782,#5781,#4778,.T.);
#7295=EDGE_CURVE('',#5782,#5617,#793,.T.);
#7296=EDGE_CURVE('',#5620,#5783,#794,.T.);
#7297=EDGE_CURVE('',#5619,#5784,#3570,.T.);
#7298=EDGE_CURVE('',#5783,#5784,#369,.T.);
#7299=EDGE_CURVE('',#5785,#5782,#370,.T.);
#7300=EDGE_CURVE('',#5618,#5785,#3571,.T.);
#7301=EDGE_CURVE('',#5784,#5785,#3572,.T.);
#7302=EDGE_CURVE('',#5626,#5783,#4779,.T.);
#7303=EDGE_CURVE('',#5786,#5787,#3573,.T.);
#7304=EDGE_CURVE('',#5788,#5786,#3574,.T.);
#7305=EDGE_CURVE('',#5789,#5788,#3575,.T.);
#7306=EDGE_CURVE('',#5790,#5789,#3576,.T.);
#7307=EDGE_CURVE('',#5791,#5790,#3577,.T.);
#7308=EDGE_CURVE('',#5792,#5791,#3578,.T.);
#7309=EDGE_CURVE('',#5793,#5792,#3579,.T.);
#7310=EDGE_CURVE('',#5787,#5793,#3580,.T.);
#7311=EDGE_CURVE('',#5790,#5794,#3581,.T.);
#7312=EDGE_CURVE('',#5794,#5795,#3582,.T.);
#7313=EDGE_CURVE('',#5795,#5791,#3583,.T.);
#7314=EDGE_CURVE('',#5796,#5789,#3584,.T.);
#7315=EDGE_CURVE('',#5796,#5794,#3585,.T.);
#7316=EDGE_CURVE('',#5788,#5797,#3586,.T.);
#7317=EDGE_CURVE('',#5797,#5796,#3587,.T.);
#7318=EDGE_CURVE('',#5798,#5786,#3588,.T.);
#7319=EDGE_CURVE('',#5798,#5797,#3589,.T.);
#7320=EDGE_CURVE('',#5799,#5800,#3590,.T.);
#7321=EDGE_CURVE('',#5795,#5799,#3591,.T.);
#7322=EDGE_CURVE('',#5801,#5798,#3592,.T.);
#7323=EDGE_CURVE('',#5800,#5801,#3593,.T.);
#7324=EDGE_CURVE('',#5792,#5799,#3594,.T.);
#7325=EDGE_CURVE('',#5787,#5801,#3595,.T.);
#7326=EDGE_CURVE('',#5800,#5793,#3596,.T.);
#7327=EDGE_CURVE('',#5802,#5803,#3597,.T.);
#7328=EDGE_CURVE('',#5802,#5804,#3598,.T.);
#7329=EDGE_CURVE('',#5804,#5805,#3599,.T.);
#7330=EDGE_CURVE('',#5803,#5805,#3600,.T.);
#7331=EDGE_CURVE('',#5806,#5802,#3601,.T.);
#7332=EDGE_CURVE('',#5806,#5807,#3602,.T.);
#7333=EDGE_CURVE('',#5807,#5804,#3603,.T.);
#7334=EDGE_CURVE('',#5808,#5806,#3604,.T.);
#7335=EDGE_CURVE('',#5808,#5809,#3605,.T.);
#7336=EDGE_CURVE('',#5809,#5807,#3606,.T.);
#7337=EDGE_CURVE('',#5810,#5808,#3607,.T.);
#7338=EDGE_CURVE('',#5810,#5811,#3608,.T.);
#7339=EDGE_CURVE('',#5811,#5809,#3609,.T.);
#7340=EDGE_CURVE('',#5812,#5810,#3610,.T.);
#7341=EDGE_CURVE('',#5812,#5813,#3611,.T.);
#7342=EDGE_CURVE('',#5813,#5811,#3612,.T.);
#7343=EDGE_CURVE('',#5803,#5812,#3613,.T.);
#7344=EDGE_CURVE('',#5805,#5813,#3614,.T.);
#7345=EDGE_CURVE('',#5814,#5814,#4780,.T.);
#7346=EDGE_CURVE('',#5815,#5815,#4781,.T.);
#7347=EDGE_CURVE('',#5815,#5814,#3615,.T.);
#7348=EDGE_CURVE('',#5816,#5816,#4782,.F.);
#7349=EDGE_CURVE('',#5816,#5815,#3616,.T.);
#7350=EDGE_CURVE('',#5817,#5817,#4783,.T.);
#7351=EDGE_CURVE('',#5817,#5816,#3617,.T.);
#7352=ORIENTED_EDGE('',*,*,#5818,.F.);
#7353=ORIENTED_EDGE('',*,*,#5819,.T.);
#7354=ORIENTED_EDGE('',*,*,#5820,.F.);
#7355=ORIENTED_EDGE('',*,*,#5819,.F.);
#7356=ORIENTED_EDGE('',*,*,#5821,.F.);
#7357=ORIENTED_EDGE('',*,*,#5822,.T.);
#7358=ORIENTED_EDGE('',*,*,#5823,.F.);
#7359=ORIENTED_EDGE('',*,*,#5822,.F.);
#7360=ORIENTED_EDGE('',*,*,#5824,.F.);
#7361=ORIENTED_EDGE('',*,*,#5825,.T.);
#7362=ORIENTED_EDGE('',*,*,#5826,.F.);
#7363=ORIENTED_EDGE('',*,*,#5825,.F.);
#7364=ORIENTED_EDGE('',*,*,#5827,.F.);
#7365=ORIENTED_EDGE('',*,*,#5828,.T.);
#7366=ORIENTED_EDGE('',*,*,#5829,.F.);
#7367=ORIENTED_EDGE('',*,*,#5828,.F.);
#7368=ORIENTED_EDGE('',*,*,#5830,.T.);
#7369=ORIENTED_EDGE('',*,*,#5831,.T.);
#7370=ORIENTED_EDGE('',*,*,#5832,.F.);
#7371=ORIENTED_EDGE('',*,*,#5833,.F.);
#7372=ORIENTED_EDGE('',*,*,#5834,.T.);
#7373=ORIENTED_EDGE('',*,*,#5833,.T.);
#7374=ORIENTED_EDGE('',*,*,#5835,.F.);
#7375=ORIENTED_EDGE('',*,*,#5836,.F.);
#7376=ORIENTED_EDGE('',*,*,#5837,.T.);
#7377=ORIENTED_EDGE('',*,*,#5836,.T.);
#7378=ORIENTED_EDGE('',*,*,#5838,.F.);
#7379=ORIENTED_EDGE('',*,*,#5839,.F.);
#7380=ORIENTED_EDGE('',*,*,#5840,.T.);
#7381=ORIENTED_EDGE('',*,*,#5839,.T.);
#7382=ORIENTED_EDGE('',*,*,#5841,.F.);
#7383=ORIENTED_EDGE('',*,*,#5831,.F.);
#7384=ORIENTED_EDGE('',*,*,#5841,.T.);
#7385=ORIENTED_EDGE('',*,*,#5838,.T.);
#7386=ORIENTED_EDGE('',*,*,#5835,.T.);
#7387=ORIENTED_EDGE('',*,*,#5832,.T.);
#7388=ORIENTED_EDGE('',*,*,#5820,.T.);
#7389=ORIENTED_EDGE('',*,*,#5823,.T.);
#7390=ORIENTED_EDGE('',*,*,#5826,.T.);
#7391=ORIENTED_EDGE('',*,*,#5829,.T.);
#7392=ORIENTED_EDGE('',*,*,#5840,.F.);
#7393=ORIENTED_EDGE('',*,*,#5830,.F.);
#7394=ORIENTED_EDGE('',*,*,#5834,.F.);
#7395=ORIENTED_EDGE('',*,*,#5837,.F.);
#7396=ORIENTED_EDGE('',*,*,#5818,.T.);
#7397=ORIENTED_EDGE('',*,*,#5821,.T.);
#7398=ORIENTED_EDGE('',*,*,#5824,.T.);
#7399=ORIENTED_EDGE('',*,*,#5827,.T.);
#7400=ORIENTED_EDGE('',*,*,#5842,.F.);
#7401=ORIENTED_EDGE('',*,*,#5843,.T.);
#7402=ORIENTED_EDGE('',*,*,#5844,.F.);
#7403=ORIENTED_EDGE('',*,*,#5843,.F.);
#7404=ORIENTED_EDGE('',*,*,#5845,.F.);
#7405=ORIENTED_EDGE('',*,*,#5846,.T.);
#7406=ORIENTED_EDGE('',*,*,#5847,.F.);
#7407=ORIENTED_EDGE('',*,*,#5846,.F.);
#7408=ORIENTED_EDGE('',*,*,#5848,.F.);
#7409=ORIENTED_EDGE('',*,*,#5849,.T.);
#7410=ORIENTED_EDGE('',*,*,#5850,.F.);
#7411=ORIENTED_EDGE('',*,*,#5849,.F.);
#7412=ORIENTED_EDGE('',*,*,#5851,.F.);
#7413=ORIENTED_EDGE('',*,*,#5852,.T.);
#7414=ORIENTED_EDGE('',*,*,#5853,.F.);
#7415=ORIENTED_EDGE('',*,*,#5852,.F.);
#7416=ORIENTED_EDGE('',*,*,#5854,.F.);
#7417=ORIENTED_EDGE('',*,*,#5855,.T.);
#7418=ORIENTED_EDGE('',*,*,#5856,.F.);
#7419=ORIENTED_EDGE('',*,*,#5855,.F.);
#7420=ORIENTED_EDGE('',*,*,#5857,.F.);
#7421=ORIENTED_EDGE('',*,*,#5858,.T.);
#7422=ORIENTED_EDGE('',*,*,#5859,.F.);
#7423=ORIENTED_EDGE('',*,*,#5858,.F.);
#7424=ORIENTED_EDGE('',*,*,#5860,.F.);
#7425=ORIENTED_EDGE('',*,*,#5861,.T.);
#7426=ORIENTED_EDGE('',*,*,#5862,.T.);
#7427=ORIENTED_EDGE('',*,*,#5861,.F.);
#7428=ORIENTED_EDGE('',*,*,#5862,.F.);
#7429=ORIENTED_EDGE('',*,*,#5863,.F.);
#7430=ORIENTED_EDGE('',*,*,#5864,.F.);
#7431=ORIENTED_EDGE('',*,*,#5865,.T.);
#7432=ORIENTED_EDGE('',*,*,#5866,.T.);
#7433=ORIENTED_EDGE('',*,*,#5865,.F.);
#7434=ORIENTED_EDGE('',*,*,#5866,.F.);
#7435=ORIENTED_EDGE('',*,*,#5867,.F.);
#7436=ORIENTED_EDGE('',*,*,#5868,.F.);
#7437=ORIENTED_EDGE('',*,*,#5869,.T.);
#7438=ORIENTED_EDGE('',*,*,#5870,.T.);
#7439=ORIENTED_EDGE('',*,*,#5869,.F.);
#7440=ORIENTED_EDGE('',*,*,#5870,.F.);
#7441=ORIENTED_EDGE('',*,*,#5871,.F.);
#7442=ORIENTED_EDGE('',*,*,#5872,.F.);
#7443=ORIENTED_EDGE('',*,*,#5873,.T.);
#7444=ORIENTED_EDGE('',*,*,#5874,.T.);
#7445=ORIENTED_EDGE('',*,*,#5873,.F.);
#7446=ORIENTED_EDGE('',*,*,#5874,.F.);
#7447=ORIENTED_EDGE('',*,*,#5875,.F.);
#7448=ORIENTED_EDGE('',*,*,#5863,.T.);
#7449=ORIENTED_EDGE('',*,*,#5876,.T.);
#7450=ORIENTED_EDGE('',*,*,#5877,.F.);
#7451=ORIENTED_EDGE('',*,*,#5876,.F.);
#7452=ORIENTED_EDGE('',*,*,#5867,.T.);
#7453=ORIENTED_EDGE('',*,*,#5878,.T.);
#7454=ORIENTED_EDGE('',*,*,#5879,.F.);
#7455=ORIENTED_EDGE('',*,*,#5878,.F.);
#7456=ORIENTED_EDGE('',*,*,#5871,.T.);
#7457=ORIENTED_EDGE('',*,*,#5880,.T.);
#7458=ORIENTED_EDGE('',*,*,#5881,.F.);
#7459=ORIENTED_EDGE('',*,*,#5880,.F.);
#7460=ORIENTED_EDGE('',*,*,#5875,.T.);
#7461=ORIENTED_EDGE('',*,*,#5882,.T.);
#7462=ORIENTED_EDGE('',*,*,#5883,.F.);
#7463=ORIENTED_EDGE('',*,*,#5882,.F.);
#7464=ORIENTED_EDGE('',*,*,#5884,.F.);
#7465=ORIENTED_EDGE('',*,*,#5885,.T.);
#7466=ORIENTED_EDGE('',*,*,#5886,.T.);
#7467=ORIENTED_EDGE('',*,*,#5885,.F.);
#7468=ORIENTED_EDGE('',*,*,#5886,.F.);
#7469=ORIENTED_EDGE('',*,*,#5887,.F.);
#7470=ORIENTED_EDGE('',*,*,#5888,.T.);
#7471=ORIENTED_EDGE('',*,*,#5889,.T.);
#7472=ORIENTED_EDGE('',*,*,#5888,.F.);
#7473=ORIENTED_EDGE('',*,*,#5889,.F.);
#7474=ORIENTED_EDGE('',*,*,#5890,.F.);
#7475=ORIENTED_EDGE('',*,*,#5891,.T.);
#7476=ORIENTED_EDGE('',*,*,#5892,.T.);
#7477=ORIENTED_EDGE('',*,*,#5891,.F.);
#7478=ORIENTED_EDGE('',*,*,#5892,.F.);
#7479=ORIENTED_EDGE('',*,*,#5893,.F.);
#7480=ORIENTED_EDGE('',*,*,#5893,.T.);
#7481=ORIENTED_EDGE('',*,*,#5894,.T.);
#7482=ORIENTED_EDGE('',*,*,#5895,.F.);
#7483=ORIENTED_EDGE('',*,*,#5894,.F.);
#7484=ORIENTED_EDGE('',*,*,#5896,.F.);
#7485=ORIENTED_EDGE('',*,*,#5897,.T.);
#7486=ORIENTED_EDGE('',*,*,#5898,.T.);
#7487=ORIENTED_EDGE('',*,*,#5897,.F.);
#7488=ORIENTED_EDGE('',*,*,#5898,.F.);
#7489=ORIENTED_EDGE('',*,*,#5899,.F.);
#7490=ORIENTED_EDGE('',*,*,#5899,.T.);
#7491=ORIENTED_EDGE('',*,*,#5900,.T.);
#7492=ORIENTED_EDGE('',*,*,#5901,.F.);
#7493=ORIENTED_EDGE('',*,*,#5900,.F.);
#7494=ORIENTED_EDGE('',*,*,#5902,.T.);
#7495=ORIENTED_EDGE('',*,*,#5903,.T.);
#7496=ORIENTED_EDGE('',*,*,#5904,.F.);
#7497=ORIENTED_EDGE('',*,*,#5905,.F.);
#7498=ORIENTED_EDGE('',*,*,#5853,.T.);
#7499=ORIENTED_EDGE('',*,*,#5856,.T.);
#7500=ORIENTED_EDGE('',*,*,#5859,.T.);
#7501=ORIENTED_EDGE('',*,*,#5901,.T.);
#7502=ORIENTED_EDGE('',*,*,#5895,.T.);
#7503=ORIENTED_EDGE('',*,*,#5883,.T.);
#7504=ORIENTED_EDGE('',*,*,#5881,.T.);
#7505=ORIENTED_EDGE('',*,*,#5879,.T.);
#7506=ORIENTED_EDGE('',*,*,#5877,.T.);
#7507=ORIENTED_EDGE('',*,*,#5850,.T.);
#7508=ORIENTED_EDGE('',*,*,#5847,.T.);
#7509=ORIENTED_EDGE('',*,*,#5844,.T.);
#7510=ORIENTED_EDGE('',*,*,#5906,.T.);
#7511=ORIENTED_EDGE('',*,*,#5905,.T.);
#7512=ORIENTED_EDGE('',*,*,#5907,.F.);
#7513=ORIENTED_EDGE('',*,*,#5908,.F.);
#7514=ORIENTED_EDGE('',*,*,#5909,.T.);
#7515=ORIENTED_EDGE('',*,*,#5908,.T.);
#7516=ORIENTED_EDGE('',*,*,#5910,.F.);
#7517=ORIENTED_EDGE('',*,*,#5911,.F.);
#7518=ORIENTED_EDGE('',*,*,#5851,.T.);
#7519=ORIENTED_EDGE('',*,*,#5854,.T.);
#7520=ORIENTED_EDGE('',*,*,#5857,.T.);
#7521=ORIENTED_EDGE('',*,*,#5890,.T.);
#7522=ORIENTED_EDGE('',*,*,#5896,.T.);
#7523=ORIENTED_EDGE('',*,*,#5872,.T.);
#7524=ORIENTED_EDGE('',*,*,#5868,.T.);
#7525=ORIENTED_EDGE('',*,*,#5864,.T.);
#7526=ORIENTED_EDGE('',*,*,#5860,.T.);
#7527=ORIENTED_EDGE('',*,*,#5848,.T.);
#7528=ORIENTED_EDGE('',*,*,#5845,.T.);
#7529=ORIENTED_EDGE('',*,*,#5842,.T.);
#7530=ORIENTED_EDGE('',*,*,#5912,.T.);
#7531=ORIENTED_EDGE('',*,*,#5911,.T.);
#7532=ORIENTED_EDGE('',*,*,#5913,.F.);
#7533=ORIENTED_EDGE('',*,*,#5903,.F.);
#7534=ORIENTED_EDGE('',*,*,#5913,.T.);
#7535=ORIENTED_EDGE('',*,*,#5910,.T.);
#7536=ORIENTED_EDGE('',*,*,#5907,.T.);
#7537=ORIENTED_EDGE('',*,*,#5904,.T.);
#7538=ORIENTED_EDGE('',*,*,#5912,.F.);
#7539=ORIENTED_EDGE('',*,*,#5902,.F.);
#7540=ORIENTED_EDGE('',*,*,#5906,.F.);
#7541=ORIENTED_EDGE('',*,*,#5909,.F.);
#7542=ORIENTED_EDGE('',*,*,#5884,.T.);
#7543=ORIENTED_EDGE('',*,*,#5887,.T.);
#7544=ORIENTED_EDGE('',*,*,#5914,.F.);
#7545=ORIENTED_EDGE('',*,*,#5915,.T.);
#7546=ORIENTED_EDGE('',*,*,#5916,.F.);
#7547=ORIENTED_EDGE('',*,*,#5915,.F.);
#7548=ORIENTED_EDGE('',*,*,#5917,.F.);
#7549=ORIENTED_EDGE('',*,*,#5918,.T.);
#7550=ORIENTED_EDGE('',*,*,#5919,.F.);
#7551=ORIENTED_EDGE('',*,*,#5918,.F.);
#7552=ORIENTED_EDGE('',*,*,#5920,.F.);
#7553=ORIENTED_EDGE('',*,*,#5921,.T.);
#7554=ORIENTED_EDGE('',*,*,#5922,.F.);
#7555=ORIENTED_EDGE('',*,*,#5921,.F.);
#7556=ORIENTED_EDGE('',*,*,#5923,.F.);
#7557=ORIENTED_EDGE('',*,*,#5924,.T.);
#7558=ORIENTED_EDGE('',*,*,#5925,.F.);
#7559=ORIENTED_EDGE('',*,*,#5924,.F.);
#7560=ORIENTED_EDGE('',*,*,#5926,.F.);
#7561=ORIENTED_EDGE('',*,*,#5927,.T.);
#7562=ORIENTED_EDGE('',*,*,#5928,.F.);
#7563=ORIENTED_EDGE('',*,*,#5927,.F.);
#7564=ORIENTED_EDGE('',*,*,#5929,.F.);
#7565=ORIENTED_EDGE('',*,*,#5930,.T.);
#7566=ORIENTED_EDGE('',*,*,#5931,.F.);
#7567=ORIENTED_EDGE('',*,*,#5930,.F.);
#7568=ORIENTED_EDGE('',*,*,#5932,.F.);
#7569=ORIENTED_EDGE('',*,*,#5933,.T.);
#7570=ORIENTED_EDGE('',*,*,#5934,.F.);
#7571=ORIENTED_EDGE('',*,*,#5933,.F.);
#7572=ORIENTED_EDGE('',*,*,#5932,.T.);
#7573=ORIENTED_EDGE('',*,*,#5935,.F.);
#7574=ORIENTED_EDGE('',*,*,#5936,.F.);
#7575=ORIENTED_EDGE('',*,*,#5937,.T.);
#7576=ORIENTED_EDGE('',*,*,#5938,.F.);
#7577=ORIENTED_EDGE('',*,*,#5937,.F.);
#7578=ORIENTED_EDGE('',*,*,#5936,.T.);
#7579=ORIENTED_EDGE('',*,*,#5939,.F.);
#7580=ORIENTED_EDGE('',*,*,#5940,.F.);
#7581=ORIENTED_EDGE('',*,*,#5941,.T.);
#7582=ORIENTED_EDGE('',*,*,#5942,.F.);
#7583=ORIENTED_EDGE('',*,*,#5941,.F.);
#7584=ORIENTED_EDGE('',*,*,#5940,.T.);
#7585=ORIENTED_EDGE('',*,*,#5943,.F.);
#7586=ORIENTED_EDGE('',*,*,#5944,.F.);
#7587=ORIENTED_EDGE('',*,*,#5945,.T.);
#7588=ORIENTED_EDGE('',*,*,#5946,.F.);
#7589=ORIENTED_EDGE('',*,*,#5945,.F.);
#7590=ORIENTED_EDGE('',*,*,#5944,.T.);
#7591=ORIENTED_EDGE('',*,*,#5947,.F.);
#7592=ORIENTED_EDGE('',*,*,#5948,.F.);
#7593=ORIENTED_EDGE('',*,*,#5949,.T.);
#7594=ORIENTED_EDGE('',*,*,#5935,.T.);
#7595=ORIENTED_EDGE('',*,*,#5949,.F.);
#7596=ORIENTED_EDGE('',*,*,#5950,.F.);
#7597=ORIENTED_EDGE('',*,*,#5951,.T.);
#7598=ORIENTED_EDGE('',*,*,#5939,.T.);
#7599=ORIENTED_EDGE('',*,*,#5951,.F.);
#7600=ORIENTED_EDGE('',*,*,#5952,.F.);
#7601=ORIENTED_EDGE('',*,*,#5953,.T.);
#7602=ORIENTED_EDGE('',*,*,#5943,.T.);
#7603=ORIENTED_EDGE('',*,*,#5953,.F.);
#7604=ORIENTED_EDGE('',*,*,#5954,.F.);
#7605=ORIENTED_EDGE('',*,*,#5955,.T.);
#7606=ORIENTED_EDGE('',*,*,#5947,.T.);
#7607=ORIENTED_EDGE('',*,*,#5955,.F.);
#7608=ORIENTED_EDGE('',*,*,#5956,.F.);
#7609=ORIENTED_EDGE('',*,*,#5957,.T.);
#7610=ORIENTED_EDGE('',*,*,#5958,.T.);
#7611=ORIENTED_EDGE('',*,*,#5957,.F.);
#7612=ORIENTED_EDGE('',*,*,#5958,.F.);
#7613=ORIENTED_EDGE('',*,*,#5959,.F.);
#7614=ORIENTED_EDGE('',*,*,#5960,.T.);
#7615=ORIENTED_EDGE('',*,*,#5961,.T.);
#7616=ORIENTED_EDGE('',*,*,#5960,.F.);
#7617=ORIENTED_EDGE('',*,*,#5961,.F.);
#7618=ORIENTED_EDGE('',*,*,#5962,.F.);
#7619=ORIENTED_EDGE('',*,*,#5963,.T.);
#7620=ORIENTED_EDGE('',*,*,#5964,.F.);
#7621=ORIENTED_EDGE('',*,*,#5963,.F.);
#7622=ORIENTED_EDGE('',*,*,#5962,.T.);
#7623=ORIENTED_EDGE('',*,*,#5965,.F.);
#7624=ORIENTED_EDGE('',*,*,#5966,.F.);
#7625=ORIENTED_EDGE('',*,*,#5967,.T.);
#7626=ORIENTED_EDGE('',*,*,#5965,.T.);
#7627=ORIENTED_EDGE('',*,*,#5967,.F.);
#7628=ORIENTED_EDGE('',*,*,#5968,.F.);
#7629=ORIENTED_EDGE('',*,*,#5969,.T.);
#7630=ORIENTED_EDGE('',*,*,#5970,.F.);
#7631=ORIENTED_EDGE('',*,*,#5969,.F.);
#7632=ORIENTED_EDGE('',*,*,#5968,.T.);
#7633=ORIENTED_EDGE('',*,*,#5971,.F.);
#7634=ORIENTED_EDGE('',*,*,#5972,.F.);
#7635=ORIENTED_EDGE('',*,*,#5973,.T.);
#7636=ORIENTED_EDGE('',*,*,#5971,.T.);
#7637=ORIENTED_EDGE('',*,*,#5973,.F.);
#7638=ORIENTED_EDGE('',*,*,#5974,.T.);
#7639=ORIENTED_EDGE('',*,*,#5975,.T.);
#7640=ORIENTED_EDGE('',*,*,#5976,.F.);
#7641=ORIENTED_EDGE('',*,*,#5977,.F.);
#7642=ORIENTED_EDGE('',*,*,#5925,.T.);
#7643=ORIENTED_EDGE('',*,*,#5928,.T.);
#7644=ORIENTED_EDGE('',*,*,#5931,.T.);
#7645=ORIENTED_EDGE('',*,*,#5964,.T.);
#7646=ORIENTED_EDGE('',*,*,#5970,.T.);
#7647=ORIENTED_EDGE('',*,*,#5946,.T.);
#7648=ORIENTED_EDGE('',*,*,#5942,.T.);
#7649=ORIENTED_EDGE('',*,*,#5938,.T.);
#7650=ORIENTED_EDGE('',*,*,#5934,.T.);
#7651=ORIENTED_EDGE('',*,*,#5922,.T.);
#7652=ORIENTED_EDGE('',*,*,#5919,.T.);
#7653=ORIENTED_EDGE('',*,*,#5916,.T.);
#7654=ORIENTED_EDGE('',*,*,#5978,.T.);
#7655=ORIENTED_EDGE('',*,*,#5977,.T.);
#7656=ORIENTED_EDGE('',*,*,#5979,.F.);
#7657=ORIENTED_EDGE('',*,*,#5980,.F.);
#7658=ORIENTED_EDGE('',*,*,#5981,.T.);
#7659=ORIENTED_EDGE('',*,*,#5980,.T.);
#7660=ORIENTED_EDGE('',*,*,#5982,.F.);
#7661=ORIENTED_EDGE('',*,*,#5983,.F.);
#7662=ORIENTED_EDGE('',*,*,#5923,.T.);
#7663=ORIENTED_EDGE('',*,*,#5926,.T.);
#7664=ORIENTED_EDGE('',*,*,#5929,.T.);
#7665=ORIENTED_EDGE('',*,*,#5972,.T.);
#7666=ORIENTED_EDGE('',*,*,#5966,.T.);
#7667=ORIENTED_EDGE('',*,*,#5954,.T.);
#7668=ORIENTED_EDGE('',*,*,#5952,.T.);
#7669=ORIENTED_EDGE('',*,*,#5950,.T.);
#7670=ORIENTED_EDGE('',*,*,#5948,.T.);
#7671=ORIENTED_EDGE('',*,*,#5920,.T.);
#7672=ORIENTED_EDGE('',*,*,#5917,.T.);
#7673=ORIENTED_EDGE('',*,*,#5914,.T.);
#7674=ORIENTED_EDGE('',*,*,#5984,.T.);
#7675=ORIENTED_EDGE('',*,*,#5983,.T.);
#7676=ORIENTED_EDGE('',*,*,#5985,.F.);
#7677=ORIENTED_EDGE('',*,*,#5975,.F.);
#7678=ORIENTED_EDGE('',*,*,#5985,.T.);
#7679=ORIENTED_EDGE('',*,*,#5982,.T.);
#7680=ORIENTED_EDGE('',*,*,#5979,.T.);
#7681=ORIENTED_EDGE('',*,*,#5976,.T.);
#7682=ORIENTED_EDGE('',*,*,#5984,.F.);
#7683=ORIENTED_EDGE('',*,*,#5974,.F.);
#7684=ORIENTED_EDGE('',*,*,#5978,.F.);
#7685=ORIENTED_EDGE('',*,*,#5981,.F.);
#7686=ORIENTED_EDGE('',*,*,#5956,.T.);
#7687=ORIENTED_EDGE('',*,*,#5959,.T.);
#7688=ORIENTED_EDGE('',*,*,#5986,.F.);
#7689=ORIENTED_EDGE('',*,*,#5987,.T.);
#7690=ORIENTED_EDGE('',*,*,#5988,.T.);
#7691=ORIENTED_EDGE('',*,*,#5987,.F.);
#7692=ORIENTED_EDGE('',*,*,#5989,.F.);
#7693=ORIENTED_EDGE('',*,*,#5990,.T.);
#7694=ORIENTED_EDGE('',*,*,#5991,.T.);
#7695=ORIENTED_EDGE('',*,*,#5990,.F.);
#7696=ORIENTED_EDGE('',*,*,#5989,.T.);
#7697=ORIENTED_EDGE('',*,*,#5986,.T.);
#7698=ORIENTED_EDGE('',*,*,#5991,.F.);
#7699=ORIENTED_EDGE('',*,*,#5988,.F.);
#7700=ORIENTED_EDGE('',*,*,#5992,.F.);
#7701=ORIENTED_EDGE('',*,*,#5993,.T.);
#7702=ORIENTED_EDGE('',*,*,#5994,.T.);
#7703=ORIENTED_EDGE('',*,*,#5993,.F.);
#7704=ORIENTED_EDGE('',*,*,#5995,.F.);
#7705=ORIENTED_EDGE('',*,*,#5996,.T.);
#7706=ORIENTED_EDGE('',*,*,#5997,.T.);
#7707=ORIENTED_EDGE('',*,*,#5996,.F.);
#7708=ORIENTED_EDGE('',*,*,#5995,.T.);
#7709=ORIENTED_EDGE('',*,*,#5992,.T.);
#7710=ORIENTED_EDGE('',*,*,#5997,.F.);
#7711=ORIENTED_EDGE('',*,*,#5994,.F.);
#7712=ORIENTED_EDGE('',*,*,#5998,.F.);
#7713=ORIENTED_EDGE('',*,*,#5999,.T.);
#7714=ORIENTED_EDGE('',*,*,#6000,.T.);
#7715=ORIENTED_EDGE('',*,*,#5999,.F.);
#7716=ORIENTED_EDGE('',*,*,#6001,.F.);
#7717=ORIENTED_EDGE('',*,*,#6002,.T.);
#7718=ORIENTED_EDGE('',*,*,#6003,.T.);
#7719=ORIENTED_EDGE('',*,*,#6002,.F.);
#7720=ORIENTED_EDGE('',*,*,#6001,.T.);
#7721=ORIENTED_EDGE('',*,*,#5998,.T.);
#7722=ORIENTED_EDGE('',*,*,#6003,.F.);
#7723=ORIENTED_EDGE('',*,*,#6000,.F.);
#7724=ORIENTED_EDGE('',*,*,#6004,.F.);
#7725=ORIENTED_EDGE('',*,*,#6005,.T.);
#7726=ORIENTED_EDGE('',*,*,#6006,.T.);
#7727=ORIENTED_EDGE('',*,*,#6005,.F.);
#7728=ORIENTED_EDGE('',*,*,#6007,.F.);
#7729=ORIENTED_EDGE('',*,*,#6008,.T.);
#7730=ORIENTED_EDGE('',*,*,#6009,.T.);
#7731=ORIENTED_EDGE('',*,*,#6008,.F.);
#7732=ORIENTED_EDGE('',*,*,#6007,.T.);
#7733=ORIENTED_EDGE('',*,*,#6004,.T.);
#7734=ORIENTED_EDGE('',*,*,#6009,.F.);
#7735=ORIENTED_EDGE('',*,*,#6006,.F.);
#7736=ORIENTED_EDGE('',*,*,#6010,.F.);
#7737=ORIENTED_EDGE('',*,*,#6011,.T.);
#7738=ORIENTED_EDGE('',*,*,#6012,.F.);
#7739=ORIENTED_EDGE('',*,*,#6011,.F.);
#7740=ORIENTED_EDGE('',*,*,#6013,.F.);
#7741=ORIENTED_EDGE('',*,*,#6014,.T.);
#7742=ORIENTED_EDGE('',*,*,#6015,.F.);
#7743=ORIENTED_EDGE('',*,*,#6014,.F.);
#7744=ORIENTED_EDGE('',*,*,#6016,.F.);
#7745=ORIENTED_EDGE('',*,*,#6017,.T.);
#7746=ORIENTED_EDGE('',*,*,#6018,.F.);
#7747=ORIENTED_EDGE('',*,*,#6017,.F.);
#7748=ORIENTED_EDGE('',*,*,#6019,.F.);
#7749=ORIENTED_EDGE('',*,*,#6020,.T.);
#7750=ORIENTED_EDGE('',*,*,#6021,.F.);
#7751=ORIENTED_EDGE('',*,*,#6020,.F.);
#7752=ORIENTED_EDGE('',*,*,#6019,.T.);
#7753=ORIENTED_EDGE('',*,*,#6022,.T.);
#7754=ORIENTED_EDGE('',*,*,#6022,.F.);
#7755=ORIENTED_EDGE('',*,*,#6023,.T.);
#7756=ORIENTED_EDGE('',*,*,#6024,.T.);
#7757=ORIENTED_EDGE('',*,*,#6023,.F.);
#7758=ORIENTED_EDGE('',*,*,#6025,.F.);
#7759=ORIENTED_EDGE('',*,*,#6026,.T.);
#7760=ORIENTED_EDGE('',*,*,#6027,.T.);
#7761=ORIENTED_EDGE('',*,*,#6026,.F.);
#7762=ORIENTED_EDGE('',*,*,#6025,.T.);
#7763=ORIENTED_EDGE('',*,*,#6012,.T.);
#7764=ORIENTED_EDGE('',*,*,#6015,.T.);
#7765=ORIENTED_EDGE('',*,*,#6018,.T.);
#7766=ORIENTED_EDGE('',*,*,#6021,.T.);
#7767=ORIENTED_EDGE('',*,*,#6027,.F.);
#7768=ORIENTED_EDGE('',*,*,#6010,.T.);
#7769=ORIENTED_EDGE('',*,*,#6013,.T.);
#7770=ORIENTED_EDGE('',*,*,#6016,.T.);
#7771=ORIENTED_EDGE('',*,*,#6024,.F.);
#7772=ORIENTED_EDGE('',*,*,#6028,.F.);
#7773=ORIENTED_EDGE('',*,*,#6029,.T.);
#7774=ORIENTED_EDGE('',*,*,#6030,.F.);
#7775=ORIENTED_EDGE('',*,*,#6029,.F.);
#7776=ORIENTED_EDGE('',*,*,#6031,.F.);
#7777=ORIENTED_EDGE('',*,*,#6032,.T.);
#7778=ORIENTED_EDGE('',*,*,#6033,.F.);
#7779=ORIENTED_EDGE('',*,*,#6032,.F.);
#7780=ORIENTED_EDGE('',*,*,#6034,.F.);
#7781=ORIENTED_EDGE('',*,*,#6035,.T.);
#7782=ORIENTED_EDGE('',*,*,#6036,.F.);
#7783=ORIENTED_EDGE('',*,*,#6035,.F.);
#7784=ORIENTED_EDGE('',*,*,#6037,.F.);
#7785=ORIENTED_EDGE('',*,*,#6038,.T.);
#7786=ORIENTED_EDGE('',*,*,#6039,.F.);
#7787=ORIENTED_EDGE('',*,*,#6038,.F.);
#7788=ORIENTED_EDGE('',*,*,#6037,.T.);
#7789=ORIENTED_EDGE('',*,*,#6040,.T.);
#7790=ORIENTED_EDGE('',*,*,#6040,.F.);
#7791=ORIENTED_EDGE('',*,*,#6041,.T.);
#7792=ORIENTED_EDGE('',*,*,#6042,.T.);
#7793=ORIENTED_EDGE('',*,*,#6041,.F.);
#7794=ORIENTED_EDGE('',*,*,#6043,.F.);
#7795=ORIENTED_EDGE('',*,*,#6044,.T.);
#7796=ORIENTED_EDGE('',*,*,#6045,.T.);
#7797=ORIENTED_EDGE('',*,*,#6044,.F.);
#7798=ORIENTED_EDGE('',*,*,#6043,.T.);
#7799=ORIENTED_EDGE('',*,*,#6030,.T.);
#7800=ORIENTED_EDGE('',*,*,#6033,.T.);
#7801=ORIENTED_EDGE('',*,*,#6036,.T.);
#7802=ORIENTED_EDGE('',*,*,#6039,.T.);
#7803=ORIENTED_EDGE('',*,*,#6045,.F.);
#7804=ORIENTED_EDGE('',*,*,#6028,.T.);
#7805=ORIENTED_EDGE('',*,*,#6031,.T.);
#7806=ORIENTED_EDGE('',*,*,#6034,.T.);
#7807=ORIENTED_EDGE('',*,*,#6042,.F.);
#7808=ORIENTED_EDGE('',*,*,#6046,.F.);
#7809=ORIENTED_EDGE('',*,*,#6047,.T.);
#7810=ORIENTED_EDGE('',*,*,#6048,.F.);
#7811=ORIENTED_EDGE('',*,*,#6047,.F.);
#7812=ORIENTED_EDGE('',*,*,#6049,.F.);
#7813=ORIENTED_EDGE('',*,*,#6050,.T.);
#7814=ORIENTED_EDGE('',*,*,#6051,.F.);
#7815=ORIENTED_EDGE('',*,*,#6050,.F.);
#7816=ORIENTED_EDGE('',*,*,#6052,.F.);
#7817=ORIENTED_EDGE('',*,*,#6053,.T.);
#7818=ORIENTED_EDGE('',*,*,#6054,.F.);
#7819=ORIENTED_EDGE('',*,*,#6053,.F.);
#7820=ORIENTED_EDGE('',*,*,#6055,.F.);
#7821=ORIENTED_EDGE('',*,*,#6056,.T.);
#7822=ORIENTED_EDGE('',*,*,#6057,.T.);
#7823=ORIENTED_EDGE('',*,*,#6056,.F.);
#7824=ORIENTED_EDGE('',*,*,#6057,.F.);
#7825=ORIENTED_EDGE('',*,*,#6058,.F.);
#7826=ORIENTED_EDGE('',*,*,#6059,.F.);
#7827=ORIENTED_EDGE('',*,*,#6060,.T.);
#7828=ORIENTED_EDGE('',*,*,#6058,.T.);
#7829=ORIENTED_EDGE('',*,*,#6060,.F.);
#7830=ORIENTED_EDGE('',*,*,#6061,.F.);
#7831=ORIENTED_EDGE('',*,*,#6062,.T.);
#7832=ORIENTED_EDGE('',*,*,#6063,.T.);
#7833=ORIENTED_EDGE('',*,*,#6062,.F.);
#7834=ORIENTED_EDGE('',*,*,#6061,.T.);
#7835=ORIENTED_EDGE('',*,*,#6048,.T.);
#7836=ORIENTED_EDGE('',*,*,#6051,.T.);
#7837=ORIENTED_EDGE('',*,*,#6054,.T.);
#7838=ORIENTED_EDGE('',*,*,#6059,.T.);
#7839=ORIENTED_EDGE('',*,*,#6063,.F.);
#7840=ORIENTED_EDGE('',*,*,#6046,.T.);
#7841=ORIENTED_EDGE('',*,*,#6049,.T.);
#7842=ORIENTED_EDGE('',*,*,#6052,.T.);
#7843=ORIENTED_EDGE('',*,*,#6055,.T.);
#7844=ORIENTED_EDGE('',*,*,#6064,.F.);
#7845=ORIENTED_EDGE('',*,*,#6065,.T.);
#7846=ORIENTED_EDGE('',*,*,#6066,.F.);
#7847=ORIENTED_EDGE('',*,*,#6065,.F.);
#7848=ORIENTED_EDGE('',*,*,#6067,.F.);
#7849=ORIENTED_EDGE('',*,*,#6068,.T.);
#7850=ORIENTED_EDGE('',*,*,#6069,.F.);
#7851=ORIENTED_EDGE('',*,*,#6068,.F.);
#7852=ORIENTED_EDGE('',*,*,#6070,.F.);
#7853=ORIENTED_EDGE('',*,*,#6071,.T.);
#7854=ORIENTED_EDGE('',*,*,#6072,.F.);
#7855=ORIENTED_EDGE('',*,*,#6071,.F.);
#7856=ORIENTED_EDGE('',*,*,#6073,.F.);
#7857=ORIENTED_EDGE('',*,*,#6074,.T.);
#7858=ORIENTED_EDGE('',*,*,#6075,.T.);
#7859=ORIENTED_EDGE('',*,*,#6074,.F.);
#7860=ORIENTED_EDGE('',*,*,#6075,.F.);
#7861=ORIENTED_EDGE('',*,*,#6076,.F.);
#7862=ORIENTED_EDGE('',*,*,#6077,.F.);
#7863=ORIENTED_EDGE('',*,*,#6078,.T.);
#7864=ORIENTED_EDGE('',*,*,#6076,.T.);
#7865=ORIENTED_EDGE('',*,*,#6078,.F.);
#7866=ORIENTED_EDGE('',*,*,#6079,.F.);
#7867=ORIENTED_EDGE('',*,*,#6080,.T.);
#7868=ORIENTED_EDGE('',*,*,#6081,.T.);
#7869=ORIENTED_EDGE('',*,*,#6080,.F.);
#7870=ORIENTED_EDGE('',*,*,#6079,.T.);
#7871=ORIENTED_EDGE('',*,*,#6066,.T.);
#7872=ORIENTED_EDGE('',*,*,#6069,.T.);
#7873=ORIENTED_EDGE('',*,*,#6072,.T.);
#7874=ORIENTED_EDGE('',*,*,#6077,.T.);
#7875=ORIENTED_EDGE('',*,*,#6081,.F.);
#7876=ORIENTED_EDGE('',*,*,#6064,.T.);
#7877=ORIENTED_EDGE('',*,*,#6067,.T.);
#7878=ORIENTED_EDGE('',*,*,#6070,.T.);
#7879=ORIENTED_EDGE('',*,*,#6073,.T.);
#7880=ORIENTED_EDGE('',*,*,#6082,.F.);
#7881=ORIENTED_EDGE('',*,*,#6083,.F.);
#7882=ORIENTED_EDGE('',*,*,#6084,.T.);
#7883=ORIENTED_EDGE('',*,*,#6082,.T.);
#7884=ORIENTED_EDGE('',*,*,#6084,.F.);
#7885=ORIENTED_EDGE('',*,*,#6085,.F.);
#7886=ORIENTED_EDGE('',*,*,#6086,.T.);
#7887=ORIENTED_EDGE('',*,*,#6083,.T.);
#7888=ORIENTED_EDGE('',*,*,#6086,.F.);
#7889=ORIENTED_EDGE('',*,*,#6087,.F.);
#7890=ORIENTED_EDGE('',*,*,#6088,.T.);
#7891=ORIENTED_EDGE('',*,*,#6085,.T.);
#7892=ORIENTED_EDGE('',*,*,#6088,.F.);
#7893=ORIENTED_EDGE('',*,*,#6087,.T.);
#7894=ORIENTED_EDGE('',*,*,#6089,.F.);
#7895=ORIENTED_EDGE('',*,*,#6090,.F.);
#7896=ORIENTED_EDGE('',*,*,#6091,.T.);
#7897=ORIENTED_EDGE('',*,*,#6089,.T.);
#7898=ORIENTED_EDGE('',*,*,#6091,.F.);
#7899=ORIENTED_EDGE('',*,*,#6092,.F.);
#7900=ORIENTED_EDGE('',*,*,#6093,.T.);
#7901=ORIENTED_EDGE('',*,*,#6090,.T.);
#7902=ORIENTED_EDGE('',*,*,#6093,.F.);
#7903=ORIENTED_EDGE('',*,*,#6094,.F.);
#7904=ORIENTED_EDGE('',*,*,#6095,.T.);
#7905=ORIENTED_EDGE('',*,*,#6092,.T.);
#7906=ORIENTED_EDGE('',*,*,#6095,.F.);
#7907=ORIENTED_EDGE('',*,*,#6094,.T.);
#7908=ORIENTED_EDGE('',*,*,#6096,.T.);
#7909=ORIENTED_EDGE('',*,*,#6097,.T.);
#7910=ORIENTED_EDGE('',*,*,#6098,.T.);
#7911=ORIENTED_EDGE('',*,*,#6099,.F.);
#7912=ORIENTED_EDGE('',*,*,#6100,.T.);
#7913=ORIENTED_EDGE('',*,*,#6101,.T.);
#7914=ORIENTED_EDGE('',*,*,#6102,.T.);
#7915=ORIENTED_EDGE('',*,*,#6097,.F.);
#7916=ORIENTED_EDGE('',*,*,#6103,.T.);
#7917=ORIENTED_EDGE('',*,*,#6104,.T.);
#7918=ORIENTED_EDGE('',*,*,#6105,.T.);
#7919=ORIENTED_EDGE('',*,*,#6101,.F.);
#7920=ORIENTED_EDGE('',*,*,#6106,.T.);
#7921=ORIENTED_EDGE('',*,*,#6107,.T.);
#7922=ORIENTED_EDGE('',*,*,#6108,.T.);
#7923=ORIENTED_EDGE('',*,*,#6104,.F.);
#7924=ORIENTED_EDGE('',*,*,#6109,.T.);
#7925=ORIENTED_EDGE('',*,*,#6110,.T.);
#7926=ORIENTED_EDGE('',*,*,#6111,.T.);
#7927=ORIENTED_EDGE('',*,*,#6107,.F.);
#7928=ORIENTED_EDGE('',*,*,#6112,.T.);
#7929=ORIENTED_EDGE('',*,*,#6099,.T.);
#7930=ORIENTED_EDGE('',*,*,#6113,.T.);
#7931=ORIENTED_EDGE('',*,*,#6110,.F.);
#7932=ORIENTED_EDGE('',*,*,#6112,.F.);
#7933=ORIENTED_EDGE('',*,*,#6109,.F.);
#7934=ORIENTED_EDGE('',*,*,#6106,.F.);
#7935=ORIENTED_EDGE('',*,*,#6103,.F.);
#7936=ORIENTED_EDGE('',*,*,#6100,.F.);
#7937=ORIENTED_EDGE('',*,*,#6096,.F.);
#7938=ORIENTED_EDGE('',*,*,#6113,.F.);
#7939=ORIENTED_EDGE('',*,*,#6098,.F.);
#7940=ORIENTED_EDGE('',*,*,#6102,.F.);
#7941=ORIENTED_EDGE('',*,*,#6105,.F.);
#7942=ORIENTED_EDGE('',*,*,#6108,.F.);
#7943=ORIENTED_EDGE('',*,*,#6111,.F.);
#7944=ORIENTED_EDGE('',*,*,#6114,.F.);
#7945=ORIENTED_EDGE('',*,*,#6115,.F.);
#7946=ORIENTED_EDGE('',*,*,#6116,.T.);
#7947=ORIENTED_EDGE('',*,*,#6114,.T.);
#7948=ORIENTED_EDGE('',*,*,#6116,.F.);
#7949=ORIENTED_EDGE('',*,*,#6117,.F.);
#7950=ORIENTED_EDGE('',*,*,#6118,.T.);
#7951=ORIENTED_EDGE('',*,*,#6115,.T.);
#7952=ORIENTED_EDGE('',*,*,#6118,.F.);
#7953=ORIENTED_EDGE('',*,*,#6119,.F.);
#7954=ORIENTED_EDGE('',*,*,#6120,.T.);
#7955=ORIENTED_EDGE('',*,*,#6117,.T.);
#7956=ORIENTED_EDGE('',*,*,#6120,.F.);
#7957=ORIENTED_EDGE('',*,*,#6119,.T.);
#7958=ORIENTED_EDGE('',*,*,#6121,.F.);
#7959=ORIENTED_EDGE('',*,*,#6122,.F.);
#7960=ORIENTED_EDGE('',*,*,#6123,.T.);
#7961=ORIENTED_EDGE('',*,*,#6121,.T.);
#7962=ORIENTED_EDGE('',*,*,#6123,.F.);
#7963=ORIENTED_EDGE('',*,*,#6124,.F.);
#7964=ORIENTED_EDGE('',*,*,#6125,.T.);
#7965=ORIENTED_EDGE('',*,*,#6122,.T.);
#7966=ORIENTED_EDGE('',*,*,#6125,.F.);
#7967=ORIENTED_EDGE('',*,*,#6126,.F.);
#7968=ORIENTED_EDGE('',*,*,#6127,.T.);
#7969=ORIENTED_EDGE('',*,*,#6124,.T.);
#7970=ORIENTED_EDGE('',*,*,#6127,.F.);
#7971=ORIENTED_EDGE('',*,*,#6126,.T.);
#7972=ORIENTED_EDGE('',*,*,#6128,.T.);
#7973=ORIENTED_EDGE('',*,*,#6129,.T.);
#7974=ORIENTED_EDGE('',*,*,#6130,.T.);
#7975=ORIENTED_EDGE('',*,*,#6131,.F.);
#7976=ORIENTED_EDGE('',*,*,#6132,.T.);
#7977=ORIENTED_EDGE('',*,*,#6133,.T.);
#7978=ORIENTED_EDGE('',*,*,#6134,.T.);
#7979=ORIENTED_EDGE('',*,*,#6129,.F.);
#7980=ORIENTED_EDGE('',*,*,#6135,.T.);
#7981=ORIENTED_EDGE('',*,*,#6136,.T.);
#7982=ORIENTED_EDGE('',*,*,#6137,.T.);
#7983=ORIENTED_EDGE('',*,*,#6133,.F.);
#7984=ORIENTED_EDGE('',*,*,#6138,.T.);
#7985=ORIENTED_EDGE('',*,*,#6139,.T.);
#7986=ORIENTED_EDGE('',*,*,#6140,.T.);
#7987=ORIENTED_EDGE('',*,*,#6136,.F.);
#7988=ORIENTED_EDGE('',*,*,#6141,.T.);
#7989=ORIENTED_EDGE('',*,*,#6142,.T.);
#7990=ORIENTED_EDGE('',*,*,#6143,.T.);
#7991=ORIENTED_EDGE('',*,*,#6139,.F.);
#7992=ORIENTED_EDGE('',*,*,#6144,.T.);
#7993=ORIENTED_EDGE('',*,*,#6131,.T.);
#7994=ORIENTED_EDGE('',*,*,#6145,.T.);
#7995=ORIENTED_EDGE('',*,*,#6142,.F.);
#7996=ORIENTED_EDGE('',*,*,#6144,.F.);
#7997=ORIENTED_EDGE('',*,*,#6141,.F.);
#7998=ORIENTED_EDGE('',*,*,#6138,.F.);
#7999=ORIENTED_EDGE('',*,*,#6135,.F.);
#8000=ORIENTED_EDGE('',*,*,#6132,.F.);
#8001=ORIENTED_EDGE('',*,*,#6128,.F.);
#8002=ORIENTED_EDGE('',*,*,#6145,.F.);
#8003=ORIENTED_EDGE('',*,*,#6130,.F.);
#8004=ORIENTED_EDGE('',*,*,#6134,.F.);
#8005=ORIENTED_EDGE('',*,*,#6137,.F.);
#8006=ORIENTED_EDGE('',*,*,#6140,.F.);
#8007=ORIENTED_EDGE('',*,*,#6143,.F.);
#8008=ORIENTED_EDGE('',*,*,#6146,.F.);
#8009=ORIENTED_EDGE('',*,*,#6147,.F.);
#8010=ORIENTED_EDGE('',*,*,#6148,.T.);
#8011=ORIENTED_EDGE('',*,*,#6149,.F.);
#8012=ORIENTED_EDGE('',*,*,#6150,.F.);
#8013=ORIENTED_EDGE('',*,*,#6148,.F.);
#8014=ORIENTED_EDGE('',*,*,#6149,.T.);
#8015=ORIENTED_EDGE('',*,*,#6150,.T.);
#8016=ORIENTED_EDGE('',*,*,#6151,.T.);
#8017=ORIENTED_EDGE('',*,*,#6152,.T.);
#8018=ORIENTED_EDGE('',*,*,#6151,.F.);
#8019=ORIENTED_EDGE('',*,*,#6153,.T.);
#8020=ORIENTED_EDGE('',*,*,#6154,.T.);
#8021=ORIENTED_EDGE('',*,*,#6155,.F.);
#8022=ORIENTED_EDGE('',*,*,#6154,.F.);
#8023=ORIENTED_EDGE('',*,*,#6155,.T.);
#8024=ORIENTED_EDGE('',*,*,#6156,.T.);
#8025=ORIENTED_EDGE('',*,*,#6157,.F.);
#8026=ORIENTED_EDGE('',*,*,#6156,.F.);
#8027=ORIENTED_EDGE('',*,*,#6152,.F.);
#8028=ORIENTED_EDGE('',*,*,#6157,.T.);
#8029=ORIENTED_EDGE('',*,*,#6158,.F.);
#8030=ORIENTED_EDGE('',*,*,#6159,.T.);
#8031=ORIENTED_EDGE('',*,*,#6146,.T.);
#8032=ORIENTED_EDGE('',*,*,#6147,.T.);
#8033=ORIENTED_EDGE('',*,*,#6159,.F.);
#8034=ORIENTED_EDGE('',*,*,#6158,.T.);
#8035=ORIENTED_EDGE('',*,*,#6160,.F.);
#8036=ORIENTED_EDGE('',*,*,#6160,.T.);
#8037=ORIENTED_EDGE('',*,*,#6161,.T.);
#8038=ORIENTED_EDGE('',*,*,#6153,.F.);
#8039=ORIENTED_EDGE('',*,*,#6161,.F.);
#8040=ORIENTED_EDGE('',*,*,#6162,.F.);
#8041=ORIENTED_EDGE('',*,*,#6163,.F.);
#8042=ORIENTED_EDGE('',*,*,#6164,.T.);
#8043=ORIENTED_EDGE('',*,*,#6165,.F.);
#8044=ORIENTED_EDGE('',*,*,#6166,.F.);
#8045=ORIENTED_EDGE('',*,*,#6164,.F.);
#8046=ORIENTED_EDGE('',*,*,#6167,.T.);
#8047=ORIENTED_EDGE('',*,*,#6168,.T.);
#8048=ORIENTED_EDGE('',*,*,#6165,.T.);
#8049=ORIENTED_EDGE('',*,*,#6166,.T.);
#8050=ORIENTED_EDGE('',*,*,#6168,.F.);
#8051=ORIENTED_EDGE('',*,*,#6169,.F.);
#8052=ORIENTED_EDGE('',*,*,#6170,.T.);
#8053=ORIENTED_EDGE('',*,*,#6171,.F.);
#8054=ORIENTED_EDGE('',*,*,#6172,.T.);
#8055=ORIENTED_EDGE('',*,*,#6169,.T.);
#8056=ORIENTED_EDGE('',*,*,#6172,.F.);
#8057=ORIENTED_EDGE('',*,*,#6173,.F.);
#8058=ORIENTED_EDGE('',*,*,#6174,.T.);
#8059=ORIENTED_EDGE('',*,*,#6171,.T.);
#8060=ORIENTED_EDGE('',*,*,#6174,.F.);
#8061=ORIENTED_EDGE('',*,*,#6175,.F.);
#8062=ORIENTED_EDGE('',*,*,#6176,.T.);
#8063=ORIENTED_EDGE('',*,*,#6173,.T.);
#8064=ORIENTED_EDGE('',*,*,#6176,.F.);
#8065=ORIENTED_EDGE('',*,*,#6175,.T.);
#8066=ORIENTED_EDGE('',*,*,#6167,.F.);
#8067=ORIENTED_EDGE('',*,*,#6162,.T.);
#8068=ORIENTED_EDGE('',*,*,#6163,.T.);
#8069=ORIENTED_EDGE('',*,*,#6177,.T.);
#8070=ORIENTED_EDGE('',*,*,#6170,.F.);
#8071=ORIENTED_EDGE('',*,*,#6177,.F.);
#8072=ORIENTED_EDGE('',*,*,#6178,.T.);
#8073=ORIENTED_EDGE('',*,*,#6178,.F.);
#8074=ORIENTED_EDGE('',*,*,#6179,.T.);
#8075=ORIENTED_EDGE('',*,*,#6179,.F.);
#8076=ORIENTED_EDGE('',*,*,#6180,.T.);
#8077=ORIENTED_EDGE('',*,*,#6180,.F.);
#8078=ORIENTED_EDGE('',*,*,#6181,.T.);
#8079=ORIENTED_EDGE('',*,*,#6181,.F.);
#8080=ORIENTED_EDGE('',*,*,#6182,.T.);
#8081=ORIENTED_EDGE('',*,*,#6182,.F.);
#8082=ORIENTED_EDGE('',*,*,#6183,.T.);
#8083=ORIENTED_EDGE('',*,*,#6183,.F.);
#8084=ORIENTED_EDGE('',*,*,#6184,.T.);
#8085=ORIENTED_EDGE('',*,*,#6184,.F.);
#8086=ORIENTED_EDGE('',*,*,#6185,.F.);
#8087=ORIENTED_EDGE('',*,*,#6186,.F.);
#8088=ORIENTED_EDGE('',*,*,#6187,.F.);
#8089=ORIENTED_EDGE('',*,*,#6188,.F.);
#8090=ORIENTED_EDGE('',*,*,#6187,.T.);
#8091=ORIENTED_EDGE('',*,*,#6189,.F.);
#8092=ORIENTED_EDGE('',*,*,#6190,.T.);
#8093=ORIENTED_EDGE('',*,*,#6191,.F.);
#8094=ORIENTED_EDGE('',*,*,#6192,.T.);
#8095=ORIENTED_EDGE('',*,*,#6193,.F.);
#8096=ORIENTED_EDGE('',*,*,#6194,.T.);
#8097=ORIENTED_EDGE('',*,*,#6195,.F.);
#8098=ORIENTED_EDGE('',*,*,#6194,.F.);
#8099=ORIENTED_EDGE('',*,*,#6196,.F.);
#8100=ORIENTED_EDGE('',*,*,#6197,.T.);
#8101=ORIENTED_EDGE('',*,*,#6198,.F.);
#8102=ORIENTED_EDGE('',*,*,#6199,.T.);
#8103=ORIENTED_EDGE('',*,*,#6200,.F.);
#8104=ORIENTED_EDGE('',*,*,#6201,.T.);
#8105=ORIENTED_EDGE('',*,*,#6202,.F.);
#8106=ORIENTED_EDGE('',*,*,#6203,.T.);
#8107=ORIENTED_EDGE('',*,*,#6204,.F.);
#8108=ORIENTED_EDGE('',*,*,#6186,.T.);
#8109=ORIENTED_EDGE('',*,*,#6205,.T.);
#8110=ORIENTED_EDGE('',*,*,#6206,.T.);
#8111=ORIENTED_EDGE('',*,*,#6189,.T.);
#8112=ORIENTED_EDGE('',*,*,#6207,.F.);
#8113=ORIENTED_EDGE('',*,*,#6208,.F.);
#8114=ORIENTED_EDGE('',*,*,#6190,.F.);
#8115=ORIENTED_EDGE('',*,*,#6206,.F.);
#8116=ORIENTED_EDGE('',*,*,#6208,.T.);
#8117=ORIENTED_EDGE('',*,*,#6209,.T.);
#8118=ORIENTED_EDGE('',*,*,#6210,.T.);
#8119=ORIENTED_EDGE('',*,*,#6191,.T.);
#8120=ORIENTED_EDGE('',*,*,#6211,.F.);
#8121=ORIENTED_EDGE('',*,*,#6212,.F.);
#8122=ORIENTED_EDGE('',*,*,#6192,.F.);
#8123=ORIENTED_EDGE('',*,*,#6210,.F.);
#8124=ORIENTED_EDGE('',*,*,#6212,.T.);
#8125=ORIENTED_EDGE('',*,*,#6213,.T.);
#8126=ORIENTED_EDGE('',*,*,#6214,.T.);
#8127=ORIENTED_EDGE('',*,*,#6215,.T.);
#8128=ORIENTED_EDGE('',*,*,#6196,.T.);
#8129=ORIENTED_EDGE('',*,*,#6193,.T.);
#8130=ORIENTED_EDGE('',*,*,#6216,.F.);
#8131=ORIENTED_EDGE('',*,*,#6217,.F.);
#8132=ORIENTED_EDGE('',*,*,#6197,.F.);
#8133=ORIENTED_EDGE('',*,*,#6215,.F.);
#8134=ORIENTED_EDGE('',*,*,#6217,.T.);
#8135=ORIENTED_EDGE('',*,*,#6218,.T.);
#8136=ORIENTED_EDGE('',*,*,#6219,.T.);
#8137=ORIENTED_EDGE('',*,*,#6198,.T.);
#8138=ORIENTED_EDGE('',*,*,#6220,.F.);
#8139=ORIENTED_EDGE('',*,*,#6221,.F.);
#8140=ORIENTED_EDGE('',*,*,#6199,.F.);
#8141=ORIENTED_EDGE('',*,*,#6219,.F.);
#8142=ORIENTED_EDGE('',*,*,#6221,.T.);
#8143=ORIENTED_EDGE('',*,*,#6222,.T.);
#8144=ORIENTED_EDGE('',*,*,#6223,.T.);
#8145=ORIENTED_EDGE('',*,*,#6200,.T.);
#8146=ORIENTED_EDGE('',*,*,#6201,.F.);
#8147=ORIENTED_EDGE('',*,*,#6223,.F.);
#8148=ORIENTED_EDGE('',*,*,#6224,.F.);
#8149=ORIENTED_EDGE('',*,*,#6225,.F.);
#8150=ORIENTED_EDGE('',*,*,#6226,.F.);
#8151=ORIENTED_EDGE('',*,*,#6227,.T.);
#8152=ORIENTED_EDGE('',*,*,#6213,.F.);
#8153=ORIENTED_EDGE('',*,*,#6211,.T.);
#8154=ORIENTED_EDGE('',*,*,#6209,.F.);
#8155=ORIENTED_EDGE('',*,*,#6207,.T.);
#8156=ORIENTED_EDGE('',*,*,#6205,.F.);
#8157=ORIENTED_EDGE('',*,*,#6185,.T.);
#8158=ORIENTED_EDGE('',*,*,#6228,.F.);
#8159=ORIENTED_EDGE('',*,*,#6229,.T.);
#8160=ORIENTED_EDGE('',*,*,#6230,.F.);
#8161=ORIENTED_EDGE('',*,*,#6224,.T.);
#8162=ORIENTED_EDGE('',*,*,#6222,.F.);
#8163=ORIENTED_EDGE('',*,*,#6220,.T.);
#8164=ORIENTED_EDGE('',*,*,#6218,.F.);
#8165=ORIENTED_EDGE('',*,*,#6216,.T.);
#8166=ORIENTED_EDGE('',*,*,#6214,.F.);
#8167=ORIENTED_EDGE('',*,*,#6227,.F.);
#8168=ORIENTED_EDGE('',*,*,#6188,.T.);
#8169=ORIENTED_EDGE('',*,*,#6204,.T.);
#8170=ORIENTED_EDGE('',*,*,#6231,.T.);
#8171=ORIENTED_EDGE('',*,*,#6228,.T.);
#8172=ORIENTED_EDGE('',*,*,#6203,.F.);
#8173=ORIENTED_EDGE('',*,*,#6232,.F.);
#8174=ORIENTED_EDGE('',*,*,#6229,.F.);
#8175=ORIENTED_EDGE('',*,*,#6231,.F.);
#8176=ORIENTED_EDGE('',*,*,#6195,.T.);
#8177=ORIENTED_EDGE('',*,*,#6226,.T.);
#8178=ORIENTED_EDGE('',*,*,#6225,.T.);
#8179=ORIENTED_EDGE('',*,*,#6230,.T.);
#8180=ORIENTED_EDGE('',*,*,#6232,.T.);
#8181=ORIENTED_EDGE('',*,*,#6202,.T.);
#8182=ORIENTED_EDGE('',*,*,#6233,.F.);
#8183=ORIENTED_EDGE('',*,*,#6234,.T.);
#8184=ORIENTED_EDGE('',*,*,#6235,.F.);
#8185=ORIENTED_EDGE('',*,*,#6236,.T.);
#8186=ORIENTED_EDGE('',*,*,#6233,.T.);
#8187=ORIENTED_EDGE('',*,*,#6236,.F.);
#8188=ORIENTED_EDGE('',*,*,#6235,.T.);
#8189=ORIENTED_EDGE('',*,*,#6237,.F.);
#8190=ORIENTED_EDGE('',*,*,#6237,.T.);
#8191=ORIENTED_EDGE('',*,*,#6238,.T.);
#8192=ORIENTED_EDGE('',*,*,#6234,.F.);
#8193=ORIENTED_EDGE('',*,*,#6238,.F.);
#8194=ORIENTED_EDGE('',*,*,#6239,.F.);
#8195=ORIENTED_EDGE('',*,*,#6240,.T.);
#8196=ORIENTED_EDGE('',*,*,#6241,.F.);
#8197=ORIENTED_EDGE('',*,*,#6242,.T.);
#8198=ORIENTED_EDGE('',*,*,#6239,.T.);
#8199=ORIENTED_EDGE('',*,*,#6242,.F.);
#8200=ORIENTED_EDGE('',*,*,#6241,.T.);
#8201=ORIENTED_EDGE('',*,*,#6243,.F.);
#8202=ORIENTED_EDGE('',*,*,#6243,.T.);
#8203=ORIENTED_EDGE('',*,*,#6244,.T.);
#8204=ORIENTED_EDGE('',*,*,#6240,.F.);
#8205=ORIENTED_EDGE('',*,*,#6244,.F.);
#8206=ORIENTED_EDGE('',*,*,#6245,.F.);
#8207=ORIENTED_EDGE('',*,*,#6246,.F.);
#8208=ORIENTED_EDGE('',*,*,#6247,.T.);
#8209=ORIENTED_EDGE('',*,*,#6248,.F.);
#8210=ORIENTED_EDGE('',*,*,#6249,.F.);
#8211=ORIENTED_EDGE('',*,*,#6247,.F.);
#8212=ORIENTED_EDGE('',*,*,#6248,.T.);
#8213=ORIENTED_EDGE('',*,*,#6249,.T.);
#8214=ORIENTED_EDGE('',*,*,#6250,.T.);
#8215=ORIENTED_EDGE('',*,*,#6251,.T.);
#8216=ORIENTED_EDGE('',*,*,#6250,.F.);
#8217=ORIENTED_EDGE('',*,*,#6252,.T.);
#8218=ORIENTED_EDGE('',*,*,#6253,.T.);
#8219=ORIENTED_EDGE('',*,*,#6254,.F.);
#8220=ORIENTED_EDGE('',*,*,#6253,.F.);
#8221=ORIENTED_EDGE('',*,*,#6254,.T.);
#8222=ORIENTED_EDGE('',*,*,#6255,.T.);
#8223=ORIENTED_EDGE('',*,*,#6256,.F.);
#8224=ORIENTED_EDGE('',*,*,#6255,.F.);
#8225=ORIENTED_EDGE('',*,*,#6251,.F.);
#8226=ORIENTED_EDGE('',*,*,#6256,.T.);
#8227=ORIENTED_EDGE('',*,*,#6257,.F.);
#8228=ORIENTED_EDGE('',*,*,#6258,.T.);
#8229=ORIENTED_EDGE('',*,*,#6245,.T.);
#8230=ORIENTED_EDGE('',*,*,#6246,.T.);
#8231=ORIENTED_EDGE('',*,*,#6258,.F.);
#8232=ORIENTED_EDGE('',*,*,#6257,.T.);
#8233=ORIENTED_EDGE('',*,*,#6259,.F.);
#8234=ORIENTED_EDGE('',*,*,#6259,.T.);
#8235=ORIENTED_EDGE('',*,*,#6260,.T.);
#8236=ORIENTED_EDGE('',*,*,#6252,.F.);
#8237=ORIENTED_EDGE('',*,*,#6260,.F.);
#8238=ORIENTED_EDGE('',*,*,#6261,.F.);
#8239=ORIENTED_EDGE('',*,*,#6262,.F.);
#8240=ORIENTED_EDGE('',*,*,#6263,.T.);
#8241=ORIENTED_EDGE('',*,*,#6264,.F.);
#8242=ORIENTED_EDGE('',*,*,#6265,.F.);
#8243=ORIENTED_EDGE('',*,*,#6263,.F.);
#8244=ORIENTED_EDGE('',*,*,#6266,.T.);
#8245=ORIENTED_EDGE('',*,*,#6267,.T.);
#8246=ORIENTED_EDGE('',*,*,#6264,.T.);
#8247=ORIENTED_EDGE('',*,*,#6265,.T.);
#8248=ORIENTED_EDGE('',*,*,#6267,.F.);
#8249=ORIENTED_EDGE('',*,*,#6268,.F.);
#8250=ORIENTED_EDGE('',*,*,#6269,.T.);
#8251=ORIENTED_EDGE('',*,*,#6270,.F.);
#8252=ORIENTED_EDGE('',*,*,#6271,.T.);
#8253=ORIENTED_EDGE('',*,*,#6268,.T.);
#8254=ORIENTED_EDGE('',*,*,#6271,.F.);
#8255=ORIENTED_EDGE('',*,*,#6272,.F.);
#8256=ORIENTED_EDGE('',*,*,#6273,.T.);
#8257=ORIENTED_EDGE('',*,*,#6270,.T.);
#8258=ORIENTED_EDGE('',*,*,#6273,.F.);
#8259=ORIENTED_EDGE('',*,*,#6274,.F.);
#8260=ORIENTED_EDGE('',*,*,#6275,.T.);
#8261=ORIENTED_EDGE('',*,*,#6272,.T.);
#8262=ORIENTED_EDGE('',*,*,#6275,.F.);
#8263=ORIENTED_EDGE('',*,*,#6274,.T.);
#8264=ORIENTED_EDGE('',*,*,#6266,.F.);
#8265=ORIENTED_EDGE('',*,*,#6261,.T.);
#8266=ORIENTED_EDGE('',*,*,#6262,.T.);
#8267=ORIENTED_EDGE('',*,*,#6276,.T.);
#8268=ORIENTED_EDGE('',*,*,#6269,.F.);
#8269=ORIENTED_EDGE('',*,*,#6276,.F.);
#8270=ORIENTED_EDGE('',*,*,#6277,.T.);
#8271=ORIENTED_EDGE('',*,*,#6277,.F.);
#8272=ORIENTED_EDGE('',*,*,#6278,.T.);
#8273=ORIENTED_EDGE('',*,*,#6278,.F.);
#8274=ORIENTED_EDGE('',*,*,#6279,.T.);
#8275=ORIENTED_EDGE('',*,*,#6279,.F.);
#8276=ORIENTED_EDGE('',*,*,#6280,.T.);
#8277=ORIENTED_EDGE('',*,*,#6280,.F.);
#8278=ORIENTED_EDGE('',*,*,#6281,.T.);
#8279=ORIENTED_EDGE('',*,*,#6281,.F.);
#8280=ORIENTED_EDGE('',*,*,#6282,.T.);
#8281=ORIENTED_EDGE('',*,*,#6282,.F.);
#8282=ORIENTED_EDGE('',*,*,#6283,.T.);
#8283=ORIENTED_EDGE('',*,*,#6283,.F.);
#8284=ORIENTED_EDGE('',*,*,#6284,.T.);
#8285=ORIENTED_EDGE('',*,*,#6284,.F.);
#8286=ORIENTED_EDGE('',*,*,#6285,.F.);
#8287=ORIENTED_EDGE('',*,*,#6286,.F.);
#8288=ORIENTED_EDGE('',*,*,#6287,.F.);
#8289=ORIENTED_EDGE('',*,*,#6288,.F.);
#8290=ORIENTED_EDGE('',*,*,#6287,.T.);
#8291=ORIENTED_EDGE('',*,*,#6289,.F.);
#8292=ORIENTED_EDGE('',*,*,#6290,.T.);
#8293=ORIENTED_EDGE('',*,*,#6291,.F.);
#8294=ORIENTED_EDGE('',*,*,#6292,.T.);
#8295=ORIENTED_EDGE('',*,*,#6293,.F.);
#8296=ORIENTED_EDGE('',*,*,#6294,.T.);
#8297=ORIENTED_EDGE('',*,*,#6295,.T.);
#8298=ORIENTED_EDGE('',*,*,#6296,.F.);
#8299=ORIENTED_EDGE('',*,*,#6295,.F.);
#8300=ORIENTED_EDGE('',*,*,#6297,.T.);
#8301=ORIENTED_EDGE('',*,*,#6298,.F.);
#8302=ORIENTED_EDGE('',*,*,#6299,.T.);
#8303=ORIENTED_EDGE('',*,*,#6300,.F.);
#8304=ORIENTED_EDGE('',*,*,#6301,.T.);
#8305=ORIENTED_EDGE('',*,*,#6302,.F.);
#8306=ORIENTED_EDGE('',*,*,#6303,.T.);
#8307=ORIENTED_EDGE('',*,*,#6304,.F.);
#8308=ORIENTED_EDGE('',*,*,#6305,.T.);
#8309=ORIENTED_EDGE('',*,*,#6306,.F.);
#8310=ORIENTED_EDGE('',*,*,#6286,.T.);
#8311=ORIENTED_EDGE('',*,*,#6307,.T.);
#8312=ORIENTED_EDGE('',*,*,#6308,.T.);
#8313=ORIENTED_EDGE('',*,*,#6289,.T.);
#8314=ORIENTED_EDGE('',*,*,#6309,.F.);
#8315=ORIENTED_EDGE('',*,*,#6310,.F.);
#8316=ORIENTED_EDGE('',*,*,#6290,.F.);
#8317=ORIENTED_EDGE('',*,*,#6308,.F.);
#8318=ORIENTED_EDGE('',*,*,#6310,.T.);
#8319=ORIENTED_EDGE('',*,*,#6311,.T.);
#8320=ORIENTED_EDGE('',*,*,#6312,.T.);
#8321=ORIENTED_EDGE('',*,*,#6291,.T.);
#8322=ORIENTED_EDGE('',*,*,#6313,.F.);
#8323=ORIENTED_EDGE('',*,*,#6314,.F.);
#8324=ORIENTED_EDGE('',*,*,#6292,.F.);
#8325=ORIENTED_EDGE('',*,*,#6312,.F.);
#8326=ORIENTED_EDGE('',*,*,#6314,.T.);
#8327=ORIENTED_EDGE('',*,*,#6315,.T.);
#8328=ORIENTED_EDGE('',*,*,#6316,.T.);
#8329=ORIENTED_EDGE('',*,*,#6293,.T.);
#8330=ORIENTED_EDGE('',*,*,#6317,.F.);
#8331=ORIENTED_EDGE('',*,*,#6318,.F.);
#8332=ORIENTED_EDGE('',*,*,#6297,.F.);
#8333=ORIENTED_EDGE('',*,*,#6294,.F.);
#8334=ORIENTED_EDGE('',*,*,#6316,.F.);
#8335=ORIENTED_EDGE('',*,*,#6319,.F.);
#8336=ORIENTED_EDGE('',*,*,#6318,.T.);
#8337=ORIENTED_EDGE('',*,*,#6320,.T.);
#8338=ORIENTED_EDGE('',*,*,#6321,.T.);
#8339=ORIENTED_EDGE('',*,*,#6298,.T.);
#8340=ORIENTED_EDGE('',*,*,#6322,.F.);
#8341=ORIENTED_EDGE('',*,*,#6323,.F.);
#8342=ORIENTED_EDGE('',*,*,#6299,.F.);
#8343=ORIENTED_EDGE('',*,*,#6321,.F.);
#8344=ORIENTED_EDGE('',*,*,#6323,.T.);
#8345=ORIENTED_EDGE('',*,*,#6324,.T.);
#8346=ORIENTED_EDGE('',*,*,#6325,.T.);
#8347=ORIENTED_EDGE('',*,*,#6300,.T.);
#8348=ORIENTED_EDGE('',*,*,#6326,.F.);
#8349=ORIENTED_EDGE('',*,*,#6327,.F.);
#8350=ORIENTED_EDGE('',*,*,#6301,.F.);
#8351=ORIENTED_EDGE('',*,*,#6325,.F.);
#8352=ORIENTED_EDGE('',*,*,#6327,.T.);
#8353=ORIENTED_EDGE('',*,*,#6328,.T.);
#8354=ORIENTED_EDGE('',*,*,#6329,.T.);
#8355=ORIENTED_EDGE('',*,*,#6302,.T.);
#8356=ORIENTED_EDGE('',*,*,#6303,.F.);
#8357=ORIENTED_EDGE('',*,*,#6329,.F.);
#8358=ORIENTED_EDGE('',*,*,#6330,.F.);
#8359=ORIENTED_EDGE('',*,*,#6331,.F.);
#8360=ORIENTED_EDGE('',*,*,#6332,.F.);
#8361=ORIENTED_EDGE('',*,*,#6333,.T.);
#8362=ORIENTED_EDGE('',*,*,#6319,.T.);
#8363=ORIENTED_EDGE('',*,*,#6315,.F.);
#8364=ORIENTED_EDGE('',*,*,#6313,.T.);
#8365=ORIENTED_EDGE('',*,*,#6311,.F.);
#8366=ORIENTED_EDGE('',*,*,#6309,.T.);
#8367=ORIENTED_EDGE('',*,*,#6307,.F.);
#8368=ORIENTED_EDGE('',*,*,#6285,.T.);
#8369=ORIENTED_EDGE('',*,*,#6334,.F.);
#8370=ORIENTED_EDGE('',*,*,#6335,.T.);
#8371=ORIENTED_EDGE('',*,*,#6336,.F.);
#8372=ORIENTED_EDGE('',*,*,#6330,.T.);
#8373=ORIENTED_EDGE('',*,*,#6328,.F.);
#8374=ORIENTED_EDGE('',*,*,#6326,.T.);
#8375=ORIENTED_EDGE('',*,*,#6324,.F.);
#8376=ORIENTED_EDGE('',*,*,#6322,.T.);
#8377=ORIENTED_EDGE('',*,*,#6320,.F.);
#8378=ORIENTED_EDGE('',*,*,#6317,.T.);
#8379=ORIENTED_EDGE('',*,*,#6333,.F.);
#8380=ORIENTED_EDGE('',*,*,#6288,.T.);
#8381=ORIENTED_EDGE('',*,*,#6306,.T.);
#8382=ORIENTED_EDGE('',*,*,#6337,.T.);
#8383=ORIENTED_EDGE('',*,*,#6334,.T.);
#8384=ORIENTED_EDGE('',*,*,#6305,.F.);
#8385=ORIENTED_EDGE('',*,*,#6338,.F.);
#8386=ORIENTED_EDGE('',*,*,#6335,.F.);
#8387=ORIENTED_EDGE('',*,*,#6337,.F.);
#8388=ORIENTED_EDGE('',*,*,#6296,.T.);
#8389=ORIENTED_EDGE('',*,*,#6332,.T.);
#8390=ORIENTED_EDGE('',*,*,#6331,.T.);
#8391=ORIENTED_EDGE('',*,*,#6336,.T.);
#8392=ORIENTED_EDGE('',*,*,#6338,.T.);
#8393=ORIENTED_EDGE('',*,*,#6304,.T.);
#8394=ORIENTED_EDGE('',*,*,#6339,.F.);
#8395=ORIENTED_EDGE('',*,*,#6340,.T.);
#8396=ORIENTED_EDGE('',*,*,#6341,.F.);
#8397=ORIENTED_EDGE('',*,*,#6342,.T.);
#8398=ORIENTED_EDGE('',*,*,#6339,.T.);
#8399=ORIENTED_EDGE('',*,*,#6342,.F.);
#8400=ORIENTED_EDGE('',*,*,#6341,.T.);
#8401=ORIENTED_EDGE('',*,*,#6343,.F.);
#8402=ORIENTED_EDGE('',*,*,#6343,.T.);
#8403=ORIENTED_EDGE('',*,*,#6344,.T.);
#8404=ORIENTED_EDGE('',*,*,#6340,.F.);
#8405=ORIENTED_EDGE('',*,*,#6344,.F.);
#8406=ORIENTED_EDGE('',*,*,#6345,.F.);
#8407=ORIENTED_EDGE('',*,*,#6346,.T.);
#8408=ORIENTED_EDGE('',*,*,#6347,.F.);
#8409=ORIENTED_EDGE('',*,*,#6348,.T.);
#8410=ORIENTED_EDGE('',*,*,#6345,.T.);
#8411=ORIENTED_EDGE('',*,*,#6348,.F.);
#8412=ORIENTED_EDGE('',*,*,#6347,.T.);
#8413=ORIENTED_EDGE('',*,*,#6349,.F.);
#8414=ORIENTED_EDGE('',*,*,#6349,.T.);
#8415=ORIENTED_EDGE('',*,*,#6350,.T.);
#8416=ORIENTED_EDGE('',*,*,#6346,.F.);
#8417=ORIENTED_EDGE('',*,*,#6350,.F.);
#8418=ORIENTED_EDGE('',*,*,#6351,.F.);
#8419=ORIENTED_EDGE('',*,*,#6352,.F.);
#8420=ORIENTED_EDGE('',*,*,#6353,.T.);
#8421=ORIENTED_EDGE('',*,*,#6351,.T.);
#8422=ORIENTED_EDGE('',*,*,#6353,.F.);
#8423=ORIENTED_EDGE('',*,*,#6354,.F.);
#8424=ORIENTED_EDGE('',*,*,#6355,.T.);
#8425=ORIENTED_EDGE('',*,*,#6352,.T.);
#8426=ORIENTED_EDGE('',*,*,#6355,.F.);
#8427=ORIENTED_EDGE('',*,*,#6356,.F.);
#8428=ORIENTED_EDGE('',*,*,#6357,.T.);
#8429=ORIENTED_EDGE('',*,*,#6354,.T.);
#8430=ORIENTED_EDGE('',*,*,#6357,.F.);
#8431=ORIENTED_EDGE('',*,*,#6356,.T.);
#8432=ORIENTED_EDGE('',*,*,#6358,.F.);
#8433=ORIENTED_EDGE('',*,*,#6359,.F.);
#8434=ORIENTED_EDGE('',*,*,#6360,.T.);
#8435=ORIENTED_EDGE('',*,*,#6358,.T.);
#8436=ORIENTED_EDGE('',*,*,#6360,.F.);
#8437=ORIENTED_EDGE('',*,*,#6361,.F.);
#8438=ORIENTED_EDGE('',*,*,#6362,.T.);
#8439=ORIENTED_EDGE('',*,*,#6359,.T.);
#8440=ORIENTED_EDGE('',*,*,#6362,.F.);
#8441=ORIENTED_EDGE('',*,*,#6363,.F.);
#8442=ORIENTED_EDGE('',*,*,#6364,.T.);
#8443=ORIENTED_EDGE('',*,*,#6361,.T.);
#8444=ORIENTED_EDGE('',*,*,#6364,.F.);
#8445=ORIENTED_EDGE('',*,*,#6363,.T.);
#8446=ORIENTED_EDGE('',*,*,#6365,.T.);
#8447=ORIENTED_EDGE('',*,*,#6366,.T.);
#8448=ORIENTED_EDGE('',*,*,#6367,.T.);
#8449=ORIENTED_EDGE('',*,*,#6368,.F.);
#8450=ORIENTED_EDGE('',*,*,#6369,.T.);
#8451=ORIENTED_EDGE('',*,*,#6370,.T.);
#8452=ORIENTED_EDGE('',*,*,#6371,.T.);
#8453=ORIENTED_EDGE('',*,*,#6366,.F.);
#8454=ORIENTED_EDGE('',*,*,#6372,.T.);
#8455=ORIENTED_EDGE('',*,*,#6373,.T.);
#8456=ORIENTED_EDGE('',*,*,#6374,.T.);
#8457=ORIENTED_EDGE('',*,*,#6370,.F.);
#8458=ORIENTED_EDGE('',*,*,#6375,.T.);
#8459=ORIENTED_EDGE('',*,*,#6376,.T.);
#8460=ORIENTED_EDGE('',*,*,#6377,.T.);
#8461=ORIENTED_EDGE('',*,*,#6373,.F.);
#8462=ORIENTED_EDGE('',*,*,#6378,.T.);
#8463=ORIENTED_EDGE('',*,*,#6379,.T.);
#8464=ORIENTED_EDGE('',*,*,#6380,.T.);
#8465=ORIENTED_EDGE('',*,*,#6376,.F.);
#8466=ORIENTED_EDGE('',*,*,#6381,.T.);
#8467=ORIENTED_EDGE('',*,*,#6368,.T.);
#8468=ORIENTED_EDGE('',*,*,#6382,.T.);
#8469=ORIENTED_EDGE('',*,*,#6379,.F.);
#8470=ORIENTED_EDGE('',*,*,#6381,.F.);
#8471=ORIENTED_EDGE('',*,*,#6378,.F.);
#8472=ORIENTED_EDGE('',*,*,#6375,.F.);
#8473=ORIENTED_EDGE('',*,*,#6372,.F.);
#8474=ORIENTED_EDGE('',*,*,#6369,.F.);
#8475=ORIENTED_EDGE('',*,*,#6365,.F.);
#8476=ORIENTED_EDGE('',*,*,#6382,.F.);
#8477=ORIENTED_EDGE('',*,*,#6367,.F.);
#8478=ORIENTED_EDGE('',*,*,#6371,.F.);
#8479=ORIENTED_EDGE('',*,*,#6374,.F.);
#8480=ORIENTED_EDGE('',*,*,#6377,.F.);
#8481=ORIENTED_EDGE('',*,*,#6380,.F.);
#8482=ORIENTED_EDGE('',*,*,#6383,.F.);
#8483=ORIENTED_EDGE('',*,*,#6384,.T.);
#8484=ORIENTED_EDGE('',*,*,#6385,.F.);
#8485=ORIENTED_EDGE('',*,*,#6386,.T.);
#8486=ORIENTED_EDGE('',*,*,#6387,.F.);
#8487=ORIENTED_EDGE('',*,*,#6386,.F.);
#8488=ORIENTED_EDGE('',*,*,#6388,.F.);
#8489=ORIENTED_EDGE('',*,*,#6389,.F.);
#8490=ORIENTED_EDGE('',*,*,#6390,.F.);
#8491=ORIENTED_EDGE('',*,*,#6389,.T.);
#8492=ORIENTED_EDGE('',*,*,#6391,.T.);
#8493=ORIENTED_EDGE('',*,*,#6392,.T.);
#8494=ORIENTED_EDGE('',*,*,#6388,.T.);
#8495=ORIENTED_EDGE('',*,*,#6385,.T.);
#8496=ORIENTED_EDGE('',*,*,#6393,.T.);
#8497=ORIENTED_EDGE('',*,*,#6391,.F.);
#8498=ORIENTED_EDGE('',*,*,#6394,.F.);
#8499=ORIENTED_EDGE('',*,*,#6392,.F.);
#8500=ORIENTED_EDGE('',*,*,#6393,.F.);
#8501=ORIENTED_EDGE('',*,*,#6384,.F.);
#8502=ORIENTED_EDGE('',*,*,#6395,.F.);
#8503=ORIENTED_EDGE('',*,*,#6396,.T.);
#8504=ORIENTED_EDGE('',*,*,#6397,.T.);
#8505=ORIENTED_EDGE('',*,*,#6396,.F.);
#8506=ORIENTED_EDGE('',*,*,#6390,.T.);
#8507=ORIENTED_EDGE('',*,*,#6394,.T.);
#8508=ORIENTED_EDGE('',*,*,#6383,.T.);
#8509=ORIENTED_EDGE('',*,*,#6387,.T.);
#8510=ORIENTED_EDGE('',*,*,#6395,.T.);
#8511=ORIENTED_EDGE('',*,*,#6397,.F.);
#8512=ORIENTED_EDGE('',*,*,#6398,.F.);
#8513=ORIENTED_EDGE('',*,*,#6399,.T.);
#8514=ORIENTED_EDGE('',*,*,#6400,.T.);
#8515=ORIENTED_EDGE('',*,*,#6399,.F.);
#8516=ORIENTED_EDGE('',*,*,#6401,.F.);
#8517=ORIENTED_EDGE('',*,*,#6402,.T.);
#8518=ORIENTED_EDGE('',*,*,#6403,.T.);
#8519=ORIENTED_EDGE('',*,*,#6402,.F.);
#8520=ORIENTED_EDGE('',*,*,#6401,.T.);
#8521=ORIENTED_EDGE('',*,*,#6398,.T.);
#8522=ORIENTED_EDGE('',*,*,#6403,.F.);
#8523=ORIENTED_EDGE('',*,*,#6400,.F.);
#8524=ORIENTED_EDGE('',*,*,#6404,.F.);
#8525=ORIENTED_EDGE('',*,*,#6405,.T.);
#8526=ORIENTED_EDGE('',*,*,#6406,.T.);
#8527=ORIENTED_EDGE('',*,*,#6405,.F.);
#8528=ORIENTED_EDGE('',*,*,#6407,.F.);
#8529=ORIENTED_EDGE('',*,*,#6408,.T.);
#8530=ORIENTED_EDGE('',*,*,#6409,.T.);
#8531=ORIENTED_EDGE('',*,*,#6408,.F.);
#8532=ORIENTED_EDGE('',*,*,#6407,.T.);
#8533=ORIENTED_EDGE('',*,*,#6404,.T.);
#8534=ORIENTED_EDGE('',*,*,#6409,.F.);
#8535=ORIENTED_EDGE('',*,*,#6406,.F.);
#8536=ORIENTED_EDGE('',*,*,#6410,.F.);
#8537=ORIENTED_EDGE('',*,*,#6411,.T.);
#8538=ORIENTED_EDGE('',*,*,#6412,.F.);
#8539=ORIENTED_EDGE('',*,*,#6413,.F.);
#8540=ORIENTED_EDGE('',*,*,#6414,.T.);
#8541=ORIENTED_EDGE('',*,*,#6415,.F.);
#8542=ORIENTED_EDGE('',*,*,#6416,.F.);
#8543=ORIENTED_EDGE('',*,*,#6414,.F.);
#8544=ORIENTED_EDGE('',*,*,#6417,.F.);
#8545=ORIENTED_EDGE('',*,*,#6418,.F.);
#8546=ORIENTED_EDGE('',*,*,#6411,.F.);
#8547=ORIENTED_EDGE('',*,*,#6419,.F.);
#8548=ORIENTED_EDGE('',*,*,#6417,.T.);
#8549=ORIENTED_EDGE('',*,*,#6413,.T.);
#8550=ORIENTED_EDGE('',*,*,#6420,.F.);
#8551=ORIENTED_EDGE('',*,*,#6421,.T.);
#8552=ORIENTED_EDGE('',*,*,#6422,.T.);
#8553=ORIENTED_EDGE('',*,*,#6421,.F.);
#8554=ORIENTED_EDGE('',*,*,#6418,.T.);
#8555=ORIENTED_EDGE('',*,*,#6419,.T.);
#8556=ORIENTED_EDGE('',*,*,#6412,.T.);
#8557=ORIENTED_EDGE('',*,*,#6410,.T.);
#8558=ORIENTED_EDGE('',*,*,#6423,.F.);
#8559=ORIENTED_EDGE('',*,*,#6424,.T.);
#8560=ORIENTED_EDGE('',*,*,#6425,.T.);
#8561=ORIENTED_EDGE('',*,*,#6424,.F.);
#8562=ORIENTED_EDGE('',*,*,#6415,.T.);
#8563=ORIENTED_EDGE('',*,*,#6416,.T.);
#8564=ORIENTED_EDGE('',*,*,#6423,.T.);
#8565=ORIENTED_EDGE('',*,*,#6420,.T.);
#8566=ORIENTED_EDGE('',*,*,#6425,.F.);
#8567=ORIENTED_EDGE('',*,*,#6422,.F.);
#8568=ORIENTED_EDGE('',*,*,#6426,.F.);
#8569=ORIENTED_EDGE('',*,*,#6427,.T.);
#8570=ORIENTED_EDGE('',*,*,#6428,.T.);
#8571=ORIENTED_EDGE('',*,*,#6427,.F.);
#8572=ORIENTED_EDGE('',*,*,#6429,.F.);
#8573=ORIENTED_EDGE('',*,*,#6430,.T.);
#8574=ORIENTED_EDGE('',*,*,#6431,.T.);
#8575=ORIENTED_EDGE('',*,*,#6430,.F.);
#8576=ORIENTED_EDGE('',*,*,#6429,.T.);
#8577=ORIENTED_EDGE('',*,*,#6426,.T.);
#8578=ORIENTED_EDGE('',*,*,#6431,.F.);
#8579=ORIENTED_EDGE('',*,*,#6428,.F.);
#8580=ORIENTED_EDGE('',*,*,#6432,.F.);
#8581=ORIENTED_EDGE('',*,*,#6433,.T.);
#8582=ORIENTED_EDGE('',*,*,#6434,.F.);
#8583=ORIENTED_EDGE('',*,*,#6435,.F.);
#8584=ORIENTED_EDGE('',*,*,#6436,.T.);
#8585=ORIENTED_EDGE('',*,*,#6437,.F.);
#8586=ORIENTED_EDGE('',*,*,#6438,.F.);
#8587=ORIENTED_EDGE('',*,*,#6436,.F.);
#8588=ORIENTED_EDGE('',*,*,#6439,.F.);
#8589=ORIENTED_EDGE('',*,*,#6440,.F.);
#8590=ORIENTED_EDGE('',*,*,#6433,.F.);
#8591=ORIENTED_EDGE('',*,*,#6441,.F.);
#8592=ORIENTED_EDGE('',*,*,#6439,.T.);
#8593=ORIENTED_EDGE('',*,*,#6435,.T.);
#8594=ORIENTED_EDGE('',*,*,#6442,.F.);
#8595=ORIENTED_EDGE('',*,*,#6443,.T.);
#8596=ORIENTED_EDGE('',*,*,#6444,.T.);
#8597=ORIENTED_EDGE('',*,*,#6443,.F.);
#8598=ORIENTED_EDGE('',*,*,#6440,.T.);
#8599=ORIENTED_EDGE('',*,*,#6441,.T.);
#8600=ORIENTED_EDGE('',*,*,#6434,.T.);
#8601=ORIENTED_EDGE('',*,*,#6432,.T.);
#8602=ORIENTED_EDGE('',*,*,#6445,.F.);
#8603=ORIENTED_EDGE('',*,*,#6446,.T.);
#8604=ORIENTED_EDGE('',*,*,#6447,.T.);
#8605=ORIENTED_EDGE('',*,*,#6446,.F.);
#8606=ORIENTED_EDGE('',*,*,#6437,.T.);
#8607=ORIENTED_EDGE('',*,*,#6438,.T.);
#8608=ORIENTED_EDGE('',*,*,#6445,.T.);
#8609=ORIENTED_EDGE('',*,*,#6442,.T.);
#8610=ORIENTED_EDGE('',*,*,#6447,.F.);
#8611=ORIENTED_EDGE('',*,*,#6444,.F.);
#8612=ORIENTED_EDGE('',*,*,#6448,.F.);
#8613=ORIENTED_EDGE('',*,*,#6449,.T.);
#8614=ORIENTED_EDGE('',*,*,#6450,.T.);
#8615=ORIENTED_EDGE('',*,*,#6449,.F.);
#8616=ORIENTED_EDGE('',*,*,#6451,.F.);
#8617=ORIENTED_EDGE('',*,*,#6452,.T.);
#8618=ORIENTED_EDGE('',*,*,#6453,.T.);
#8619=ORIENTED_EDGE('',*,*,#6452,.F.);
#8620=ORIENTED_EDGE('',*,*,#6451,.T.);
#8621=ORIENTED_EDGE('',*,*,#6448,.T.);
#8622=ORIENTED_EDGE('',*,*,#6453,.F.);
#8623=ORIENTED_EDGE('',*,*,#6450,.F.);
#8624=ORIENTED_EDGE('',*,*,#6454,.F.);
#8625=ORIENTED_EDGE('',*,*,#6455,.F.);
#8626=ORIENTED_EDGE('',*,*,#6456,.F.);
#8627=ORIENTED_EDGE('',*,*,#6457,.F.);
#8628=ORIENTED_EDGE('',*,*,#6458,.F.);
#8629=ORIENTED_EDGE('',*,*,#6459,.T.);
#8630=ORIENTED_EDGE('',*,*,#6460,.F.);
#8631=ORIENTED_EDGE('',*,*,#6455,.T.);
#8632=ORIENTED_EDGE('',*,*,#6461,.F.);
#8633=ORIENTED_EDGE('',*,*,#6462,.F.);
#8634=ORIENTED_EDGE('',*,*,#6463,.F.);
#8635=ORIENTED_EDGE('',*,*,#6459,.F.);
#8636=ORIENTED_EDGE('',*,*,#6464,.T.);
#8637=ORIENTED_EDGE('',*,*,#6465,.T.);
#8638=ORIENTED_EDGE('',*,*,#6466,.T.);
#8639=ORIENTED_EDGE('',*,*,#6467,.T.);
#8640=ORIENTED_EDGE('',*,*,#6468,.T.);
#8641=ORIENTED_EDGE('',*,*,#6469,.T.);
#8642=ORIENTED_EDGE('',*,*,#6470,.T.);
#8643=ORIENTED_EDGE('',*,*,#6471,.T.);
#8644=ORIENTED_EDGE('',*,*,#6472,.T.);
#8645=ORIENTED_EDGE('',*,*,#6473,.T.);
#8646=ORIENTED_EDGE('',*,*,#6474,.T.);
#8647=ORIENTED_EDGE('',*,*,#6475,.T.);
#8648=ORIENTED_EDGE('',*,*,#6476,.T.);
#8649=ORIENTED_EDGE('',*,*,#6477,.T.);
#8650=ORIENTED_EDGE('',*,*,#6478,.T.);
#8651=ORIENTED_EDGE('',*,*,#6479,.T.);
#8652=ORIENTED_EDGE('',*,*,#6480,.T.);
#8653=ORIENTED_EDGE('',*,*,#6481,.T.);
#8654=ORIENTED_EDGE('',*,*,#6482,.T.);
#8655=ORIENTED_EDGE('',*,*,#6483,.T.);
#8656=ORIENTED_EDGE('',*,*,#6484,.T.);
#8657=ORIENTED_EDGE('',*,*,#6485,.T.);
#8658=ORIENTED_EDGE('',*,*,#6486,.T.);
#8659=ORIENTED_EDGE('',*,*,#6487,.T.);
#8660=ORIENTED_EDGE('',*,*,#6488,.T.);
#8661=ORIENTED_EDGE('',*,*,#6489,.T.);
#8662=ORIENTED_EDGE('',*,*,#6490,.T.);
#8663=ORIENTED_EDGE('',*,*,#6491,.T.);
#8664=ORIENTED_EDGE('',*,*,#6492,.T.);
#8665=ORIENTED_EDGE('',*,*,#6493,.T.);
#8666=ORIENTED_EDGE('',*,*,#6494,.T.);
#8667=ORIENTED_EDGE('',*,*,#6495,.T.);
#8668=ORIENTED_EDGE('',*,*,#6496,.T.);
#8669=ORIENTED_EDGE('',*,*,#6497,.T.);
#8670=ORIENTED_EDGE('',*,*,#6498,.T.);
#8671=ORIENTED_EDGE('',*,*,#6499,.T.);
#8672=ORIENTED_EDGE('',*,*,#6500,.T.);
#8673=ORIENTED_EDGE('',*,*,#6501,.T.);
#8674=ORIENTED_EDGE('',*,*,#6502,.T.);
#8675=ORIENTED_EDGE('',*,*,#6503,.T.);
#8676=ORIENTED_EDGE('',*,*,#6504,.T.);
#8677=ORIENTED_EDGE('',*,*,#6505,.T.);
#8678=ORIENTED_EDGE('',*,*,#6506,.T.);
#8679=ORIENTED_EDGE('',*,*,#6507,.T.);
#8680=ORIENTED_EDGE('',*,*,#6508,.T.);
#8681=ORIENTED_EDGE('',*,*,#6509,.T.);
#8682=ORIENTED_EDGE('',*,*,#6510,.T.);
#8683=ORIENTED_EDGE('',*,*,#6511,.T.);
#8684=ORIENTED_EDGE('',*,*,#6512,.T.);
#8685=ORIENTED_EDGE('',*,*,#6513,.T.);
#8686=ORIENTED_EDGE('',*,*,#6514,.T.);
#8687=ORIENTED_EDGE('',*,*,#6515,.T.);
#8688=ORIENTED_EDGE('',*,*,#6516,.T.);
#8689=ORIENTED_EDGE('',*,*,#6517,.T.);
#8690=ORIENTED_EDGE('',*,*,#6518,.T.);
#8691=ORIENTED_EDGE('',*,*,#6519,.T.);
#8692=ORIENTED_EDGE('',*,*,#6520,.T.);
#8693=ORIENTED_EDGE('',*,*,#6521,.T.);
#8694=ORIENTED_EDGE('',*,*,#6522,.T.);
#8695=ORIENTED_EDGE('',*,*,#6523,.T.);
#8696=ORIENTED_EDGE('',*,*,#6524,.T.);
#8697=ORIENTED_EDGE('',*,*,#6525,.T.);
#8698=ORIENTED_EDGE('',*,*,#6526,.T.);
#8699=ORIENTED_EDGE('',*,*,#6527,.T.);
#8700=ORIENTED_EDGE('',*,*,#6528,.T.);
#8701=ORIENTED_EDGE('',*,*,#6529,.T.);
#8702=ORIENTED_EDGE('',*,*,#6530,.T.);
#8703=ORIENTED_EDGE('',*,*,#6531,.T.);
#8704=ORIENTED_EDGE('',*,*,#6532,.T.);
#8705=ORIENTED_EDGE('',*,*,#6533,.T.);
#8706=ORIENTED_EDGE('',*,*,#6534,.T.);
#8707=ORIENTED_EDGE('',*,*,#6535,.T.);
#8708=ORIENTED_EDGE('',*,*,#6536,.T.);
#8709=ORIENTED_EDGE('',*,*,#6537,.T.);
#8710=ORIENTED_EDGE('',*,*,#6538,.T.);
#8711=ORIENTED_EDGE('',*,*,#6539,.T.);
#8712=ORIENTED_EDGE('',*,*,#6540,.T.);
#8713=ORIENTED_EDGE('',*,*,#6541,.T.);
#8714=ORIENTED_EDGE('',*,*,#6542,.T.);
#8715=ORIENTED_EDGE('',*,*,#6543,.T.);
#8716=ORIENTED_EDGE('',*,*,#6456,.T.);
#8717=ORIENTED_EDGE('',*,*,#6460,.T.);
#8718=ORIENTED_EDGE('',*,*,#6463,.T.);
#8719=ORIENTED_EDGE('',*,*,#6544,.T.);
#8720=ORIENTED_EDGE('',*,*,#6457,.T.);
#8721=ORIENTED_EDGE('',*,*,#6544,.F.);
#8722=ORIENTED_EDGE('',*,*,#6462,.T.);
#8723=ORIENTED_EDGE('',*,*,#6545,.F.);
#8724=ORIENTED_EDGE('',*,*,#6546,.F.);
#8725=ORIENTED_EDGE('',*,*,#6547,.T.);
#8726=ORIENTED_EDGE('',*,*,#6548,.F.);
#8727=ORIENTED_EDGE('',*,*,#6547,.F.);
#8728=ORIENTED_EDGE('',*,*,#6546,.T.);
#8729=ORIENTED_EDGE('',*,*,#6454,.T.);
#8730=ORIENTED_EDGE('',*,*,#6545,.T.);
#8731=ORIENTED_EDGE('',*,*,#6461,.T.);
#8732=ORIENTED_EDGE('',*,*,#6458,.T.);
#8733=ORIENTED_EDGE('',*,*,#6549,.F.);
#8734=ORIENTED_EDGE('',*,*,#6550,.F.);
#8735=ORIENTED_EDGE('',*,*,#6551,.F.);
#8736=ORIENTED_EDGE('',*,*,#6541,.F.);
#8737=ORIENTED_EDGE('',*,*,#6551,.T.);
#8738=ORIENTED_EDGE('',*,*,#6552,.F.);
#8739=ORIENTED_EDGE('',*,*,#6553,.F.);
#8740=ORIENTED_EDGE('',*,*,#6542,.F.);
#8741=ORIENTED_EDGE('',*,*,#6553,.T.);
#8742=ORIENTED_EDGE('',*,*,#6554,.F.);
#8743=ORIENTED_EDGE('',*,*,#6555,.F.);
#8744=ORIENTED_EDGE('',*,*,#6543,.F.);
#8745=ORIENTED_EDGE('',*,*,#6555,.T.);
#8746=ORIENTED_EDGE('',*,*,#6556,.F.);
#8747=ORIENTED_EDGE('',*,*,#6557,.T.);
#8748=ORIENTED_EDGE('',*,*,#6464,.F.);
#8749=ORIENTED_EDGE('',*,*,#6557,.F.);
#8750=ORIENTED_EDGE('',*,*,#6558,.F.);
#8751=ORIENTED_EDGE('',*,*,#6559,.F.);
#8752=ORIENTED_EDGE('',*,*,#6465,.F.);
#8753=ORIENTED_EDGE('',*,*,#6559,.T.);
#8754=ORIENTED_EDGE('',*,*,#6560,.F.);
#8755=ORIENTED_EDGE('',*,*,#6561,.F.);
#8756=ORIENTED_EDGE('',*,*,#6466,.F.);
#8757=ORIENTED_EDGE('',*,*,#6561,.T.);
#8758=ORIENTED_EDGE('',*,*,#6562,.F.);
#8759=ORIENTED_EDGE('',*,*,#6563,.F.);
#8760=ORIENTED_EDGE('',*,*,#6467,.F.);
#8761=ORIENTED_EDGE('',*,*,#6563,.T.);
#8762=ORIENTED_EDGE('',*,*,#6564,.F.);
#8763=ORIENTED_EDGE('',*,*,#6565,.T.);
#8764=ORIENTED_EDGE('',*,*,#6468,.F.);
#8765=ORIENTED_EDGE('',*,*,#6565,.F.);
#8766=ORIENTED_EDGE('',*,*,#6566,.F.);
#8767=ORIENTED_EDGE('',*,*,#6567,.F.);
#8768=ORIENTED_EDGE('',*,*,#6469,.F.);
#8769=ORIENTED_EDGE('',*,*,#6567,.T.);
#8770=ORIENTED_EDGE('',*,*,#6568,.F.);
#8771=ORIENTED_EDGE('',*,*,#6569,.F.);
#8772=ORIENTED_EDGE('',*,*,#6470,.F.);
#8773=ORIENTED_EDGE('',*,*,#6569,.T.);
#8774=ORIENTED_EDGE('',*,*,#6570,.F.);
#8775=ORIENTED_EDGE('',*,*,#6571,.F.);
#8776=ORIENTED_EDGE('',*,*,#6471,.F.);
#8777=ORIENTED_EDGE('',*,*,#6571,.T.);
#8778=ORIENTED_EDGE('',*,*,#6572,.F.);
#8779=ORIENTED_EDGE('',*,*,#6573,.T.);
#8780=ORIENTED_EDGE('',*,*,#6472,.F.);
#8781=ORIENTED_EDGE('',*,*,#6573,.F.);
#8782=ORIENTED_EDGE('',*,*,#6574,.F.);
#8783=ORIENTED_EDGE('',*,*,#6575,.F.);
#8784=ORIENTED_EDGE('',*,*,#6473,.F.);
#8785=ORIENTED_EDGE('',*,*,#6575,.T.);
#8786=ORIENTED_EDGE('',*,*,#6576,.F.);
#8787=ORIENTED_EDGE('',*,*,#6577,.F.);
#8788=ORIENTED_EDGE('',*,*,#6474,.F.);
#8789=ORIENTED_EDGE('',*,*,#6577,.T.);
#8790=ORIENTED_EDGE('',*,*,#6578,.F.);
#8791=ORIENTED_EDGE('',*,*,#6579,.F.);
#8792=ORIENTED_EDGE('',*,*,#6475,.F.);
#8793=ORIENTED_EDGE('',*,*,#6579,.T.);
#8794=ORIENTED_EDGE('',*,*,#6580,.F.);
#8795=ORIENTED_EDGE('',*,*,#6581,.T.);
#8796=ORIENTED_EDGE('',*,*,#6476,.F.);
#8797=ORIENTED_EDGE('',*,*,#6581,.F.);
#8798=ORIENTED_EDGE('',*,*,#6582,.F.);
#8799=ORIENTED_EDGE('',*,*,#6583,.F.);
#8800=ORIENTED_EDGE('',*,*,#6477,.F.);
#8801=ORIENTED_EDGE('',*,*,#6583,.T.);
#8802=ORIENTED_EDGE('',*,*,#6584,.F.);
#8803=ORIENTED_EDGE('',*,*,#6585,.F.);
#8804=ORIENTED_EDGE('',*,*,#6478,.F.);
#8805=ORIENTED_EDGE('',*,*,#6585,.T.);
#8806=ORIENTED_EDGE('',*,*,#6586,.F.);
#8807=ORIENTED_EDGE('',*,*,#6587,.F.);
#8808=ORIENTED_EDGE('',*,*,#6479,.F.);
#8809=ORIENTED_EDGE('',*,*,#6587,.T.);
#8810=ORIENTED_EDGE('',*,*,#6588,.F.);
#8811=ORIENTED_EDGE('',*,*,#6589,.T.);
#8812=ORIENTED_EDGE('',*,*,#6480,.F.);
#8813=ORIENTED_EDGE('',*,*,#6589,.F.);
#8814=ORIENTED_EDGE('',*,*,#6590,.F.);
#8815=ORIENTED_EDGE('',*,*,#6591,.F.);
#8816=ORIENTED_EDGE('',*,*,#6481,.F.);
#8817=ORIENTED_EDGE('',*,*,#6591,.T.);
#8818=ORIENTED_EDGE('',*,*,#6592,.F.);
#8819=ORIENTED_EDGE('',*,*,#6593,.F.);
#8820=ORIENTED_EDGE('',*,*,#6482,.F.);
#8821=ORIENTED_EDGE('',*,*,#6593,.T.);
#8822=ORIENTED_EDGE('',*,*,#6594,.F.);
#8823=ORIENTED_EDGE('',*,*,#6595,.F.);
#8824=ORIENTED_EDGE('',*,*,#6483,.F.);
#8825=ORIENTED_EDGE('',*,*,#6595,.T.);
#8826=ORIENTED_EDGE('',*,*,#6596,.F.);
#8827=ORIENTED_EDGE('',*,*,#6597,.T.);
#8828=ORIENTED_EDGE('',*,*,#6484,.F.);
#8829=ORIENTED_EDGE('',*,*,#6597,.F.);
#8830=ORIENTED_EDGE('',*,*,#6598,.F.);
#8831=ORIENTED_EDGE('',*,*,#6599,.F.);
#8832=ORIENTED_EDGE('',*,*,#6485,.F.);
#8833=ORIENTED_EDGE('',*,*,#6599,.T.);
#8834=ORIENTED_EDGE('',*,*,#6600,.F.);
#8835=ORIENTED_EDGE('',*,*,#6601,.F.);
#8836=ORIENTED_EDGE('',*,*,#6486,.F.);
#8837=ORIENTED_EDGE('',*,*,#6601,.T.);
#8838=ORIENTED_EDGE('',*,*,#6602,.F.);
#8839=ORIENTED_EDGE('',*,*,#6603,.F.);
#8840=ORIENTED_EDGE('',*,*,#6487,.F.);
#8841=ORIENTED_EDGE('',*,*,#6603,.T.);
#8842=ORIENTED_EDGE('',*,*,#6604,.F.);
#8843=ORIENTED_EDGE('',*,*,#6605,.T.);
#8844=ORIENTED_EDGE('',*,*,#6488,.F.);
#8845=ORIENTED_EDGE('',*,*,#6605,.F.);
#8846=ORIENTED_EDGE('',*,*,#6606,.F.);
#8847=ORIENTED_EDGE('',*,*,#6607,.F.);
#8848=ORIENTED_EDGE('',*,*,#6489,.F.);
#8849=ORIENTED_EDGE('',*,*,#6607,.T.);
#8850=ORIENTED_EDGE('',*,*,#6608,.F.);
#8851=ORIENTED_EDGE('',*,*,#6609,.F.);
#8852=ORIENTED_EDGE('',*,*,#6490,.F.);
#8853=ORIENTED_EDGE('',*,*,#6609,.T.);
#8854=ORIENTED_EDGE('',*,*,#6610,.F.);
#8855=ORIENTED_EDGE('',*,*,#6611,.F.);
#8856=ORIENTED_EDGE('',*,*,#6491,.F.);
#8857=ORIENTED_EDGE('',*,*,#6611,.T.);
#8858=ORIENTED_EDGE('',*,*,#6612,.F.);
#8859=ORIENTED_EDGE('',*,*,#6613,.T.);
#8860=ORIENTED_EDGE('',*,*,#6492,.F.);
#8861=ORIENTED_EDGE('',*,*,#6613,.F.);
#8862=ORIENTED_EDGE('',*,*,#6614,.F.);
#8863=ORIENTED_EDGE('',*,*,#6615,.F.);
#8864=ORIENTED_EDGE('',*,*,#6493,.F.);
#8865=ORIENTED_EDGE('',*,*,#6615,.T.);
#8866=ORIENTED_EDGE('',*,*,#6616,.F.);
#8867=ORIENTED_EDGE('',*,*,#6617,.F.);
#8868=ORIENTED_EDGE('',*,*,#6494,.F.);
#8869=ORIENTED_EDGE('',*,*,#6617,.T.);
#8870=ORIENTED_EDGE('',*,*,#6618,.F.);
#8871=ORIENTED_EDGE('',*,*,#6619,.F.);
#8872=ORIENTED_EDGE('',*,*,#6495,.F.);
#8873=ORIENTED_EDGE('',*,*,#6619,.T.);
#8874=ORIENTED_EDGE('',*,*,#6620,.F.);
#8875=ORIENTED_EDGE('',*,*,#6621,.T.);
#8876=ORIENTED_EDGE('',*,*,#6496,.F.);
#8877=ORIENTED_EDGE('',*,*,#6621,.F.);
#8878=ORIENTED_EDGE('',*,*,#6622,.F.);
#8879=ORIENTED_EDGE('',*,*,#6623,.F.);
#8880=ORIENTED_EDGE('',*,*,#6497,.F.);
#8881=ORIENTED_EDGE('',*,*,#6623,.T.);
#8882=ORIENTED_EDGE('',*,*,#6624,.F.);
#8883=ORIENTED_EDGE('',*,*,#6625,.F.);
#8884=ORIENTED_EDGE('',*,*,#6498,.F.);
#8885=ORIENTED_EDGE('',*,*,#6625,.T.);
#8886=ORIENTED_EDGE('',*,*,#6626,.F.);
#8887=ORIENTED_EDGE('',*,*,#6627,.F.);
#8888=ORIENTED_EDGE('',*,*,#6499,.F.);
#8889=ORIENTED_EDGE('',*,*,#6627,.T.);
#8890=ORIENTED_EDGE('',*,*,#6628,.F.);
#8891=ORIENTED_EDGE('',*,*,#6629,.T.);
#8892=ORIENTED_EDGE('',*,*,#6500,.F.);
#8893=ORIENTED_EDGE('',*,*,#6629,.F.);
#8894=ORIENTED_EDGE('',*,*,#6630,.F.);
#8895=ORIENTED_EDGE('',*,*,#6631,.F.);
#8896=ORIENTED_EDGE('',*,*,#6501,.F.);
#8897=ORIENTED_EDGE('',*,*,#6631,.T.);
#8898=ORIENTED_EDGE('',*,*,#6632,.F.);
#8899=ORIENTED_EDGE('',*,*,#6633,.F.);
#8900=ORIENTED_EDGE('',*,*,#6502,.F.);
#8901=ORIENTED_EDGE('',*,*,#6633,.T.);
#8902=ORIENTED_EDGE('',*,*,#6634,.F.);
#8903=ORIENTED_EDGE('',*,*,#6635,.F.);
#8904=ORIENTED_EDGE('',*,*,#6503,.F.);
#8905=ORIENTED_EDGE('',*,*,#6635,.T.);
#8906=ORIENTED_EDGE('',*,*,#6636,.F.);
#8907=ORIENTED_EDGE('',*,*,#6637,.T.);
#8908=ORIENTED_EDGE('',*,*,#6504,.F.);
#8909=ORIENTED_EDGE('',*,*,#6637,.F.);
#8910=ORIENTED_EDGE('',*,*,#6638,.F.);
#8911=ORIENTED_EDGE('',*,*,#6639,.F.);
#8912=ORIENTED_EDGE('',*,*,#6505,.F.);
#8913=ORIENTED_EDGE('',*,*,#6639,.T.);
#8914=ORIENTED_EDGE('',*,*,#6640,.F.);
#8915=ORIENTED_EDGE('',*,*,#6641,.F.);
#8916=ORIENTED_EDGE('',*,*,#6506,.F.);
#8917=ORIENTED_EDGE('',*,*,#6641,.T.);
#8918=ORIENTED_EDGE('',*,*,#6642,.F.);
#8919=ORIENTED_EDGE('',*,*,#6643,.F.);
#8920=ORIENTED_EDGE('',*,*,#6507,.F.);
#8921=ORIENTED_EDGE('',*,*,#6643,.T.);
#8922=ORIENTED_EDGE('',*,*,#6644,.F.);
#8923=ORIENTED_EDGE('',*,*,#6645,.T.);
#8924=ORIENTED_EDGE('',*,*,#6508,.F.);
#8925=ORIENTED_EDGE('',*,*,#6645,.F.);
#8926=ORIENTED_EDGE('',*,*,#6646,.F.);
#8927=ORIENTED_EDGE('',*,*,#6647,.F.);
#8928=ORIENTED_EDGE('',*,*,#6509,.F.);
#8929=ORIENTED_EDGE('',*,*,#6647,.T.);
#8930=ORIENTED_EDGE('',*,*,#6648,.F.);
#8931=ORIENTED_EDGE('',*,*,#6649,.F.);
#8932=ORIENTED_EDGE('',*,*,#6510,.F.);
#8933=ORIENTED_EDGE('',*,*,#6649,.T.);
#8934=ORIENTED_EDGE('',*,*,#6650,.F.);
#8935=ORIENTED_EDGE('',*,*,#6651,.F.);
#8936=ORIENTED_EDGE('',*,*,#6511,.F.);
#8937=ORIENTED_EDGE('',*,*,#6651,.T.);
#8938=ORIENTED_EDGE('',*,*,#6652,.F.);
#8939=ORIENTED_EDGE('',*,*,#6653,.T.);
#8940=ORIENTED_EDGE('',*,*,#6512,.F.);
#8941=ORIENTED_EDGE('',*,*,#6653,.F.);
#8942=ORIENTED_EDGE('',*,*,#6654,.F.);
#8943=ORIENTED_EDGE('',*,*,#6655,.F.);
#8944=ORIENTED_EDGE('',*,*,#6513,.F.);
#8945=ORIENTED_EDGE('',*,*,#6655,.T.);
#8946=ORIENTED_EDGE('',*,*,#6656,.F.);
#8947=ORIENTED_EDGE('',*,*,#6657,.F.);
#8948=ORIENTED_EDGE('',*,*,#6514,.F.);
#8949=ORIENTED_EDGE('',*,*,#6657,.T.);
#8950=ORIENTED_EDGE('',*,*,#6658,.F.);
#8951=ORIENTED_EDGE('',*,*,#6659,.F.);
#8952=ORIENTED_EDGE('',*,*,#6515,.F.);
#8953=ORIENTED_EDGE('',*,*,#6659,.T.);
#8954=ORIENTED_EDGE('',*,*,#6660,.F.);
#8955=ORIENTED_EDGE('',*,*,#6661,.T.);
#8956=ORIENTED_EDGE('',*,*,#6516,.F.);
#8957=ORIENTED_EDGE('',*,*,#6661,.F.);
#8958=ORIENTED_EDGE('',*,*,#6662,.F.);
#8959=ORIENTED_EDGE('',*,*,#6663,.F.);
#8960=ORIENTED_EDGE('',*,*,#6517,.F.);
#8961=ORIENTED_EDGE('',*,*,#6663,.T.);
#8962=ORIENTED_EDGE('',*,*,#6664,.F.);
#8963=ORIENTED_EDGE('',*,*,#6665,.F.);
#8964=ORIENTED_EDGE('',*,*,#6518,.F.);
#8965=ORIENTED_EDGE('',*,*,#6665,.T.);
#8966=ORIENTED_EDGE('',*,*,#6666,.F.);
#8967=ORIENTED_EDGE('',*,*,#6667,.F.);
#8968=ORIENTED_EDGE('',*,*,#6519,.F.);
#8969=ORIENTED_EDGE('',*,*,#6667,.T.);
#8970=ORIENTED_EDGE('',*,*,#6668,.F.);
#8971=ORIENTED_EDGE('',*,*,#6669,.T.);
#8972=ORIENTED_EDGE('',*,*,#6520,.F.);
#8973=ORIENTED_EDGE('',*,*,#6669,.F.);
#8974=ORIENTED_EDGE('',*,*,#6670,.F.);
#8975=ORIENTED_EDGE('',*,*,#6671,.F.);
#8976=ORIENTED_EDGE('',*,*,#6521,.F.);
#8977=ORIENTED_EDGE('',*,*,#6671,.T.);
#8978=ORIENTED_EDGE('',*,*,#6672,.F.);
#8979=ORIENTED_EDGE('',*,*,#6673,.F.);
#8980=ORIENTED_EDGE('',*,*,#6522,.F.);
#8981=ORIENTED_EDGE('',*,*,#6673,.T.);
#8982=ORIENTED_EDGE('',*,*,#6674,.F.);
#8983=ORIENTED_EDGE('',*,*,#6675,.F.);
#8984=ORIENTED_EDGE('',*,*,#6523,.F.);
#8985=ORIENTED_EDGE('',*,*,#6675,.T.);
#8986=ORIENTED_EDGE('',*,*,#6676,.F.);
#8987=ORIENTED_EDGE('',*,*,#6677,.T.);
#8988=ORIENTED_EDGE('',*,*,#6524,.F.);
#8989=ORIENTED_EDGE('',*,*,#6677,.F.);
#8990=ORIENTED_EDGE('',*,*,#6678,.F.);
#8991=ORIENTED_EDGE('',*,*,#6679,.F.);
#8992=ORIENTED_EDGE('',*,*,#6525,.F.);
#8993=ORIENTED_EDGE('',*,*,#6679,.T.);
#8994=ORIENTED_EDGE('',*,*,#6680,.F.);
#8995=ORIENTED_EDGE('',*,*,#6681,.F.);
#8996=ORIENTED_EDGE('',*,*,#6526,.F.);
#8997=ORIENTED_EDGE('',*,*,#6681,.T.);
#8998=ORIENTED_EDGE('',*,*,#6682,.F.);
#8999=ORIENTED_EDGE('',*,*,#6683,.F.);
#9000=ORIENTED_EDGE('',*,*,#6527,.F.);
#9001=ORIENTED_EDGE('',*,*,#6683,.T.);
#9002=ORIENTED_EDGE('',*,*,#6684,.F.);
#9003=ORIENTED_EDGE('',*,*,#6685,.T.);
#9004=ORIENTED_EDGE('',*,*,#6528,.F.);
#9005=ORIENTED_EDGE('',*,*,#6685,.F.);
#9006=ORIENTED_EDGE('',*,*,#6686,.F.);
#9007=ORIENTED_EDGE('',*,*,#6687,.F.);
#9008=ORIENTED_EDGE('',*,*,#6529,.F.);
#9009=ORIENTED_EDGE('',*,*,#6687,.T.);
#9010=ORIENTED_EDGE('',*,*,#6688,.F.);
#9011=ORIENTED_EDGE('',*,*,#6689,.F.);
#9012=ORIENTED_EDGE('',*,*,#6530,.F.);
#9013=ORIENTED_EDGE('',*,*,#6689,.T.);
#9014=ORIENTED_EDGE('',*,*,#6690,.F.);
#9015=ORIENTED_EDGE('',*,*,#6691,.F.);
#9016=ORIENTED_EDGE('',*,*,#6531,.F.);
#9017=ORIENTED_EDGE('',*,*,#6691,.T.);
#9018=ORIENTED_EDGE('',*,*,#6692,.F.);
#9019=ORIENTED_EDGE('',*,*,#6693,.T.);
#9020=ORIENTED_EDGE('',*,*,#6532,.F.);
#9021=ORIENTED_EDGE('',*,*,#6693,.F.);
#9022=ORIENTED_EDGE('',*,*,#6694,.F.);
#9023=ORIENTED_EDGE('',*,*,#6695,.F.);
#9024=ORIENTED_EDGE('',*,*,#6533,.F.);
#9025=ORIENTED_EDGE('',*,*,#6695,.T.);
#9026=ORIENTED_EDGE('',*,*,#6696,.F.);
#9027=ORIENTED_EDGE('',*,*,#6697,.F.);
#9028=ORIENTED_EDGE('',*,*,#6534,.F.);
#9029=ORIENTED_EDGE('',*,*,#6697,.T.);
#9030=ORIENTED_EDGE('',*,*,#6698,.F.);
#9031=ORIENTED_EDGE('',*,*,#6699,.F.);
#9032=ORIENTED_EDGE('',*,*,#6535,.F.);
#9033=ORIENTED_EDGE('',*,*,#6699,.T.);
#9034=ORIENTED_EDGE('',*,*,#6700,.F.);
#9035=ORIENTED_EDGE('',*,*,#6701,.T.);
#9036=ORIENTED_EDGE('',*,*,#6536,.F.);
#9037=ORIENTED_EDGE('',*,*,#6701,.F.);
#9038=ORIENTED_EDGE('',*,*,#6702,.F.);
#9039=ORIENTED_EDGE('',*,*,#6703,.F.);
#9040=ORIENTED_EDGE('',*,*,#6537,.F.);
#9041=ORIENTED_EDGE('',*,*,#6703,.T.);
#9042=ORIENTED_EDGE('',*,*,#6704,.F.);
#9043=ORIENTED_EDGE('',*,*,#6705,.F.);
#9044=ORIENTED_EDGE('',*,*,#6538,.F.);
#9045=ORIENTED_EDGE('',*,*,#6705,.T.);
#9046=ORIENTED_EDGE('',*,*,#6706,.F.);
#9047=ORIENTED_EDGE('',*,*,#6707,.F.);
#9048=ORIENTED_EDGE('',*,*,#6539,.F.);
#9049=ORIENTED_EDGE('',*,*,#6708,.T.);
#9050=ORIENTED_EDGE('',*,*,#6706,.T.);
#9051=ORIENTED_EDGE('',*,*,#6704,.T.);
#9052=ORIENTED_EDGE('',*,*,#6702,.T.);
#9053=ORIENTED_EDGE('',*,*,#6700,.T.);
#9054=ORIENTED_EDGE('',*,*,#6698,.T.);
#9055=ORIENTED_EDGE('',*,*,#6696,.T.);
#9056=ORIENTED_EDGE('',*,*,#6694,.T.);
#9057=ORIENTED_EDGE('',*,*,#6692,.T.);
#9058=ORIENTED_EDGE('',*,*,#6690,.T.);
#9059=ORIENTED_EDGE('',*,*,#6688,.T.);
#9060=ORIENTED_EDGE('',*,*,#6686,.T.);
#9061=ORIENTED_EDGE('',*,*,#6684,.T.);
#9062=ORIENTED_EDGE('',*,*,#6682,.T.);
#9063=ORIENTED_EDGE('',*,*,#6680,.T.);
#9064=ORIENTED_EDGE('',*,*,#6678,.T.);
#9065=ORIENTED_EDGE('',*,*,#6676,.T.);
#9066=ORIENTED_EDGE('',*,*,#6674,.T.);
#9067=ORIENTED_EDGE('',*,*,#6672,.T.);
#9068=ORIENTED_EDGE('',*,*,#6670,.T.);
#9069=ORIENTED_EDGE('',*,*,#6668,.T.);
#9070=ORIENTED_EDGE('',*,*,#6666,.T.);
#9071=ORIENTED_EDGE('',*,*,#6664,.T.);
#9072=ORIENTED_EDGE('',*,*,#6662,.T.);
#9073=ORIENTED_EDGE('',*,*,#6660,.T.);
#9074=ORIENTED_EDGE('',*,*,#6658,.T.);
#9075=ORIENTED_EDGE('',*,*,#6656,.T.);
#9076=ORIENTED_EDGE('',*,*,#6654,.T.);
#9077=ORIENTED_EDGE('',*,*,#6652,.T.);
#9078=ORIENTED_EDGE('',*,*,#6650,.T.);
#9079=ORIENTED_EDGE('',*,*,#6648,.T.);
#9080=ORIENTED_EDGE('',*,*,#6646,.T.);
#9081=ORIENTED_EDGE('',*,*,#6644,.T.);
#9082=ORIENTED_EDGE('',*,*,#6642,.T.);
#9083=ORIENTED_EDGE('',*,*,#6640,.T.);
#9084=ORIENTED_EDGE('',*,*,#6638,.T.);
#9085=ORIENTED_EDGE('',*,*,#6636,.T.);
#9086=ORIENTED_EDGE('',*,*,#6634,.T.);
#9087=ORIENTED_EDGE('',*,*,#6632,.T.);
#9088=ORIENTED_EDGE('',*,*,#6630,.T.);
#9089=ORIENTED_EDGE('',*,*,#6628,.T.);
#9090=ORIENTED_EDGE('',*,*,#6626,.T.);
#9091=ORIENTED_EDGE('',*,*,#6624,.T.);
#9092=ORIENTED_EDGE('',*,*,#6622,.T.);
#9093=ORIENTED_EDGE('',*,*,#6620,.T.);
#9094=ORIENTED_EDGE('',*,*,#6618,.T.);
#9095=ORIENTED_EDGE('',*,*,#6616,.T.);
#9096=ORIENTED_EDGE('',*,*,#6614,.T.);
#9097=ORIENTED_EDGE('',*,*,#6612,.T.);
#9098=ORIENTED_EDGE('',*,*,#6610,.T.);
#9099=ORIENTED_EDGE('',*,*,#6608,.T.);
#9100=ORIENTED_EDGE('',*,*,#6606,.T.);
#9101=ORIENTED_EDGE('',*,*,#6604,.T.);
#9102=ORIENTED_EDGE('',*,*,#6602,.T.);
#9103=ORIENTED_EDGE('',*,*,#6600,.T.);
#9104=ORIENTED_EDGE('',*,*,#6598,.T.);
#9105=ORIENTED_EDGE('',*,*,#6596,.T.);
#9106=ORIENTED_EDGE('',*,*,#6594,.T.);
#9107=ORIENTED_EDGE('',*,*,#6592,.T.);
#9108=ORIENTED_EDGE('',*,*,#6590,.T.);
#9109=ORIENTED_EDGE('',*,*,#6588,.T.);
#9110=ORIENTED_EDGE('',*,*,#6586,.T.);
#9111=ORIENTED_EDGE('',*,*,#6584,.T.);
#9112=ORIENTED_EDGE('',*,*,#6582,.T.);
#9113=ORIENTED_EDGE('',*,*,#6580,.T.);
#9114=ORIENTED_EDGE('',*,*,#6578,.T.);
#9115=ORIENTED_EDGE('',*,*,#6576,.T.);
#9116=ORIENTED_EDGE('',*,*,#6574,.T.);
#9117=ORIENTED_EDGE('',*,*,#6572,.T.);
#9118=ORIENTED_EDGE('',*,*,#6570,.T.);
#9119=ORIENTED_EDGE('',*,*,#6568,.T.);
#9120=ORIENTED_EDGE('',*,*,#6566,.T.);
#9121=ORIENTED_EDGE('',*,*,#6564,.T.);
#9122=ORIENTED_EDGE('',*,*,#6562,.T.);
#9123=ORIENTED_EDGE('',*,*,#6560,.T.);
#9124=ORIENTED_EDGE('',*,*,#6558,.T.);
#9125=ORIENTED_EDGE('',*,*,#6556,.T.);
#9126=ORIENTED_EDGE('',*,*,#6554,.T.);
#9127=ORIENTED_EDGE('',*,*,#6552,.T.);
#9128=ORIENTED_EDGE('',*,*,#6550,.T.);
#9129=ORIENTED_EDGE('',*,*,#6548,.T.);
#9130=ORIENTED_EDGE('',*,*,#6549,.T.);
#9131=ORIENTED_EDGE('',*,*,#6540,.F.);
#9132=ORIENTED_EDGE('',*,*,#6707,.T.);
#9133=ORIENTED_EDGE('',*,*,#6708,.F.);
#9134=ORIENTED_EDGE('',*,*,#6709,.T.);
#9135=ORIENTED_EDGE('',*,*,#6710,.T.);
#9136=ORIENTED_EDGE('',*,*,#6711,.T.);
#9137=ORIENTED_EDGE('',*,*,#6712,.T.);
#9138=ORIENTED_EDGE('',*,*,#6713,.T.);
#9139=ORIENTED_EDGE('',*,*,#6714,.T.);
#9140=ORIENTED_EDGE('',*,*,#6709,.F.);
#9141=ORIENTED_EDGE('',*,*,#6715,.T.);
#9142=ORIENTED_EDGE('',*,*,#6716,.T.);
#9143=ORIENTED_EDGE('',*,*,#6717,.T.);
#9144=ORIENTED_EDGE('',*,*,#6713,.F.);
#9145=ORIENTED_EDGE('',*,*,#6718,.T.);
#9146=ORIENTED_EDGE('',*,*,#6711,.F.);
#9147=ORIENTED_EDGE('',*,*,#6719,.T.);
#9148=ORIENTED_EDGE('',*,*,#6716,.F.);
#9149=ORIENTED_EDGE('',*,*,#6720,.T.);
#9150=ORIENTED_EDGE('',*,*,#6715,.F.);
#9151=ORIENTED_EDGE('',*,*,#6721,.F.);
#9152=ORIENTED_EDGE('',*,*,#6722,.F.);
#9153=ORIENTED_EDGE('',*,*,#6723,.T.);
#9154=ORIENTED_EDGE('',*,*,#6712,.F.);
#9155=ORIENTED_EDGE('',*,*,#6724,.F.);
#9156=ORIENTED_EDGE('',*,*,#6725,.F.);
#9157=ORIENTED_EDGE('',*,*,#6721,.T.);
#9158=ORIENTED_EDGE('',*,*,#6710,.F.);
#9159=ORIENTED_EDGE('',*,*,#6714,.F.);
#9160=ORIENTED_EDGE('',*,*,#6717,.F.);
#9161=ORIENTED_EDGE('',*,*,#6719,.F.);
#9162=ORIENTED_EDGE('',*,*,#6726,.T.);
#9163=ORIENTED_EDGE('',*,*,#6725,.T.);
#9164=ORIENTED_EDGE('',*,*,#6727,.T.);
#9165=ORIENTED_EDGE('',*,*,#6728,.T.);
#9166=ORIENTED_EDGE('',*,*,#6729,.T.);
#9167=ORIENTED_EDGE('',*,*,#6722,.T.);
#9168=ORIENTED_EDGE('',*,*,#6726,.F.);
#9169=ORIENTED_EDGE('',*,*,#6730,.T.);
#9170=ORIENTED_EDGE('',*,*,#6731,.T.);
#9171=ORIENTED_EDGE('',*,*,#6732,.T.);
#9172=ORIENTED_EDGE('',*,*,#6729,.F.);
#9173=ORIENTED_EDGE('',*,*,#6733,.T.);
#9174=ORIENTED_EDGE('',*,*,#6727,.F.);
#9175=ORIENTED_EDGE('',*,*,#6734,.T.);
#9176=ORIENTED_EDGE('',*,*,#6731,.F.);
#9177=ORIENTED_EDGE('',*,*,#6735,.T.);
#9178=ORIENTED_EDGE('',*,*,#6720,.F.);
#9179=ORIENTED_EDGE('',*,*,#6736,.F.);
#9180=ORIENTED_EDGE('',*,*,#6734,.F.);
#9181=ORIENTED_EDGE('',*,*,#6724,.T.);
#9182=ORIENTED_EDGE('',*,*,#6728,.F.);
#9183=ORIENTED_EDGE('',*,*,#6735,.F.);
#9184=ORIENTED_EDGE('',*,*,#6733,.F.);
#9185=ORIENTED_EDGE('',*,*,#6730,.F.);
#9186=ORIENTED_EDGE('',*,*,#6718,.F.);
#9187=ORIENTED_EDGE('',*,*,#6723,.F.);
#9188=ORIENTED_EDGE('',*,*,#6732,.F.);
#9189=ORIENTED_EDGE('',*,*,#6736,.T.);
#9190=ORIENTED_EDGE('',*,*,#6737,.F.);
#9191=ORIENTED_EDGE('',*,*,#6738,.T.);
#9192=ORIENTED_EDGE('',*,*,#6739,.F.);
#9193=ORIENTED_EDGE('',*,*,#6740,.T.);
#9194=ORIENTED_EDGE('',*,*,#6741,.F.);
#9195=ORIENTED_EDGE('',*,*,#6740,.F.);
#9196=ORIENTED_EDGE('',*,*,#6742,.F.);
#9197=ORIENTED_EDGE('',*,*,#6743,.F.);
#9198=ORIENTED_EDGE('',*,*,#6744,.F.);
#9199=ORIENTED_EDGE('',*,*,#6743,.T.);
#9200=ORIENTED_EDGE('',*,*,#6745,.T.);
#9201=ORIENTED_EDGE('',*,*,#6746,.T.);
#9202=ORIENTED_EDGE('',*,*,#6742,.T.);
#9203=ORIENTED_EDGE('',*,*,#6739,.T.);
#9204=ORIENTED_EDGE('',*,*,#6747,.T.);
#9205=ORIENTED_EDGE('',*,*,#6745,.F.);
#9206=ORIENTED_EDGE('',*,*,#6748,.F.);
#9207=ORIENTED_EDGE('',*,*,#6746,.F.);
#9208=ORIENTED_EDGE('',*,*,#6747,.F.);
#9209=ORIENTED_EDGE('',*,*,#6738,.F.);
#9210=ORIENTED_EDGE('',*,*,#6749,.F.);
#9211=ORIENTED_EDGE('',*,*,#6750,.T.);
#9212=ORIENTED_EDGE('',*,*,#6751,.T.);
#9213=ORIENTED_EDGE('',*,*,#6750,.F.);
#9214=ORIENTED_EDGE('',*,*,#6744,.T.);
#9215=ORIENTED_EDGE('',*,*,#6748,.T.);
#9216=ORIENTED_EDGE('',*,*,#6737,.T.);
#9217=ORIENTED_EDGE('',*,*,#6741,.T.);
#9218=ORIENTED_EDGE('',*,*,#6749,.T.);
#9219=ORIENTED_EDGE('',*,*,#6751,.F.);
#9220=ORIENTED_EDGE('',*,*,#6752,.F.);
#9221=ORIENTED_EDGE('',*,*,#6753,.T.);
#9222=ORIENTED_EDGE('',*,*,#6754,.T.);
#9223=ORIENTED_EDGE('',*,*,#6753,.F.);
#9224=ORIENTED_EDGE('',*,*,#6755,.F.);
#9225=ORIENTED_EDGE('',*,*,#6756,.T.);
#9226=ORIENTED_EDGE('',*,*,#6757,.T.);
#9227=ORIENTED_EDGE('',*,*,#6756,.F.);
#9228=ORIENTED_EDGE('',*,*,#6755,.T.);
#9229=ORIENTED_EDGE('',*,*,#6752,.T.);
#9230=ORIENTED_EDGE('',*,*,#6757,.F.);
#9231=ORIENTED_EDGE('',*,*,#6754,.F.);
#9232=ORIENTED_EDGE('',*,*,#6758,.F.);
#9233=ORIENTED_EDGE('',*,*,#6759,.T.);
#9234=ORIENTED_EDGE('',*,*,#6760,.T.);
#9235=ORIENTED_EDGE('',*,*,#6759,.F.);
#9236=ORIENTED_EDGE('',*,*,#6761,.F.);
#9237=ORIENTED_EDGE('',*,*,#6762,.T.);
#9238=ORIENTED_EDGE('',*,*,#6763,.T.);
#9239=ORIENTED_EDGE('',*,*,#6762,.F.);
#9240=ORIENTED_EDGE('',*,*,#6761,.T.);
#9241=ORIENTED_EDGE('',*,*,#6758,.T.);
#9242=ORIENTED_EDGE('',*,*,#6763,.F.);
#9243=ORIENTED_EDGE('',*,*,#6760,.F.);
#9244=ORIENTED_EDGE('',*,*,#6764,.F.);
#9245=ORIENTED_EDGE('',*,*,#6765,.T.);
#9246=ORIENTED_EDGE('',*,*,#6766,.F.);
#9247=ORIENTED_EDGE('',*,*,#6767,.F.);
#9248=ORIENTED_EDGE('',*,*,#6768,.T.);
#9249=ORIENTED_EDGE('',*,*,#6769,.F.);
#9250=ORIENTED_EDGE('',*,*,#6770,.F.);
#9251=ORIENTED_EDGE('',*,*,#6768,.F.);
#9252=ORIENTED_EDGE('',*,*,#6771,.F.);
#9253=ORIENTED_EDGE('',*,*,#6772,.F.);
#9254=ORIENTED_EDGE('',*,*,#6765,.F.);
#9255=ORIENTED_EDGE('',*,*,#6773,.F.);
#9256=ORIENTED_EDGE('',*,*,#6771,.T.);
#9257=ORIENTED_EDGE('',*,*,#6767,.T.);
#9258=ORIENTED_EDGE('',*,*,#6774,.F.);
#9259=ORIENTED_EDGE('',*,*,#6775,.T.);
#9260=ORIENTED_EDGE('',*,*,#6776,.T.);
#9261=ORIENTED_EDGE('',*,*,#6775,.F.);
#9262=ORIENTED_EDGE('',*,*,#6772,.T.);
#9263=ORIENTED_EDGE('',*,*,#6773,.T.);
#9264=ORIENTED_EDGE('',*,*,#6766,.T.);
#9265=ORIENTED_EDGE('',*,*,#6764,.T.);
#9266=ORIENTED_EDGE('',*,*,#6777,.F.);
#9267=ORIENTED_EDGE('',*,*,#6778,.T.);
#9268=ORIENTED_EDGE('',*,*,#6779,.T.);
#9269=ORIENTED_EDGE('',*,*,#6778,.F.);
#9270=ORIENTED_EDGE('',*,*,#6769,.T.);
#9271=ORIENTED_EDGE('',*,*,#6770,.T.);
#9272=ORIENTED_EDGE('',*,*,#6777,.T.);
#9273=ORIENTED_EDGE('',*,*,#6774,.T.);
#9274=ORIENTED_EDGE('',*,*,#6779,.F.);
#9275=ORIENTED_EDGE('',*,*,#6776,.F.);
#9276=ORIENTED_EDGE('',*,*,#6780,.F.);
#9277=ORIENTED_EDGE('',*,*,#6781,.T.);
#9278=ORIENTED_EDGE('',*,*,#6782,.T.);
#9279=ORIENTED_EDGE('',*,*,#6781,.F.);
#9280=ORIENTED_EDGE('',*,*,#6783,.F.);
#9281=ORIENTED_EDGE('',*,*,#6784,.T.);
#9282=ORIENTED_EDGE('',*,*,#6785,.T.);
#9283=ORIENTED_EDGE('',*,*,#6784,.F.);
#9284=ORIENTED_EDGE('',*,*,#6783,.T.);
#9285=ORIENTED_EDGE('',*,*,#6780,.T.);
#9286=ORIENTED_EDGE('',*,*,#6785,.F.);
#9287=ORIENTED_EDGE('',*,*,#6782,.F.);
#9288=ORIENTED_EDGE('',*,*,#6786,.F.);
#9289=ORIENTED_EDGE('',*,*,#6787,.T.);
#9290=ORIENTED_EDGE('',*,*,#6788,.F.);
#9291=ORIENTED_EDGE('',*,*,#6789,.F.);
#9292=ORIENTED_EDGE('',*,*,#6790,.T.);
#9293=ORIENTED_EDGE('',*,*,#6791,.F.);
#9294=ORIENTED_EDGE('',*,*,#6792,.F.);
#9295=ORIENTED_EDGE('',*,*,#6790,.F.);
#9296=ORIENTED_EDGE('',*,*,#6793,.F.);
#9297=ORIENTED_EDGE('',*,*,#6794,.F.);
#9298=ORIENTED_EDGE('',*,*,#6787,.F.);
#9299=ORIENTED_EDGE('',*,*,#6795,.F.);
#9300=ORIENTED_EDGE('',*,*,#6793,.T.);
#9301=ORIENTED_EDGE('',*,*,#6789,.T.);
#9302=ORIENTED_EDGE('',*,*,#6796,.F.);
#9303=ORIENTED_EDGE('',*,*,#6797,.T.);
#9304=ORIENTED_EDGE('',*,*,#6798,.T.);
#9305=ORIENTED_EDGE('',*,*,#6797,.F.);
#9306=ORIENTED_EDGE('',*,*,#6794,.T.);
#9307=ORIENTED_EDGE('',*,*,#6795,.T.);
#9308=ORIENTED_EDGE('',*,*,#6788,.T.);
#9309=ORIENTED_EDGE('',*,*,#6786,.T.);
#9310=ORIENTED_EDGE('',*,*,#6799,.F.);
#9311=ORIENTED_EDGE('',*,*,#6800,.T.);
#9312=ORIENTED_EDGE('',*,*,#6801,.T.);
#9313=ORIENTED_EDGE('',*,*,#6800,.F.);
#9314=ORIENTED_EDGE('',*,*,#6791,.T.);
#9315=ORIENTED_EDGE('',*,*,#6792,.T.);
#9316=ORIENTED_EDGE('',*,*,#6799,.T.);
#9317=ORIENTED_EDGE('',*,*,#6796,.T.);
#9318=ORIENTED_EDGE('',*,*,#6801,.F.);
#9319=ORIENTED_EDGE('',*,*,#6798,.F.);
#9320=ORIENTED_EDGE('',*,*,#6802,.F.);
#9321=ORIENTED_EDGE('',*,*,#6803,.T.);
#9322=ORIENTED_EDGE('',*,*,#6804,.T.);
#9323=ORIENTED_EDGE('',*,*,#6803,.F.);
#9324=ORIENTED_EDGE('',*,*,#6805,.F.);
#9325=ORIENTED_EDGE('',*,*,#6806,.T.);
#9326=ORIENTED_EDGE('',*,*,#6807,.T.);
#9327=ORIENTED_EDGE('',*,*,#6806,.F.);
#9328=ORIENTED_EDGE('',*,*,#6805,.T.);
#9329=ORIENTED_EDGE('',*,*,#6802,.T.);
#9330=ORIENTED_EDGE('',*,*,#6807,.F.);
#9331=ORIENTED_EDGE('',*,*,#6804,.F.);
#9332=ORIENTED_EDGE('',*,*,#6808,.F.);
#9333=ORIENTED_EDGE('',*,*,#6809,.F.);
#9334=ORIENTED_EDGE('',*,*,#6810,.F.);
#9335=ORIENTED_EDGE('',*,*,#6811,.F.);
#9336=ORIENTED_EDGE('',*,*,#6812,.F.);
#9337=ORIENTED_EDGE('',*,*,#6813,.T.);
#9338=ORIENTED_EDGE('',*,*,#6814,.F.);
#9339=ORIENTED_EDGE('',*,*,#6809,.T.);
#9340=ORIENTED_EDGE('',*,*,#6815,.F.);
#9341=ORIENTED_EDGE('',*,*,#6816,.F.);
#9342=ORIENTED_EDGE('',*,*,#6817,.F.);
#9343=ORIENTED_EDGE('',*,*,#6813,.F.);
#9344=ORIENTED_EDGE('',*,*,#6818,.T.);
#9345=ORIENTED_EDGE('',*,*,#6819,.T.);
#9346=ORIENTED_EDGE('',*,*,#6820,.T.);
#9347=ORIENTED_EDGE('',*,*,#6821,.T.);
#9348=ORIENTED_EDGE('',*,*,#6822,.T.);
#9349=ORIENTED_EDGE('',*,*,#6823,.T.);
#9350=ORIENTED_EDGE('',*,*,#6824,.T.);
#9351=ORIENTED_EDGE('',*,*,#6825,.T.);
#9352=ORIENTED_EDGE('',*,*,#6826,.T.);
#9353=ORIENTED_EDGE('',*,*,#6827,.T.);
#9354=ORIENTED_EDGE('',*,*,#6828,.T.);
#9355=ORIENTED_EDGE('',*,*,#6829,.T.);
#9356=ORIENTED_EDGE('',*,*,#6830,.T.);
#9357=ORIENTED_EDGE('',*,*,#6831,.T.);
#9358=ORIENTED_EDGE('',*,*,#6832,.T.);
#9359=ORIENTED_EDGE('',*,*,#6833,.T.);
#9360=ORIENTED_EDGE('',*,*,#6834,.T.);
#9361=ORIENTED_EDGE('',*,*,#6835,.T.);
#9362=ORIENTED_EDGE('',*,*,#6836,.T.);
#9363=ORIENTED_EDGE('',*,*,#6837,.T.);
#9364=ORIENTED_EDGE('',*,*,#6838,.T.);
#9365=ORIENTED_EDGE('',*,*,#6839,.T.);
#9366=ORIENTED_EDGE('',*,*,#6840,.T.);
#9367=ORIENTED_EDGE('',*,*,#6841,.T.);
#9368=ORIENTED_EDGE('',*,*,#6842,.T.);
#9369=ORIENTED_EDGE('',*,*,#6843,.T.);
#9370=ORIENTED_EDGE('',*,*,#6844,.T.);
#9371=ORIENTED_EDGE('',*,*,#6845,.T.);
#9372=ORIENTED_EDGE('',*,*,#6846,.T.);
#9373=ORIENTED_EDGE('',*,*,#6847,.T.);
#9374=ORIENTED_EDGE('',*,*,#6848,.T.);
#9375=ORIENTED_EDGE('',*,*,#6849,.T.);
#9376=ORIENTED_EDGE('',*,*,#6850,.T.);
#9377=ORIENTED_EDGE('',*,*,#6851,.T.);
#9378=ORIENTED_EDGE('',*,*,#6852,.T.);
#9379=ORIENTED_EDGE('',*,*,#6853,.T.);
#9380=ORIENTED_EDGE('',*,*,#6854,.T.);
#9381=ORIENTED_EDGE('',*,*,#6855,.T.);
#9382=ORIENTED_EDGE('',*,*,#6856,.T.);
#9383=ORIENTED_EDGE('',*,*,#6857,.T.);
#9384=ORIENTED_EDGE('',*,*,#6858,.T.);
#9385=ORIENTED_EDGE('',*,*,#6859,.T.);
#9386=ORIENTED_EDGE('',*,*,#6860,.T.);
#9387=ORIENTED_EDGE('',*,*,#6861,.T.);
#9388=ORIENTED_EDGE('',*,*,#6862,.T.);
#9389=ORIENTED_EDGE('',*,*,#6863,.T.);
#9390=ORIENTED_EDGE('',*,*,#6864,.T.);
#9391=ORIENTED_EDGE('',*,*,#6865,.T.);
#9392=ORIENTED_EDGE('',*,*,#6866,.T.);
#9393=ORIENTED_EDGE('',*,*,#6867,.T.);
#9394=ORIENTED_EDGE('',*,*,#6868,.T.);
#9395=ORIENTED_EDGE('',*,*,#6869,.T.);
#9396=ORIENTED_EDGE('',*,*,#6870,.T.);
#9397=ORIENTED_EDGE('',*,*,#6871,.T.);
#9398=ORIENTED_EDGE('',*,*,#6872,.T.);
#9399=ORIENTED_EDGE('',*,*,#6873,.T.);
#9400=ORIENTED_EDGE('',*,*,#6874,.T.);
#9401=ORIENTED_EDGE('',*,*,#6875,.T.);
#9402=ORIENTED_EDGE('',*,*,#6876,.T.);
#9403=ORIENTED_EDGE('',*,*,#6877,.T.);
#9404=ORIENTED_EDGE('',*,*,#6878,.T.);
#9405=ORIENTED_EDGE('',*,*,#6879,.T.);
#9406=ORIENTED_EDGE('',*,*,#6880,.T.);
#9407=ORIENTED_EDGE('',*,*,#6881,.T.);
#9408=ORIENTED_EDGE('',*,*,#6882,.T.);
#9409=ORIENTED_EDGE('',*,*,#6883,.T.);
#9410=ORIENTED_EDGE('',*,*,#6884,.T.);
#9411=ORIENTED_EDGE('',*,*,#6885,.T.);
#9412=ORIENTED_EDGE('',*,*,#6886,.T.);
#9413=ORIENTED_EDGE('',*,*,#6887,.T.);
#9414=ORIENTED_EDGE('',*,*,#6888,.T.);
#9415=ORIENTED_EDGE('',*,*,#6889,.T.);
#9416=ORIENTED_EDGE('',*,*,#6890,.T.);
#9417=ORIENTED_EDGE('',*,*,#6891,.T.);
#9418=ORIENTED_EDGE('',*,*,#6892,.T.);
#9419=ORIENTED_EDGE('',*,*,#6893,.T.);
#9420=ORIENTED_EDGE('',*,*,#6894,.T.);
#9421=ORIENTED_EDGE('',*,*,#6895,.T.);
#9422=ORIENTED_EDGE('',*,*,#6896,.T.);
#9423=ORIENTED_EDGE('',*,*,#6897,.T.);
#9424=ORIENTED_EDGE('',*,*,#6898,.T.);
#9425=ORIENTED_EDGE('',*,*,#6899,.T.);
#9426=ORIENTED_EDGE('',*,*,#6900,.T.);
#9427=ORIENTED_EDGE('',*,*,#6901,.T.);
#9428=ORIENTED_EDGE('',*,*,#6902,.T.);
#9429=ORIENTED_EDGE('',*,*,#6903,.T.);
#9430=ORIENTED_EDGE('',*,*,#6904,.T.);
#9431=ORIENTED_EDGE('',*,*,#6905,.T.);
#9432=ORIENTED_EDGE('',*,*,#6906,.T.);
#9433=ORIENTED_EDGE('',*,*,#6907,.T.);
#9434=ORIENTED_EDGE('',*,*,#6908,.T.);
#9435=ORIENTED_EDGE('',*,*,#6909,.T.);
#9436=ORIENTED_EDGE('',*,*,#6910,.T.);
#9437=ORIENTED_EDGE('',*,*,#6911,.T.);
#9438=ORIENTED_EDGE('',*,*,#6912,.T.);
#9439=ORIENTED_EDGE('',*,*,#6913,.T.);
#9440=ORIENTED_EDGE('',*,*,#6914,.T.);
#9441=ORIENTED_EDGE('',*,*,#6915,.T.);
#9442=ORIENTED_EDGE('',*,*,#6916,.T.);
#9443=ORIENTED_EDGE('',*,*,#6917,.T.);
#9444=ORIENTED_EDGE('',*,*,#6918,.T.);
#9445=ORIENTED_EDGE('',*,*,#6919,.T.);
#9446=ORIENTED_EDGE('',*,*,#6920,.T.);
#9447=ORIENTED_EDGE('',*,*,#6921,.T.);
#9448=ORIENTED_EDGE('',*,*,#6922,.T.);
#9449=ORIENTED_EDGE('',*,*,#6923,.T.);
#9450=ORIENTED_EDGE('',*,*,#6924,.T.);
#9451=ORIENTED_EDGE('',*,*,#6925,.T.);
#9452=ORIENTED_EDGE('',*,*,#6926,.T.);
#9453=ORIENTED_EDGE('',*,*,#6927,.T.);
#9454=ORIENTED_EDGE('',*,*,#6928,.T.);
#9455=ORIENTED_EDGE('',*,*,#6929,.T.);
#9456=ORIENTED_EDGE('',*,*,#6930,.T.);
#9457=ORIENTED_EDGE('',*,*,#6931,.T.);
#9458=ORIENTED_EDGE('',*,*,#6932,.T.);
#9459=ORIENTED_EDGE('',*,*,#6933,.T.);
#9460=ORIENTED_EDGE('',*,*,#6934,.T.);
#9461=ORIENTED_EDGE('',*,*,#6935,.T.);
#9462=ORIENTED_EDGE('',*,*,#6936,.T.);
#9463=ORIENTED_EDGE('',*,*,#6937,.T.);
#9464=ORIENTED_EDGE('',*,*,#6938,.T.);
#9465=ORIENTED_EDGE('',*,*,#6939,.T.);
#9466=ORIENTED_EDGE('',*,*,#6940,.T.);
#9467=ORIENTED_EDGE('',*,*,#6941,.T.);
#9468=ORIENTED_EDGE('',*,*,#6942,.T.);
#9469=ORIENTED_EDGE('',*,*,#6943,.T.);
#9470=ORIENTED_EDGE('',*,*,#6944,.T.);
#9471=ORIENTED_EDGE('',*,*,#6945,.T.);
#9472=ORIENTED_EDGE('',*,*,#6946,.T.);
#9473=ORIENTED_EDGE('',*,*,#6947,.T.);
#9474=ORIENTED_EDGE('',*,*,#6948,.T.);
#9475=ORIENTED_EDGE('',*,*,#6949,.T.);
#9476=ORIENTED_EDGE('',*,*,#6950,.T.);
#9477=ORIENTED_EDGE('',*,*,#6951,.T.);
#9478=ORIENTED_EDGE('',*,*,#6952,.T.);
#9479=ORIENTED_EDGE('',*,*,#6953,.T.);
#9480=ORIENTED_EDGE('',*,*,#6954,.T.);
#9481=ORIENTED_EDGE('',*,*,#6955,.T.);
#9482=ORIENTED_EDGE('',*,*,#6956,.T.);
#9483=ORIENTED_EDGE('',*,*,#6957,.T.);
#9484=ORIENTED_EDGE('',*,*,#6958,.T.);
#9485=ORIENTED_EDGE('',*,*,#6959,.T.);
#9486=ORIENTED_EDGE('',*,*,#6960,.T.);
#9487=ORIENTED_EDGE('',*,*,#6961,.T.);
#9488=ORIENTED_EDGE('',*,*,#6962,.T.);
#9489=ORIENTED_EDGE('',*,*,#6963,.T.);
#9490=ORIENTED_EDGE('',*,*,#6964,.T.);
#9491=ORIENTED_EDGE('',*,*,#6965,.T.);
#9492=ORIENTED_EDGE('',*,*,#6966,.T.);
#9493=ORIENTED_EDGE('',*,*,#6967,.T.);
#9494=ORIENTED_EDGE('',*,*,#6968,.T.);
#9495=ORIENTED_EDGE('',*,*,#6969,.T.);
#9496=ORIENTED_EDGE('',*,*,#6970,.T.);
#9497=ORIENTED_EDGE('',*,*,#6971,.T.);
#9498=ORIENTED_EDGE('',*,*,#6972,.T.);
#9499=ORIENTED_EDGE('',*,*,#6973,.T.);
#9500=ORIENTED_EDGE('',*,*,#6974,.T.);
#9501=ORIENTED_EDGE('',*,*,#6975,.T.);
#9502=ORIENTED_EDGE('',*,*,#6976,.T.);
#9503=ORIENTED_EDGE('',*,*,#6977,.T.);
#9504=ORIENTED_EDGE('',*,*,#6810,.T.);
#9505=ORIENTED_EDGE('',*,*,#6814,.T.);
#9506=ORIENTED_EDGE('',*,*,#6817,.T.);
#9507=ORIENTED_EDGE('',*,*,#6978,.T.);
#9508=ORIENTED_EDGE('',*,*,#6811,.T.);
#9509=ORIENTED_EDGE('',*,*,#6978,.F.);
#9510=ORIENTED_EDGE('',*,*,#6816,.T.);
#9511=ORIENTED_EDGE('',*,*,#6979,.F.);
#9512=ORIENTED_EDGE('',*,*,#6980,.F.);
#9513=ORIENTED_EDGE('',*,*,#6981,.T.);
#9514=ORIENTED_EDGE('',*,*,#6982,.F.);
#9515=ORIENTED_EDGE('',*,*,#6981,.F.);
#9516=ORIENTED_EDGE('',*,*,#6980,.T.);
#9517=ORIENTED_EDGE('',*,*,#6808,.T.);
#9518=ORIENTED_EDGE('',*,*,#6979,.T.);
#9519=ORIENTED_EDGE('',*,*,#6815,.T.);
#9520=ORIENTED_EDGE('',*,*,#6812,.T.);
#9521=ORIENTED_EDGE('',*,*,#6983,.F.);
#9522=ORIENTED_EDGE('',*,*,#6984,.F.);
#9523=ORIENTED_EDGE('',*,*,#6985,.F.);
#9524=ORIENTED_EDGE('',*,*,#6975,.F.);
#9525=ORIENTED_EDGE('',*,*,#6986,.F.);
#9526=ORIENTED_EDGE('',*,*,#6977,.F.);
#9527=ORIENTED_EDGE('',*,*,#6987,.T.);
#9528=ORIENTED_EDGE('',*,*,#6988,.F.);
#9529=ORIENTED_EDGE('',*,*,#6985,.T.);
#9530=ORIENTED_EDGE('',*,*,#6989,.F.);
#9531=ORIENTED_EDGE('',*,*,#6987,.F.);
#9532=ORIENTED_EDGE('',*,*,#6976,.F.);
#9533=ORIENTED_EDGE('',*,*,#6986,.T.);
#9534=ORIENTED_EDGE('',*,*,#6990,.F.);
#9535=ORIENTED_EDGE('',*,*,#6991,.T.);
#9536=ORIENTED_EDGE('',*,*,#6818,.F.);
#9537=ORIENTED_EDGE('',*,*,#6991,.F.);
#9538=ORIENTED_EDGE('',*,*,#6992,.F.);
#9539=ORIENTED_EDGE('',*,*,#6993,.F.);
#9540=ORIENTED_EDGE('',*,*,#6819,.F.);
#9541=ORIENTED_EDGE('',*,*,#6994,.F.);
#9542=ORIENTED_EDGE('',*,*,#6821,.F.);
#9543=ORIENTED_EDGE('',*,*,#6995,.T.);
#9544=ORIENTED_EDGE('',*,*,#6996,.F.);
#9545=ORIENTED_EDGE('',*,*,#6993,.T.);
#9546=ORIENTED_EDGE('',*,*,#6997,.F.);
#9547=ORIENTED_EDGE('',*,*,#6995,.F.);
#9548=ORIENTED_EDGE('',*,*,#6820,.F.);
#9549=ORIENTED_EDGE('',*,*,#6994,.T.);
#9550=ORIENTED_EDGE('',*,*,#6998,.F.);
#9551=ORIENTED_EDGE('',*,*,#6999,.T.);
#9552=ORIENTED_EDGE('',*,*,#6822,.F.);
#9553=ORIENTED_EDGE('',*,*,#6999,.F.);
#9554=ORIENTED_EDGE('',*,*,#7000,.F.);
#9555=ORIENTED_EDGE('',*,*,#7001,.F.);
#9556=ORIENTED_EDGE('',*,*,#6823,.F.);
#9557=ORIENTED_EDGE('',*,*,#7002,.F.);
#9558=ORIENTED_EDGE('',*,*,#6825,.F.);
#9559=ORIENTED_EDGE('',*,*,#7003,.T.);
#9560=ORIENTED_EDGE('',*,*,#7004,.F.);
#9561=ORIENTED_EDGE('',*,*,#7001,.T.);
#9562=ORIENTED_EDGE('',*,*,#7005,.F.);
#9563=ORIENTED_EDGE('',*,*,#7003,.F.);
#9564=ORIENTED_EDGE('',*,*,#6824,.F.);
#9565=ORIENTED_EDGE('',*,*,#7002,.T.);
#9566=ORIENTED_EDGE('',*,*,#7006,.F.);
#9567=ORIENTED_EDGE('',*,*,#7007,.T.);
#9568=ORIENTED_EDGE('',*,*,#6826,.F.);
#9569=ORIENTED_EDGE('',*,*,#7007,.F.);
#9570=ORIENTED_EDGE('',*,*,#7008,.F.);
#9571=ORIENTED_EDGE('',*,*,#7009,.F.);
#9572=ORIENTED_EDGE('',*,*,#6827,.F.);
#9573=ORIENTED_EDGE('',*,*,#7010,.F.);
#9574=ORIENTED_EDGE('',*,*,#6829,.F.);
#9575=ORIENTED_EDGE('',*,*,#7011,.T.);
#9576=ORIENTED_EDGE('',*,*,#7012,.F.);
#9577=ORIENTED_EDGE('',*,*,#7009,.T.);
#9578=ORIENTED_EDGE('',*,*,#7013,.F.);
#9579=ORIENTED_EDGE('',*,*,#7011,.F.);
#9580=ORIENTED_EDGE('',*,*,#6828,.F.);
#9581=ORIENTED_EDGE('',*,*,#7010,.T.);
#9582=ORIENTED_EDGE('',*,*,#7014,.F.);
#9583=ORIENTED_EDGE('',*,*,#7015,.T.);
#9584=ORIENTED_EDGE('',*,*,#6830,.F.);
#9585=ORIENTED_EDGE('',*,*,#7015,.F.);
#9586=ORIENTED_EDGE('',*,*,#7016,.F.);
#9587=ORIENTED_EDGE('',*,*,#7017,.F.);
#9588=ORIENTED_EDGE('',*,*,#6831,.F.);
#9589=ORIENTED_EDGE('',*,*,#7018,.F.);
#9590=ORIENTED_EDGE('',*,*,#6833,.F.);
#9591=ORIENTED_EDGE('',*,*,#7019,.T.);
#9592=ORIENTED_EDGE('',*,*,#7020,.F.);
#9593=ORIENTED_EDGE('',*,*,#7017,.T.);
#9594=ORIENTED_EDGE('',*,*,#7021,.F.);
#9595=ORIENTED_EDGE('',*,*,#7019,.F.);
#9596=ORIENTED_EDGE('',*,*,#6832,.F.);
#9597=ORIENTED_EDGE('',*,*,#7018,.T.);
#9598=ORIENTED_EDGE('',*,*,#7022,.F.);
#9599=ORIENTED_EDGE('',*,*,#7023,.T.);
#9600=ORIENTED_EDGE('',*,*,#6834,.F.);
#9601=ORIENTED_EDGE('',*,*,#7023,.F.);
#9602=ORIENTED_EDGE('',*,*,#7024,.F.);
#9603=ORIENTED_EDGE('',*,*,#7025,.F.);
#9604=ORIENTED_EDGE('',*,*,#6835,.F.);
#9605=ORIENTED_EDGE('',*,*,#7026,.F.);
#9606=ORIENTED_EDGE('',*,*,#6837,.F.);
#9607=ORIENTED_EDGE('',*,*,#7027,.T.);
#9608=ORIENTED_EDGE('',*,*,#7028,.F.);
#9609=ORIENTED_EDGE('',*,*,#7025,.T.);
#9610=ORIENTED_EDGE('',*,*,#7029,.F.);
#9611=ORIENTED_EDGE('',*,*,#7027,.F.);
#9612=ORIENTED_EDGE('',*,*,#6836,.F.);
#9613=ORIENTED_EDGE('',*,*,#7026,.T.);
#9614=ORIENTED_EDGE('',*,*,#7030,.F.);
#9615=ORIENTED_EDGE('',*,*,#7031,.T.);
#9616=ORIENTED_EDGE('',*,*,#6838,.F.);
#9617=ORIENTED_EDGE('',*,*,#7031,.F.);
#9618=ORIENTED_EDGE('',*,*,#7032,.F.);
#9619=ORIENTED_EDGE('',*,*,#7033,.F.);
#9620=ORIENTED_EDGE('',*,*,#6839,.F.);
#9621=ORIENTED_EDGE('',*,*,#7034,.F.);
#9622=ORIENTED_EDGE('',*,*,#6841,.F.);
#9623=ORIENTED_EDGE('',*,*,#7035,.T.);
#9624=ORIENTED_EDGE('',*,*,#7036,.F.);
#9625=ORIENTED_EDGE('',*,*,#7033,.T.);
#9626=ORIENTED_EDGE('',*,*,#7037,.F.);
#9627=ORIENTED_EDGE('',*,*,#7035,.F.);
#9628=ORIENTED_EDGE('',*,*,#6840,.F.);
#9629=ORIENTED_EDGE('',*,*,#7034,.T.);
#9630=ORIENTED_EDGE('',*,*,#7038,.F.);
#9631=ORIENTED_EDGE('',*,*,#7039,.T.);
#9632=ORIENTED_EDGE('',*,*,#6842,.F.);
#9633=ORIENTED_EDGE('',*,*,#7039,.F.);
#9634=ORIENTED_EDGE('',*,*,#7040,.F.);
#9635=ORIENTED_EDGE('',*,*,#7041,.F.);
#9636=ORIENTED_EDGE('',*,*,#6843,.F.);
#9637=ORIENTED_EDGE('',*,*,#7042,.F.);
#9638=ORIENTED_EDGE('',*,*,#6845,.F.);
#9639=ORIENTED_EDGE('',*,*,#7043,.T.);
#9640=ORIENTED_EDGE('',*,*,#7044,.F.);
#9641=ORIENTED_EDGE('',*,*,#7041,.T.);
#9642=ORIENTED_EDGE('',*,*,#7045,.F.);
#9643=ORIENTED_EDGE('',*,*,#7043,.F.);
#9644=ORIENTED_EDGE('',*,*,#6844,.F.);
#9645=ORIENTED_EDGE('',*,*,#7042,.T.);
#9646=ORIENTED_EDGE('',*,*,#7046,.F.);
#9647=ORIENTED_EDGE('',*,*,#7047,.T.);
#9648=ORIENTED_EDGE('',*,*,#6846,.F.);
#9649=ORIENTED_EDGE('',*,*,#7047,.F.);
#9650=ORIENTED_EDGE('',*,*,#7048,.F.);
#9651=ORIENTED_EDGE('',*,*,#7049,.F.);
#9652=ORIENTED_EDGE('',*,*,#6847,.F.);
#9653=ORIENTED_EDGE('',*,*,#7050,.F.);
#9654=ORIENTED_EDGE('',*,*,#6849,.F.);
#9655=ORIENTED_EDGE('',*,*,#7051,.T.);
#9656=ORIENTED_EDGE('',*,*,#7052,.F.);
#9657=ORIENTED_EDGE('',*,*,#7049,.T.);
#9658=ORIENTED_EDGE('',*,*,#7053,.F.);
#9659=ORIENTED_EDGE('',*,*,#7051,.F.);
#9660=ORIENTED_EDGE('',*,*,#6848,.F.);
#9661=ORIENTED_EDGE('',*,*,#7050,.T.);
#9662=ORIENTED_EDGE('',*,*,#7054,.F.);
#9663=ORIENTED_EDGE('',*,*,#7055,.T.);
#9664=ORIENTED_EDGE('',*,*,#6850,.F.);
#9665=ORIENTED_EDGE('',*,*,#7055,.F.);
#9666=ORIENTED_EDGE('',*,*,#7056,.F.);
#9667=ORIENTED_EDGE('',*,*,#7057,.F.);
#9668=ORIENTED_EDGE('',*,*,#6851,.F.);
#9669=ORIENTED_EDGE('',*,*,#7058,.F.);
#9670=ORIENTED_EDGE('',*,*,#6853,.F.);
#9671=ORIENTED_EDGE('',*,*,#7059,.T.);
#9672=ORIENTED_EDGE('',*,*,#7060,.F.);
#9673=ORIENTED_EDGE('',*,*,#7057,.T.);
#9674=ORIENTED_EDGE('',*,*,#7061,.F.);
#9675=ORIENTED_EDGE('',*,*,#7059,.F.);
#9676=ORIENTED_EDGE('',*,*,#6852,.F.);
#9677=ORIENTED_EDGE('',*,*,#7058,.T.);
#9678=ORIENTED_EDGE('',*,*,#7062,.F.);
#9679=ORIENTED_EDGE('',*,*,#7063,.T.);
#9680=ORIENTED_EDGE('',*,*,#6854,.F.);
#9681=ORIENTED_EDGE('',*,*,#7063,.F.);
#9682=ORIENTED_EDGE('',*,*,#7064,.F.);
#9683=ORIENTED_EDGE('',*,*,#7065,.F.);
#9684=ORIENTED_EDGE('',*,*,#6855,.F.);
#9685=ORIENTED_EDGE('',*,*,#7066,.F.);
#9686=ORIENTED_EDGE('',*,*,#6857,.F.);
#9687=ORIENTED_EDGE('',*,*,#7067,.T.);
#9688=ORIENTED_EDGE('',*,*,#7068,.F.);
#9689=ORIENTED_EDGE('',*,*,#7065,.T.);
#9690=ORIENTED_EDGE('',*,*,#7069,.F.);
#9691=ORIENTED_EDGE('',*,*,#7067,.F.);
#9692=ORIENTED_EDGE('',*,*,#6856,.F.);
#9693=ORIENTED_EDGE('',*,*,#7066,.T.);
#9694=ORIENTED_EDGE('',*,*,#7070,.F.);
#9695=ORIENTED_EDGE('',*,*,#7071,.T.);
#9696=ORIENTED_EDGE('',*,*,#6858,.F.);
#9697=ORIENTED_EDGE('',*,*,#7071,.F.);
#9698=ORIENTED_EDGE('',*,*,#7072,.F.);
#9699=ORIENTED_EDGE('',*,*,#7073,.F.);
#9700=ORIENTED_EDGE('',*,*,#6859,.F.);
#9701=ORIENTED_EDGE('',*,*,#7074,.F.);
#9702=ORIENTED_EDGE('',*,*,#6861,.F.);
#9703=ORIENTED_EDGE('',*,*,#7075,.T.);
#9704=ORIENTED_EDGE('',*,*,#7076,.F.);
#9705=ORIENTED_EDGE('',*,*,#7073,.T.);
#9706=ORIENTED_EDGE('',*,*,#7077,.F.);
#9707=ORIENTED_EDGE('',*,*,#7075,.F.);
#9708=ORIENTED_EDGE('',*,*,#6860,.F.);
#9709=ORIENTED_EDGE('',*,*,#7074,.T.);
#9710=ORIENTED_EDGE('',*,*,#7078,.F.);
#9711=ORIENTED_EDGE('',*,*,#7079,.T.);
#9712=ORIENTED_EDGE('',*,*,#6862,.F.);
#9713=ORIENTED_EDGE('',*,*,#7079,.F.);
#9714=ORIENTED_EDGE('',*,*,#7080,.F.);
#9715=ORIENTED_EDGE('',*,*,#7081,.F.);
#9716=ORIENTED_EDGE('',*,*,#6863,.F.);
#9717=ORIENTED_EDGE('',*,*,#7082,.F.);
#9718=ORIENTED_EDGE('',*,*,#6865,.F.);
#9719=ORIENTED_EDGE('',*,*,#7083,.T.);
#9720=ORIENTED_EDGE('',*,*,#7084,.F.);
#9721=ORIENTED_EDGE('',*,*,#7081,.T.);
#9722=ORIENTED_EDGE('',*,*,#7085,.F.);
#9723=ORIENTED_EDGE('',*,*,#7083,.F.);
#9724=ORIENTED_EDGE('',*,*,#6864,.F.);
#9725=ORIENTED_EDGE('',*,*,#7082,.T.);
#9726=ORIENTED_EDGE('',*,*,#7086,.F.);
#9727=ORIENTED_EDGE('',*,*,#7087,.T.);
#9728=ORIENTED_EDGE('',*,*,#6866,.F.);
#9729=ORIENTED_EDGE('',*,*,#7087,.F.);
#9730=ORIENTED_EDGE('',*,*,#7088,.F.);
#9731=ORIENTED_EDGE('',*,*,#7089,.F.);
#9732=ORIENTED_EDGE('',*,*,#6867,.F.);
#9733=ORIENTED_EDGE('',*,*,#7090,.F.);
#9734=ORIENTED_EDGE('',*,*,#6869,.F.);
#9735=ORIENTED_EDGE('',*,*,#7091,.T.);
#9736=ORIENTED_EDGE('',*,*,#7092,.F.);
#9737=ORIENTED_EDGE('',*,*,#7089,.T.);
#9738=ORIENTED_EDGE('',*,*,#7093,.F.);
#9739=ORIENTED_EDGE('',*,*,#7091,.F.);
#9740=ORIENTED_EDGE('',*,*,#6868,.F.);
#9741=ORIENTED_EDGE('',*,*,#7090,.T.);
#9742=ORIENTED_EDGE('',*,*,#7094,.F.);
#9743=ORIENTED_EDGE('',*,*,#7095,.T.);
#9744=ORIENTED_EDGE('',*,*,#6870,.F.);
#9745=ORIENTED_EDGE('',*,*,#7095,.F.);
#9746=ORIENTED_EDGE('',*,*,#7096,.F.);
#9747=ORIENTED_EDGE('',*,*,#7097,.F.);
#9748=ORIENTED_EDGE('',*,*,#6871,.F.);
#9749=ORIENTED_EDGE('',*,*,#7098,.F.);
#9750=ORIENTED_EDGE('',*,*,#6873,.F.);
#9751=ORIENTED_EDGE('',*,*,#7099,.T.);
#9752=ORIENTED_EDGE('',*,*,#7100,.F.);
#9753=ORIENTED_EDGE('',*,*,#7097,.T.);
#9754=ORIENTED_EDGE('',*,*,#7101,.F.);
#9755=ORIENTED_EDGE('',*,*,#7099,.F.);
#9756=ORIENTED_EDGE('',*,*,#6872,.F.);
#9757=ORIENTED_EDGE('',*,*,#7098,.T.);
#9758=ORIENTED_EDGE('',*,*,#7102,.F.);
#9759=ORIENTED_EDGE('',*,*,#7103,.T.);
#9760=ORIENTED_EDGE('',*,*,#6874,.F.);
#9761=ORIENTED_EDGE('',*,*,#7103,.F.);
#9762=ORIENTED_EDGE('',*,*,#7104,.F.);
#9763=ORIENTED_EDGE('',*,*,#7105,.F.);
#9764=ORIENTED_EDGE('',*,*,#6875,.F.);
#9765=ORIENTED_EDGE('',*,*,#7106,.F.);
#9766=ORIENTED_EDGE('',*,*,#6877,.F.);
#9767=ORIENTED_EDGE('',*,*,#7107,.T.);
#9768=ORIENTED_EDGE('',*,*,#7108,.F.);
#9769=ORIENTED_EDGE('',*,*,#7105,.T.);
#9770=ORIENTED_EDGE('',*,*,#7109,.F.);
#9771=ORIENTED_EDGE('',*,*,#7107,.F.);
#9772=ORIENTED_EDGE('',*,*,#6876,.F.);
#9773=ORIENTED_EDGE('',*,*,#7106,.T.);
#9774=ORIENTED_EDGE('',*,*,#7110,.F.);
#9775=ORIENTED_EDGE('',*,*,#7111,.T.);
#9776=ORIENTED_EDGE('',*,*,#6878,.F.);
#9777=ORIENTED_EDGE('',*,*,#7111,.F.);
#9778=ORIENTED_EDGE('',*,*,#7112,.F.);
#9779=ORIENTED_EDGE('',*,*,#7113,.F.);
#9780=ORIENTED_EDGE('',*,*,#6879,.F.);
#9781=ORIENTED_EDGE('',*,*,#7114,.F.);
#9782=ORIENTED_EDGE('',*,*,#6881,.F.);
#9783=ORIENTED_EDGE('',*,*,#7115,.T.);
#9784=ORIENTED_EDGE('',*,*,#7116,.F.);
#9785=ORIENTED_EDGE('',*,*,#7113,.T.);
#9786=ORIENTED_EDGE('',*,*,#7117,.F.);
#9787=ORIENTED_EDGE('',*,*,#7115,.F.);
#9788=ORIENTED_EDGE('',*,*,#6880,.F.);
#9789=ORIENTED_EDGE('',*,*,#7114,.T.);
#9790=ORIENTED_EDGE('',*,*,#7118,.F.);
#9791=ORIENTED_EDGE('',*,*,#7119,.T.);
#9792=ORIENTED_EDGE('',*,*,#6882,.F.);
#9793=ORIENTED_EDGE('',*,*,#7119,.F.);
#9794=ORIENTED_EDGE('',*,*,#7120,.F.);
#9795=ORIENTED_EDGE('',*,*,#7121,.F.);
#9796=ORIENTED_EDGE('',*,*,#6883,.F.);
#9797=ORIENTED_EDGE('',*,*,#7122,.F.);
#9798=ORIENTED_EDGE('',*,*,#6885,.F.);
#9799=ORIENTED_EDGE('',*,*,#7123,.T.);
#9800=ORIENTED_EDGE('',*,*,#7124,.F.);
#9801=ORIENTED_EDGE('',*,*,#7121,.T.);
#9802=ORIENTED_EDGE('',*,*,#7125,.F.);
#9803=ORIENTED_EDGE('',*,*,#7123,.F.);
#9804=ORIENTED_EDGE('',*,*,#6884,.F.);
#9805=ORIENTED_EDGE('',*,*,#7122,.T.);
#9806=ORIENTED_EDGE('',*,*,#7126,.F.);
#9807=ORIENTED_EDGE('',*,*,#7127,.T.);
#9808=ORIENTED_EDGE('',*,*,#6886,.F.);
#9809=ORIENTED_EDGE('',*,*,#7127,.F.);
#9810=ORIENTED_EDGE('',*,*,#7128,.F.);
#9811=ORIENTED_EDGE('',*,*,#7129,.F.);
#9812=ORIENTED_EDGE('',*,*,#6887,.F.);
#9813=ORIENTED_EDGE('',*,*,#7130,.F.);
#9814=ORIENTED_EDGE('',*,*,#6889,.F.);
#9815=ORIENTED_EDGE('',*,*,#7131,.T.);
#9816=ORIENTED_EDGE('',*,*,#7132,.F.);
#9817=ORIENTED_EDGE('',*,*,#7129,.T.);
#9818=ORIENTED_EDGE('',*,*,#7133,.F.);
#9819=ORIENTED_EDGE('',*,*,#7131,.F.);
#9820=ORIENTED_EDGE('',*,*,#6888,.F.);
#9821=ORIENTED_EDGE('',*,*,#7130,.T.);
#9822=ORIENTED_EDGE('',*,*,#7134,.F.);
#9823=ORIENTED_EDGE('',*,*,#7135,.T.);
#9824=ORIENTED_EDGE('',*,*,#6890,.F.);
#9825=ORIENTED_EDGE('',*,*,#7135,.F.);
#9826=ORIENTED_EDGE('',*,*,#7136,.F.);
#9827=ORIENTED_EDGE('',*,*,#7137,.F.);
#9828=ORIENTED_EDGE('',*,*,#6891,.F.);
#9829=ORIENTED_EDGE('',*,*,#7138,.F.);
#9830=ORIENTED_EDGE('',*,*,#6893,.F.);
#9831=ORIENTED_EDGE('',*,*,#7139,.T.);
#9832=ORIENTED_EDGE('',*,*,#7140,.F.);
#9833=ORIENTED_EDGE('',*,*,#7137,.T.);
#9834=ORIENTED_EDGE('',*,*,#7141,.F.);
#9835=ORIENTED_EDGE('',*,*,#7139,.F.);
#9836=ORIENTED_EDGE('',*,*,#6892,.F.);
#9837=ORIENTED_EDGE('',*,*,#7138,.T.);
#9838=ORIENTED_EDGE('',*,*,#7142,.F.);
#9839=ORIENTED_EDGE('',*,*,#7143,.T.);
#9840=ORIENTED_EDGE('',*,*,#6894,.F.);
#9841=ORIENTED_EDGE('',*,*,#7143,.F.);
#9842=ORIENTED_EDGE('',*,*,#7144,.F.);
#9843=ORIENTED_EDGE('',*,*,#7145,.F.);
#9844=ORIENTED_EDGE('',*,*,#6895,.F.);
#9845=ORIENTED_EDGE('',*,*,#7146,.F.);
#9846=ORIENTED_EDGE('',*,*,#6897,.F.);
#9847=ORIENTED_EDGE('',*,*,#7147,.T.);
#9848=ORIENTED_EDGE('',*,*,#7148,.F.);
#9849=ORIENTED_EDGE('',*,*,#7145,.T.);
#9850=ORIENTED_EDGE('',*,*,#7149,.F.);
#9851=ORIENTED_EDGE('',*,*,#7147,.F.);
#9852=ORIENTED_EDGE('',*,*,#6896,.F.);
#9853=ORIENTED_EDGE('',*,*,#7146,.T.);
#9854=ORIENTED_EDGE('',*,*,#7150,.F.);
#9855=ORIENTED_EDGE('',*,*,#7151,.T.);
#9856=ORIENTED_EDGE('',*,*,#6898,.F.);
#9857=ORIENTED_EDGE('',*,*,#7151,.F.);
#9858=ORIENTED_EDGE('',*,*,#7152,.F.);
#9859=ORIENTED_EDGE('',*,*,#7153,.F.);
#9860=ORIENTED_EDGE('',*,*,#6899,.F.);
#9861=ORIENTED_EDGE('',*,*,#7154,.F.);
#9862=ORIENTED_EDGE('',*,*,#6901,.F.);
#9863=ORIENTED_EDGE('',*,*,#7155,.T.);
#9864=ORIENTED_EDGE('',*,*,#7156,.F.);
#9865=ORIENTED_EDGE('',*,*,#7153,.T.);
#9866=ORIENTED_EDGE('',*,*,#7157,.F.);
#9867=ORIENTED_EDGE('',*,*,#7155,.F.);
#9868=ORIENTED_EDGE('',*,*,#6900,.F.);
#9869=ORIENTED_EDGE('',*,*,#7154,.T.);
#9870=ORIENTED_EDGE('',*,*,#7158,.F.);
#9871=ORIENTED_EDGE('',*,*,#7159,.T.);
#9872=ORIENTED_EDGE('',*,*,#6902,.F.);
#9873=ORIENTED_EDGE('',*,*,#7159,.F.);
#9874=ORIENTED_EDGE('',*,*,#7160,.F.);
#9875=ORIENTED_EDGE('',*,*,#7161,.F.);
#9876=ORIENTED_EDGE('',*,*,#6903,.F.);
#9877=ORIENTED_EDGE('',*,*,#7162,.F.);
#9878=ORIENTED_EDGE('',*,*,#6905,.F.);
#9879=ORIENTED_EDGE('',*,*,#7163,.T.);
#9880=ORIENTED_EDGE('',*,*,#7164,.F.);
#9881=ORIENTED_EDGE('',*,*,#7161,.T.);
#9882=ORIENTED_EDGE('',*,*,#7165,.F.);
#9883=ORIENTED_EDGE('',*,*,#7163,.F.);
#9884=ORIENTED_EDGE('',*,*,#6904,.F.);
#9885=ORIENTED_EDGE('',*,*,#7162,.T.);
#9886=ORIENTED_EDGE('',*,*,#7166,.F.);
#9887=ORIENTED_EDGE('',*,*,#7167,.T.);
#9888=ORIENTED_EDGE('',*,*,#6906,.F.);
#9889=ORIENTED_EDGE('',*,*,#7167,.F.);
#9890=ORIENTED_EDGE('',*,*,#7168,.F.);
#9891=ORIENTED_EDGE('',*,*,#7169,.F.);
#9892=ORIENTED_EDGE('',*,*,#6907,.F.);
#9893=ORIENTED_EDGE('',*,*,#7170,.F.);
#9894=ORIENTED_EDGE('',*,*,#6909,.F.);
#9895=ORIENTED_EDGE('',*,*,#7171,.T.);
#9896=ORIENTED_EDGE('',*,*,#7172,.F.);
#9897=ORIENTED_EDGE('',*,*,#7169,.T.);
#9898=ORIENTED_EDGE('',*,*,#7173,.F.);
#9899=ORIENTED_EDGE('',*,*,#7171,.F.);
#9900=ORIENTED_EDGE('',*,*,#6908,.F.);
#9901=ORIENTED_EDGE('',*,*,#7170,.T.);
#9902=ORIENTED_EDGE('',*,*,#7174,.F.);
#9903=ORIENTED_EDGE('',*,*,#7175,.T.);
#9904=ORIENTED_EDGE('',*,*,#6910,.F.);
#9905=ORIENTED_EDGE('',*,*,#7175,.F.);
#9906=ORIENTED_EDGE('',*,*,#7176,.F.);
#9907=ORIENTED_EDGE('',*,*,#7177,.F.);
#9908=ORIENTED_EDGE('',*,*,#6911,.F.);
#9909=ORIENTED_EDGE('',*,*,#7178,.F.);
#9910=ORIENTED_EDGE('',*,*,#6913,.F.);
#9911=ORIENTED_EDGE('',*,*,#7179,.T.);
#9912=ORIENTED_EDGE('',*,*,#7180,.F.);
#9913=ORIENTED_EDGE('',*,*,#7177,.T.);
#9914=ORIENTED_EDGE('',*,*,#7181,.F.);
#9915=ORIENTED_EDGE('',*,*,#7179,.F.);
#9916=ORIENTED_EDGE('',*,*,#6912,.F.);
#9917=ORIENTED_EDGE('',*,*,#7178,.T.);
#9918=ORIENTED_EDGE('',*,*,#7182,.F.);
#9919=ORIENTED_EDGE('',*,*,#7183,.T.);
#9920=ORIENTED_EDGE('',*,*,#6914,.F.);
#9921=ORIENTED_EDGE('',*,*,#7183,.F.);
#9922=ORIENTED_EDGE('',*,*,#7184,.F.);
#9923=ORIENTED_EDGE('',*,*,#7185,.F.);
#9924=ORIENTED_EDGE('',*,*,#6915,.F.);
#9925=ORIENTED_EDGE('',*,*,#7186,.F.);
#9926=ORIENTED_EDGE('',*,*,#6917,.F.);
#9927=ORIENTED_EDGE('',*,*,#7187,.T.);
#9928=ORIENTED_EDGE('',*,*,#7188,.F.);
#9929=ORIENTED_EDGE('',*,*,#7185,.T.);
#9930=ORIENTED_EDGE('',*,*,#7189,.F.);
#9931=ORIENTED_EDGE('',*,*,#7187,.F.);
#9932=ORIENTED_EDGE('',*,*,#6916,.F.);
#9933=ORIENTED_EDGE('',*,*,#7186,.T.);
#9934=ORIENTED_EDGE('',*,*,#7190,.F.);
#9935=ORIENTED_EDGE('',*,*,#7191,.T.);
#9936=ORIENTED_EDGE('',*,*,#6918,.F.);
#9937=ORIENTED_EDGE('',*,*,#7191,.F.);
#9938=ORIENTED_EDGE('',*,*,#7192,.F.);
#9939=ORIENTED_EDGE('',*,*,#7193,.F.);
#9940=ORIENTED_EDGE('',*,*,#6919,.F.);
#9941=ORIENTED_EDGE('',*,*,#7194,.F.);
#9942=ORIENTED_EDGE('',*,*,#6921,.F.);
#9943=ORIENTED_EDGE('',*,*,#7195,.T.);
#9944=ORIENTED_EDGE('',*,*,#7196,.F.);
#9945=ORIENTED_EDGE('',*,*,#7193,.T.);
#9946=ORIENTED_EDGE('',*,*,#7197,.F.);
#9947=ORIENTED_EDGE('',*,*,#7195,.F.);
#9948=ORIENTED_EDGE('',*,*,#6920,.F.);
#9949=ORIENTED_EDGE('',*,*,#7194,.T.);
#9950=ORIENTED_EDGE('',*,*,#7198,.F.);
#9951=ORIENTED_EDGE('',*,*,#7199,.T.);
#9952=ORIENTED_EDGE('',*,*,#6922,.F.);
#9953=ORIENTED_EDGE('',*,*,#7199,.F.);
#9954=ORIENTED_EDGE('',*,*,#7200,.F.);
#9955=ORIENTED_EDGE('',*,*,#7201,.F.);
#9956=ORIENTED_EDGE('',*,*,#6923,.F.);
#9957=ORIENTED_EDGE('',*,*,#7202,.F.);
#9958=ORIENTED_EDGE('',*,*,#6925,.F.);
#9959=ORIENTED_EDGE('',*,*,#7203,.T.);
#9960=ORIENTED_EDGE('',*,*,#7204,.F.);
#9961=ORIENTED_EDGE('',*,*,#7201,.T.);
#9962=ORIENTED_EDGE('',*,*,#7205,.F.);
#9963=ORIENTED_EDGE('',*,*,#7203,.F.);
#9964=ORIENTED_EDGE('',*,*,#6924,.F.);
#9965=ORIENTED_EDGE('',*,*,#7202,.T.);
#9966=ORIENTED_EDGE('',*,*,#7206,.F.);
#9967=ORIENTED_EDGE('',*,*,#7207,.T.);
#9968=ORIENTED_EDGE('',*,*,#6926,.F.);
#9969=ORIENTED_EDGE('',*,*,#7207,.F.);
#9970=ORIENTED_EDGE('',*,*,#7208,.F.);
#9971=ORIENTED_EDGE('',*,*,#7209,.F.);
#9972=ORIENTED_EDGE('',*,*,#6927,.F.);
#9973=ORIENTED_EDGE('',*,*,#7210,.F.);
#9974=ORIENTED_EDGE('',*,*,#6929,.F.);
#9975=ORIENTED_EDGE('',*,*,#7211,.T.);
#9976=ORIENTED_EDGE('',*,*,#7212,.F.);
#9977=ORIENTED_EDGE('',*,*,#7209,.T.);
#9978=ORIENTED_EDGE('',*,*,#7213,.F.);
#9979=ORIENTED_EDGE('',*,*,#7211,.F.);
#9980=ORIENTED_EDGE('',*,*,#6928,.F.);
#9981=ORIENTED_EDGE('',*,*,#7210,.T.);
#9982=ORIENTED_EDGE('',*,*,#7214,.F.);
#9983=ORIENTED_EDGE('',*,*,#7215,.T.);
#9984=ORIENTED_EDGE('',*,*,#6930,.F.);
#9985=ORIENTED_EDGE('',*,*,#7215,.F.);
#9986=ORIENTED_EDGE('',*,*,#7216,.F.);
#9987=ORIENTED_EDGE('',*,*,#7217,.F.);
#9988=ORIENTED_EDGE('',*,*,#6931,.F.);
#9989=ORIENTED_EDGE('',*,*,#7218,.F.);
#9990=ORIENTED_EDGE('',*,*,#6933,.F.);
#9991=ORIENTED_EDGE('',*,*,#7219,.T.);
#9992=ORIENTED_EDGE('',*,*,#7220,.F.);
#9993=ORIENTED_EDGE('',*,*,#7217,.T.);
#9994=ORIENTED_EDGE('',*,*,#7221,.F.);
#9995=ORIENTED_EDGE('',*,*,#7219,.F.);
#9996=ORIENTED_EDGE('',*,*,#6932,.F.);
#9997=ORIENTED_EDGE('',*,*,#7218,.T.);
#9998=ORIENTED_EDGE('',*,*,#7222,.F.);
#9999=ORIENTED_EDGE('',*,*,#7223,.T.);
#10000=ORIENTED_EDGE('',*,*,#6934,.F.);
#10001=ORIENTED_EDGE('',*,*,#7223,.F.);
#10002=ORIENTED_EDGE('',*,*,#7224,.F.);
#10003=ORIENTED_EDGE('',*,*,#7225,.F.);
#10004=ORIENTED_EDGE('',*,*,#6935,.F.);
#10005=ORIENTED_EDGE('',*,*,#7226,.F.);
#10006=ORIENTED_EDGE('',*,*,#6937,.F.);
#10007=ORIENTED_EDGE('',*,*,#7227,.T.);
#10008=ORIENTED_EDGE('',*,*,#7228,.F.);
#10009=ORIENTED_EDGE('',*,*,#7225,.T.);
#10010=ORIENTED_EDGE('',*,*,#7229,.F.);
#10011=ORIENTED_EDGE('',*,*,#7227,.F.);
#10012=ORIENTED_EDGE('',*,*,#6936,.F.);
#10013=ORIENTED_EDGE('',*,*,#7226,.T.);
#10014=ORIENTED_EDGE('',*,*,#7230,.F.);
#10015=ORIENTED_EDGE('',*,*,#7231,.T.);
#10016=ORIENTED_EDGE('',*,*,#6938,.F.);
#10017=ORIENTED_EDGE('',*,*,#7231,.F.);
#10018=ORIENTED_EDGE('',*,*,#7232,.F.);
#10019=ORIENTED_EDGE('',*,*,#7233,.F.);
#10020=ORIENTED_EDGE('',*,*,#6939,.F.);
#10021=ORIENTED_EDGE('',*,*,#7234,.F.);
#10022=ORIENTED_EDGE('',*,*,#6941,.F.);
#10023=ORIENTED_EDGE('',*,*,#7235,.T.);
#10024=ORIENTED_EDGE('',*,*,#7236,.F.);
#10025=ORIENTED_EDGE('',*,*,#7233,.T.);
#10026=ORIENTED_EDGE('',*,*,#7237,.F.);
#10027=ORIENTED_EDGE('',*,*,#7235,.F.);
#10028=ORIENTED_EDGE('',*,*,#6940,.F.);
#10029=ORIENTED_EDGE('',*,*,#7234,.T.);
#10030=ORIENTED_EDGE('',*,*,#7238,.F.);
#10031=ORIENTED_EDGE('',*,*,#7239,.T.);
#10032=ORIENTED_EDGE('',*,*,#6942,.F.);
#10033=ORIENTED_EDGE('',*,*,#7239,.F.);
#10034=ORIENTED_EDGE('',*,*,#7240,.F.);
#10035=ORIENTED_EDGE('',*,*,#7241,.F.);
#10036=ORIENTED_EDGE('',*,*,#6943,.F.);
#10037=ORIENTED_EDGE('',*,*,#7242,.F.);
#10038=ORIENTED_EDGE('',*,*,#6945,.F.);
#10039=ORIENTED_EDGE('',*,*,#7243,.T.);
#10040=ORIENTED_EDGE('',*,*,#7244,.F.);
#10041=ORIENTED_EDGE('',*,*,#7241,.T.);
#10042=ORIENTED_EDGE('',*,*,#7245,.F.);
#10043=ORIENTED_EDGE('',*,*,#7243,.F.);
#10044=ORIENTED_EDGE('',*,*,#6944,.F.);
#10045=ORIENTED_EDGE('',*,*,#7242,.T.);
#10046=ORIENTED_EDGE('',*,*,#7246,.F.);
#10047=ORIENTED_EDGE('',*,*,#7247,.T.);
#10048=ORIENTED_EDGE('',*,*,#6946,.F.);
#10049=ORIENTED_EDGE('',*,*,#7247,.F.);
#10050=ORIENTED_EDGE('',*,*,#7248,.F.);
#10051=ORIENTED_EDGE('',*,*,#7249,.F.);
#10052=ORIENTED_EDGE('',*,*,#6947,.F.);
#10053=ORIENTED_EDGE('',*,*,#7250,.F.);
#10054=ORIENTED_EDGE('',*,*,#6949,.F.);
#10055=ORIENTED_EDGE('',*,*,#7251,.T.);
#10056=ORIENTED_EDGE('',*,*,#7252,.F.);
#10057=ORIENTED_EDGE('',*,*,#7249,.T.);
#10058=ORIENTED_EDGE('',*,*,#7253,.F.);
#10059=ORIENTED_EDGE('',*,*,#7251,.F.);
#10060=ORIENTED_EDGE('',*,*,#6948,.F.);
#10061=ORIENTED_EDGE('',*,*,#7250,.T.);
#10062=ORIENTED_EDGE('',*,*,#7254,.F.);
#10063=ORIENTED_EDGE('',*,*,#7255,.T.);
#10064=ORIENTED_EDGE('',*,*,#6950,.F.);
#10065=ORIENTED_EDGE('',*,*,#7255,.F.);
#10066=ORIENTED_EDGE('',*,*,#7256,.F.);
#10067=ORIENTED_EDGE('',*,*,#7257,.F.);
#10068=ORIENTED_EDGE('',*,*,#6951,.F.);
#10069=ORIENTED_EDGE('',*,*,#7258,.F.);
#10070=ORIENTED_EDGE('',*,*,#6953,.F.);
#10071=ORIENTED_EDGE('',*,*,#7259,.T.);
#10072=ORIENTED_EDGE('',*,*,#7260,.F.);
#10073=ORIENTED_EDGE('',*,*,#7257,.T.);
#10074=ORIENTED_EDGE('',*,*,#7261,.F.);
#10075=ORIENTED_EDGE('',*,*,#7259,.F.);
#10076=ORIENTED_EDGE('',*,*,#6952,.F.);
#10077=ORIENTED_EDGE('',*,*,#7258,.T.);
#10078=ORIENTED_EDGE('',*,*,#7262,.F.);
#10079=ORIENTED_EDGE('',*,*,#7263,.T.);
#10080=ORIENTED_EDGE('',*,*,#6954,.F.);
#10081=ORIENTED_EDGE('',*,*,#7263,.F.);
#10082=ORIENTED_EDGE('',*,*,#7264,.F.);
#10083=ORIENTED_EDGE('',*,*,#7265,.F.);
#10084=ORIENTED_EDGE('',*,*,#6955,.F.);
#10085=ORIENTED_EDGE('',*,*,#7266,.F.);
#10086=ORIENTED_EDGE('',*,*,#6957,.F.);
#10087=ORIENTED_EDGE('',*,*,#7267,.T.);
#10088=ORIENTED_EDGE('',*,*,#7268,.F.);
#10089=ORIENTED_EDGE('',*,*,#7265,.T.);
#10090=ORIENTED_EDGE('',*,*,#7269,.F.);
#10091=ORIENTED_EDGE('',*,*,#7267,.F.);
#10092=ORIENTED_EDGE('',*,*,#6956,.F.);
#10093=ORIENTED_EDGE('',*,*,#7266,.T.);
#10094=ORIENTED_EDGE('',*,*,#7270,.F.);
#10095=ORIENTED_EDGE('',*,*,#7271,.T.);
#10096=ORIENTED_EDGE('',*,*,#6958,.F.);
#10097=ORIENTED_EDGE('',*,*,#7271,.F.);
#10098=ORIENTED_EDGE('',*,*,#7272,.F.);
#10099=ORIENTED_EDGE('',*,*,#7273,.F.);
#10100=ORIENTED_EDGE('',*,*,#6959,.F.);
#10101=ORIENTED_EDGE('',*,*,#7274,.F.);
#10102=ORIENTED_EDGE('',*,*,#6961,.F.);
#10103=ORIENTED_EDGE('',*,*,#7275,.T.);
#10104=ORIENTED_EDGE('',*,*,#7276,.F.);
#10105=ORIENTED_EDGE('',*,*,#7273,.T.);
#10106=ORIENTED_EDGE('',*,*,#7277,.F.);
#10107=ORIENTED_EDGE('',*,*,#7275,.F.);
#10108=ORIENTED_EDGE('',*,*,#6960,.F.);
#10109=ORIENTED_EDGE('',*,*,#7274,.T.);
#10110=ORIENTED_EDGE('',*,*,#7278,.F.);
#10111=ORIENTED_EDGE('',*,*,#7279,.T.);
#10112=ORIENTED_EDGE('',*,*,#6962,.F.);
#10113=ORIENTED_EDGE('',*,*,#7279,.F.);
#10114=ORIENTED_EDGE('',*,*,#7280,.F.);
#10115=ORIENTED_EDGE('',*,*,#7281,.F.);
#10116=ORIENTED_EDGE('',*,*,#6963,.F.);
#10117=ORIENTED_EDGE('',*,*,#7282,.F.);
#10118=ORIENTED_EDGE('',*,*,#6965,.F.);
#10119=ORIENTED_EDGE('',*,*,#7283,.T.);
#10120=ORIENTED_EDGE('',*,*,#7284,.F.);
#10121=ORIENTED_EDGE('',*,*,#7281,.T.);
#10122=ORIENTED_EDGE('',*,*,#7285,.F.);
#10123=ORIENTED_EDGE('',*,*,#7283,.F.);
#10124=ORIENTED_EDGE('',*,*,#6964,.F.);
#10125=ORIENTED_EDGE('',*,*,#7282,.T.);
#10126=ORIENTED_EDGE('',*,*,#7286,.F.);
#10127=ORIENTED_EDGE('',*,*,#7287,.T.);
#10128=ORIENTED_EDGE('',*,*,#6966,.F.);
#10129=ORIENTED_EDGE('',*,*,#7287,.F.);
#10130=ORIENTED_EDGE('',*,*,#7288,.F.);
#10131=ORIENTED_EDGE('',*,*,#7289,.F.);
#10132=ORIENTED_EDGE('',*,*,#6967,.F.);
#10133=ORIENTED_EDGE('',*,*,#7289,.T.);
#10134=ORIENTED_EDGE('',*,*,#7290,.F.);
#10135=ORIENTED_EDGE('',*,*,#7291,.F.);
#10136=ORIENTED_EDGE('',*,*,#6968,.F.);
#10137=ORIENTED_EDGE('',*,*,#7292,.F.);
#10138=ORIENTED_EDGE('',*,*,#6969,.F.);
#10139=ORIENTED_EDGE('',*,*,#7291,.T.);
#10140=ORIENTED_EDGE('',*,*,#7293,.F.);
#10141=ORIENTED_EDGE('',*,*,#7292,.T.);
#10142=ORIENTED_EDGE('',*,*,#7294,.F.);
#10143=ORIENTED_EDGE('',*,*,#7295,.T.);
#10144=ORIENTED_EDGE('',*,*,#6970,.F.);
#10145=ORIENTED_EDGE('',*,*,#7296,.F.);
#10146=ORIENTED_EDGE('',*,*,#6973,.F.);
#10147=ORIENTED_EDGE('',*,*,#7297,.T.);
#10148=ORIENTED_EDGE('',*,*,#7298,.F.);
#10149=ORIENTED_EDGE('',*,*,#7295,.F.);
#10150=ORIENTED_EDGE('',*,*,#7299,.F.);
#10151=ORIENTED_EDGE('',*,*,#7300,.F.);
#10152=ORIENTED_EDGE('',*,*,#6971,.F.);
#10153=ORIENTED_EDGE('',*,*,#7300,.T.);
#10154=ORIENTED_EDGE('',*,*,#7301,.F.);
#10155=ORIENTED_EDGE('',*,*,#7297,.F.);
#10156=ORIENTED_EDGE('',*,*,#6972,.F.);
#10157=ORIENTED_EDGE('',*,*,#6988,.T.);
#10158=ORIENTED_EDGE('',*,*,#6989,.T.);
#10159=ORIENTED_EDGE('',*,*,#6984,.T.);
#10160=ORIENTED_EDGE('',*,*,#7302,.T.);
#10161=ORIENTED_EDGE('',*,*,#7298,.T.);
#10162=ORIENTED_EDGE('',*,*,#7301,.T.);
#10163=ORIENTED_EDGE('',*,*,#7299,.T.);
#10164=ORIENTED_EDGE('',*,*,#7294,.T.);
#10165=ORIENTED_EDGE('',*,*,#7293,.T.);
#10166=ORIENTED_EDGE('',*,*,#7290,.T.);
#10167=ORIENTED_EDGE('',*,*,#7288,.T.);
#10168=ORIENTED_EDGE('',*,*,#7286,.T.);
#10169=ORIENTED_EDGE('',*,*,#7284,.T.);
#10170=ORIENTED_EDGE('',*,*,#7285,.T.);
#10171=ORIENTED_EDGE('',*,*,#7280,.T.);
#10172=ORIENTED_EDGE('',*,*,#7278,.T.);
#10173=ORIENTED_EDGE('',*,*,#7276,.T.);
#10174=ORIENTED_EDGE('',*,*,#7277,.T.);
#10175=ORIENTED_EDGE('',*,*,#7272,.T.);
#10176=ORIENTED_EDGE('',*,*,#7270,.T.);
#10177=ORIENTED_EDGE('',*,*,#7268,.T.);
#10178=ORIENTED_EDGE('',*,*,#7269,.T.);
#10179=ORIENTED_EDGE('',*,*,#7264,.T.);
#10180=ORIENTED_EDGE('',*,*,#7262,.T.);
#10181=ORIENTED_EDGE('',*,*,#7260,.T.);
#10182=ORIENTED_EDGE('',*,*,#7261,.T.);
#10183=ORIENTED_EDGE('',*,*,#7256,.T.);
#10184=ORIENTED_EDGE('',*,*,#7254,.T.);
#10185=ORIENTED_EDGE('',*,*,#7252,.T.);
#10186=ORIENTED_EDGE('',*,*,#7253,.T.);
#10187=ORIENTED_EDGE('',*,*,#7248,.T.);
#10188=ORIENTED_EDGE('',*,*,#7246,.T.);
#10189=ORIENTED_EDGE('',*,*,#7244,.T.);
#10190=ORIENTED_EDGE('',*,*,#7245,.T.);
#10191=ORIENTED_EDGE('',*,*,#7240,.T.);
#10192=ORIENTED_EDGE('',*,*,#7238,.T.);
#10193=ORIENTED_EDGE('',*,*,#7236,.T.);
#10194=ORIENTED_EDGE('',*,*,#7237,.T.);
#10195=ORIENTED_EDGE('',*,*,#7232,.T.);
#10196=ORIENTED_EDGE('',*,*,#7230,.T.);
#10197=ORIENTED_EDGE('',*,*,#7228,.T.);
#10198=ORIENTED_EDGE('',*,*,#7229,.T.);
#10199=ORIENTED_EDGE('',*,*,#7224,.T.);
#10200=ORIENTED_EDGE('',*,*,#7222,.T.);
#10201=ORIENTED_EDGE('',*,*,#7220,.T.);
#10202=ORIENTED_EDGE('',*,*,#7221,.T.);
#10203=ORIENTED_EDGE('',*,*,#7216,.T.);
#10204=ORIENTED_EDGE('',*,*,#7214,.T.);
#10205=ORIENTED_EDGE('',*,*,#7212,.T.);
#10206=ORIENTED_EDGE('',*,*,#7213,.T.);
#10207=ORIENTED_EDGE('',*,*,#7208,.T.);
#10208=ORIENTED_EDGE('',*,*,#7206,.T.);
#10209=ORIENTED_EDGE('',*,*,#7204,.T.);
#10210=ORIENTED_EDGE('',*,*,#7205,.T.);
#10211=ORIENTED_EDGE('',*,*,#7200,.T.);
#10212=ORIENTED_EDGE('',*,*,#7198,.T.);
#10213=ORIENTED_EDGE('',*,*,#7196,.T.);
#10214=ORIENTED_EDGE('',*,*,#7197,.T.);
#10215=ORIENTED_EDGE('',*,*,#7192,.T.);
#10216=ORIENTED_EDGE('',*,*,#7190,.T.);
#10217=ORIENTED_EDGE('',*,*,#7188,.T.);
#10218=ORIENTED_EDGE('',*,*,#7189,.T.);
#10219=ORIENTED_EDGE('',*,*,#7184,.T.);
#10220=ORIENTED_EDGE('',*,*,#7182,.T.);
#10221=ORIENTED_EDGE('',*,*,#7180,.T.);
#10222=ORIENTED_EDGE('',*,*,#7181,.T.);
#10223=ORIENTED_EDGE('',*,*,#7176,.T.);
#10224=ORIENTED_EDGE('',*,*,#7174,.T.);
#10225=ORIENTED_EDGE('',*,*,#7172,.T.);
#10226=ORIENTED_EDGE('',*,*,#7173,.T.);
#10227=ORIENTED_EDGE('',*,*,#7168,.T.);
#10228=ORIENTED_EDGE('',*,*,#7166,.T.);
#10229=ORIENTED_EDGE('',*,*,#7164,.T.);
#10230=ORIENTED_EDGE('',*,*,#7165,.T.);
#10231=ORIENTED_EDGE('',*,*,#7160,.T.);
#10232=ORIENTED_EDGE('',*,*,#7158,.T.);
#10233=ORIENTED_EDGE('',*,*,#7156,.T.);
#10234=ORIENTED_EDGE('',*,*,#7157,.T.);
#10235=ORIENTED_EDGE('',*,*,#7152,.T.);
#10236=ORIENTED_EDGE('',*,*,#7150,.T.);
#10237=ORIENTED_EDGE('',*,*,#7148,.T.);
#10238=ORIENTED_EDGE('',*,*,#7149,.T.);
#10239=ORIENTED_EDGE('',*,*,#7144,.T.);
#10240=ORIENTED_EDGE('',*,*,#7142,.T.);
#10241=ORIENTED_EDGE('',*,*,#7140,.T.);
#10242=ORIENTED_EDGE('',*,*,#7141,.T.);
#10243=ORIENTED_EDGE('',*,*,#7136,.T.);
#10244=ORIENTED_EDGE('',*,*,#7134,.T.);
#10245=ORIENTED_EDGE('',*,*,#7132,.T.);
#10246=ORIENTED_EDGE('',*,*,#7133,.T.);
#10247=ORIENTED_EDGE('',*,*,#7128,.T.);
#10248=ORIENTED_EDGE('',*,*,#7126,.T.);
#10249=ORIENTED_EDGE('',*,*,#7124,.T.);
#10250=ORIENTED_EDGE('',*,*,#7125,.T.);
#10251=ORIENTED_EDGE('',*,*,#7120,.T.);
#10252=ORIENTED_EDGE('',*,*,#7118,.T.);
#10253=ORIENTED_EDGE('',*,*,#7116,.T.);
#10254=ORIENTED_EDGE('',*,*,#7117,.T.);
#10255=ORIENTED_EDGE('',*,*,#7112,.T.);
#10256=ORIENTED_EDGE('',*,*,#7110,.T.);
#10257=ORIENTED_EDGE('',*,*,#7108,.T.);
#10258=ORIENTED_EDGE('',*,*,#7109,.T.);
#10259=ORIENTED_EDGE('',*,*,#7104,.T.);
#10260=ORIENTED_EDGE('',*,*,#7102,.T.);
#10261=ORIENTED_EDGE('',*,*,#7100,.T.);
#10262=ORIENTED_EDGE('',*,*,#7101,.T.);
#10263=ORIENTED_EDGE('',*,*,#7096,.T.);
#10264=ORIENTED_EDGE('',*,*,#7094,.T.);
#10265=ORIENTED_EDGE('',*,*,#7092,.T.);
#10266=ORIENTED_EDGE('',*,*,#7093,.T.);
#10267=ORIENTED_EDGE('',*,*,#7088,.T.);
#10268=ORIENTED_EDGE('',*,*,#7086,.T.);
#10269=ORIENTED_EDGE('',*,*,#7084,.T.);
#10270=ORIENTED_EDGE('',*,*,#7085,.T.);
#10271=ORIENTED_EDGE('',*,*,#7080,.T.);
#10272=ORIENTED_EDGE('',*,*,#7078,.T.);
#10273=ORIENTED_EDGE('',*,*,#7076,.T.);
#10274=ORIENTED_EDGE('',*,*,#7077,.T.);
#10275=ORIENTED_EDGE('',*,*,#7072,.T.);
#10276=ORIENTED_EDGE('',*,*,#7070,.T.);
#10277=ORIENTED_EDGE('',*,*,#7068,.T.);
#10278=ORIENTED_EDGE('',*,*,#7069,.T.);
#10279=ORIENTED_EDGE('',*,*,#7064,.T.);
#10280=ORIENTED_EDGE('',*,*,#7062,.T.);
#10281=ORIENTED_EDGE('',*,*,#7060,.T.);
#10282=ORIENTED_EDGE('',*,*,#7061,.T.);
#10283=ORIENTED_EDGE('',*,*,#7056,.T.);
#10284=ORIENTED_EDGE('',*,*,#7054,.T.);
#10285=ORIENTED_EDGE('',*,*,#7052,.T.);
#10286=ORIENTED_EDGE('',*,*,#7053,.T.);
#10287=ORIENTED_EDGE('',*,*,#7048,.T.);
#10288=ORIENTED_EDGE('',*,*,#7046,.T.);
#10289=ORIENTED_EDGE('',*,*,#7044,.T.);
#10290=ORIENTED_EDGE('',*,*,#7045,.T.);
#10291=ORIENTED_EDGE('',*,*,#7040,.T.);
#10292=ORIENTED_EDGE('',*,*,#7038,.T.);
#10293=ORIENTED_EDGE('',*,*,#7036,.T.);
#10294=ORIENTED_EDGE('',*,*,#7037,.T.);
#10295=ORIENTED_EDGE('',*,*,#7032,.T.);
#10296=ORIENTED_EDGE('',*,*,#7030,.T.);
#10297=ORIENTED_EDGE('',*,*,#7028,.T.);
#10298=ORIENTED_EDGE('',*,*,#7029,.T.);
#10299=ORIENTED_EDGE('',*,*,#7024,.T.);
#10300=ORIENTED_EDGE('',*,*,#7022,.T.);
#10301=ORIENTED_EDGE('',*,*,#7020,.T.);
#10302=ORIENTED_EDGE('',*,*,#7021,.T.);
#10303=ORIENTED_EDGE('',*,*,#7016,.T.);
#10304=ORIENTED_EDGE('',*,*,#7014,.T.);
#10305=ORIENTED_EDGE('',*,*,#7012,.T.);
#10306=ORIENTED_EDGE('',*,*,#7013,.T.);
#10307=ORIENTED_EDGE('',*,*,#7008,.T.);
#10308=ORIENTED_EDGE('',*,*,#7006,.T.);
#10309=ORIENTED_EDGE('',*,*,#7004,.T.);
#10310=ORIENTED_EDGE('',*,*,#7005,.T.);
#10311=ORIENTED_EDGE('',*,*,#7000,.T.);
#10312=ORIENTED_EDGE('',*,*,#6998,.T.);
#10313=ORIENTED_EDGE('',*,*,#6996,.T.);
#10314=ORIENTED_EDGE('',*,*,#6997,.T.);
#10315=ORIENTED_EDGE('',*,*,#6992,.T.);
#10316=ORIENTED_EDGE('',*,*,#6990,.T.);
#10317=ORIENTED_EDGE('',*,*,#6982,.T.);
#10318=ORIENTED_EDGE('',*,*,#6983,.T.);
#10319=ORIENTED_EDGE('',*,*,#6974,.F.);
#10320=ORIENTED_EDGE('',*,*,#7296,.T.);
#10321=ORIENTED_EDGE('',*,*,#7302,.F.);
#10322=ORIENTED_EDGE('',*,*,#7303,.F.);
#10323=ORIENTED_EDGE('',*,*,#7304,.F.);
#10324=ORIENTED_EDGE('',*,*,#7305,.F.);
#10325=ORIENTED_EDGE('',*,*,#7306,.F.);
#10326=ORIENTED_EDGE('',*,*,#7307,.F.);
#10327=ORIENTED_EDGE('',*,*,#7308,.F.);
#10328=ORIENTED_EDGE('',*,*,#7309,.F.);
#10329=ORIENTED_EDGE('',*,*,#7310,.F.);
#10330=ORIENTED_EDGE('',*,*,#7307,.T.);
#10331=ORIENTED_EDGE('',*,*,#7311,.T.);
#10332=ORIENTED_EDGE('',*,*,#7312,.T.);
#10333=ORIENTED_EDGE('',*,*,#7313,.T.);
#10334=ORIENTED_EDGE('',*,*,#7306,.T.);
#10335=ORIENTED_EDGE('',*,*,#7314,.F.);
#10336=ORIENTED_EDGE('',*,*,#7315,.T.);
#10337=ORIENTED_EDGE('',*,*,#7311,.F.);
#10338=ORIENTED_EDGE('',*,*,#7305,.T.);
#10339=ORIENTED_EDGE('',*,*,#7316,.T.);
#10340=ORIENTED_EDGE('',*,*,#7317,.T.);
#10341=ORIENTED_EDGE('',*,*,#7314,.T.);
#10342=ORIENTED_EDGE('',*,*,#7304,.T.);
#10343=ORIENTED_EDGE('',*,*,#7318,.F.);
#10344=ORIENTED_EDGE('',*,*,#7319,.T.);
#10345=ORIENTED_EDGE('',*,*,#7316,.F.);
#10346=ORIENTED_EDGE('',*,*,#7320,.F.);
#10347=ORIENTED_EDGE('',*,*,#7321,.F.);
#10348=ORIENTED_EDGE('',*,*,#7312,.F.);
#10349=ORIENTED_EDGE('',*,*,#7315,.F.);
#10350=ORIENTED_EDGE('',*,*,#7317,.F.);
#10351=ORIENTED_EDGE('',*,*,#7319,.F.);
#10352=ORIENTED_EDGE('',*,*,#7322,.F.);
#10353=ORIENTED_EDGE('',*,*,#7323,.F.);
#10354=ORIENTED_EDGE('',*,*,#7308,.T.);
#10355=ORIENTED_EDGE('',*,*,#7313,.F.);
#10356=ORIENTED_EDGE('',*,*,#7321,.T.);
#10357=ORIENTED_EDGE('',*,*,#7324,.F.);
#10358=ORIENTED_EDGE('',*,*,#7303,.T.);
#10359=ORIENTED_EDGE('',*,*,#7325,.T.);
#10360=ORIENTED_EDGE('',*,*,#7322,.T.);
#10361=ORIENTED_EDGE('',*,*,#7318,.T.);
#10362=ORIENTED_EDGE('',*,*,#7309,.T.);
#10363=ORIENTED_EDGE('',*,*,#7324,.T.);
#10364=ORIENTED_EDGE('',*,*,#7320,.T.);
#10365=ORIENTED_EDGE('',*,*,#7326,.T.);
#10366=ORIENTED_EDGE('',*,*,#7310,.T.);
#10367=ORIENTED_EDGE('',*,*,#7326,.F.);
#10368=ORIENTED_EDGE('',*,*,#7323,.T.);
#10369=ORIENTED_EDGE('',*,*,#7325,.F.);
#10370=ORIENTED_EDGE('',*,*,#7327,.F.);
#10371=ORIENTED_EDGE('',*,*,#7328,.T.);
#10372=ORIENTED_EDGE('',*,*,#7329,.T.);
#10373=ORIENTED_EDGE('',*,*,#7330,.F.);
#10374=ORIENTED_EDGE('',*,*,#7331,.F.);
#10375=ORIENTED_EDGE('',*,*,#7332,.T.);
#10376=ORIENTED_EDGE('',*,*,#7333,.T.);
#10377=ORIENTED_EDGE('',*,*,#7328,.F.);
#10378=ORIENTED_EDGE('',*,*,#7334,.F.);
#10379=ORIENTED_EDGE('',*,*,#7335,.T.);
#10380=ORIENTED_EDGE('',*,*,#7336,.T.);
#10381=ORIENTED_EDGE('',*,*,#7332,.F.);
#10382=ORIENTED_EDGE('',*,*,#7337,.F.);
#10383=ORIENTED_EDGE('',*,*,#7338,.T.);
#10384=ORIENTED_EDGE('',*,*,#7339,.T.);
#10385=ORIENTED_EDGE('',*,*,#7335,.F.);
#10386=ORIENTED_EDGE('',*,*,#7340,.F.);
#10387=ORIENTED_EDGE('',*,*,#7341,.T.);
#10388=ORIENTED_EDGE('',*,*,#7342,.T.);
#10389=ORIENTED_EDGE('',*,*,#7338,.F.);
#10390=ORIENTED_EDGE('',*,*,#7343,.F.);
#10391=ORIENTED_EDGE('',*,*,#7330,.T.);
#10392=ORIENTED_EDGE('',*,*,#7344,.T.);
#10393=ORIENTED_EDGE('',*,*,#7341,.F.);
#10394=ORIENTED_EDGE('',*,*,#7344,.F.);
#10395=ORIENTED_EDGE('',*,*,#7329,.F.);
#10396=ORIENTED_EDGE('',*,*,#7333,.F.);
#10397=ORIENTED_EDGE('',*,*,#7336,.F.);
#10398=ORIENTED_EDGE('',*,*,#7339,.F.);
#10399=ORIENTED_EDGE('',*,*,#7342,.F.);
#10400=ORIENTED_EDGE('',*,*,#7345,.F.);
#10401=ORIENTED_EDGE('',*,*,#7327,.T.);
#10402=ORIENTED_EDGE('',*,*,#7343,.T.);
#10403=ORIENTED_EDGE('',*,*,#7340,.T.);
#10404=ORIENTED_EDGE('',*,*,#7337,.T.);
#10405=ORIENTED_EDGE('',*,*,#7334,.T.);
#10406=ORIENTED_EDGE('',*,*,#7331,.T.);
#10407=ORIENTED_EDGE('',*,*,#7346,.F.);
#10408=ORIENTED_EDGE('',*,*,#7347,.T.);
#10409=ORIENTED_EDGE('',*,*,#7345,.T.);
#10410=ORIENTED_EDGE('',*,*,#7347,.F.);
#10411=ORIENTED_EDGE('',*,*,#7348,.F.);
#10412=ORIENTED_EDGE('',*,*,#7349,.T.);
#10413=ORIENTED_EDGE('',*,*,#7346,.T.);
#10414=ORIENTED_EDGE('',*,*,#7349,.F.);
#10415=ORIENTED_EDGE('',*,*,#7350,.F.);
#10416=ORIENTED_EDGE('',*,*,#7351,.T.);
#10417=ORIENTED_EDGE('',*,*,#7348,.T.);
#10418=ORIENTED_EDGE('',*,*,#7351,.F.);
#10419=ORIENTED_EDGE('',*,*,#7350,.T.);
#10420=CYLINDRICAL_SURFACE('',#11809,0.33);
#10421=CYLINDRICAL_SURFACE('',#11812,0.33);
#10422=CYLINDRICAL_SURFACE('',#11815,0.33);
#10423=CYLINDRICAL_SURFACE('',#11818,0.33);
#10424=CYLINDRICAL_SURFACE('',#11828,0.165);
#10425=CYLINDRICAL_SURFACE('',#11831,0.165);
#10426=CYLINDRICAL_SURFACE('',#11834,0.164999999999999);
#10427=CYLINDRICAL_SURFACE('',#11837,0.165);
#10428=CYLINDRICAL_SURFACE('',#11840,0.165);
#10429=CYLINDRICAL_SURFACE('',#11843,0.165);
#10430=CYLINDRICAL_SURFACE('',#11846,0.475);
#10431=CYLINDRICAL_SURFACE('',#11851,0.475);
#10432=CYLINDRICAL_SURFACE('',#11856,0.475);
#10433=CYLINDRICAL_SURFACE('',#11861,0.475);
#10434=CYLINDRICAL_SURFACE('',#11866,0.275);
#10435=CYLINDRICAL_SURFACE('',#11868,0.275);
#10436=CYLINDRICAL_SURFACE('',#11870,0.275);
#10437=CYLINDRICAL_SURFACE('',#11872,0.275);
#10438=CYLINDRICAL_SURFACE('',#11874,0.25);
#10439=CYLINDRICAL_SURFACE('',#11878,0.25);
#10440=CYLINDRICAL_SURFACE('',#11882,2.35);
#10441=CYLINDRICAL_SURFACE('',#11887,2.15);
#10442=CYLINDRICAL_SURFACE('',#11889,1.6);
#10443=CYLINDRICAL_SURFACE('',#11894,1.4);
#10444=CYLINDRICAL_SURFACE('',#11903,0.165);
#10445=CYLINDRICAL_SURFACE('',#11906,0.165);
#10446=CYLINDRICAL_SURFACE('',#11909,0.164999999999999);
#10447=CYLINDRICAL_SURFACE('',#11912,0.165);
#10448=CYLINDRICAL_SURFACE('',#11915,0.165);
#10449=CYLINDRICAL_SURFACE('',#11918,0.165);
#10450=CYLINDRICAL_SURFACE('',#11921,0.475);
#10451=CYLINDRICAL_SURFACE('',#11926,0.475);
#10452=CYLINDRICAL_SURFACE('',#11931,0.475);
#10453=CYLINDRICAL_SURFACE('',#11936,0.475);
#10454=CYLINDRICAL_SURFACE('',#11941,0.275);
#10455=CYLINDRICAL_SURFACE('',#11943,0.275);
#10456=CYLINDRICAL_SURFACE('',#11945,0.275);
#10457=CYLINDRICAL_SURFACE('',#11947,0.275);
#10458=CYLINDRICAL_SURFACE('',#11949,0.25);
#10459=CYLINDRICAL_SURFACE('',#11953,0.25);
#10460=CYLINDRICAL_SURFACE('',#11957,2.35);
#10461=CYLINDRICAL_SURFACE('',#11962,2.15);
#10462=CYLINDRICAL_SURFACE('',#11964,1.6);
#10463=CYLINDRICAL_SURFACE('',#11969,1.4);
#10464=CYLINDRICAL_SURFACE('',#11978,0.21);
#10465=CYLINDRICAL_SURFACE('',#11981,0.5);
#10466=CYLINDRICAL_SURFACE('',#11987,0.21);
#10467=CYLINDRICAL_SURFACE('',#11990,0.5);
#10468=CYLINDRICAL_SURFACE('',#11996,0.210000000000001);
#10469=CYLINDRICAL_SURFACE('',#11999,0.5);
#10470=CYLINDRICAL_SURFACE('',#12005,0.210000000000001);
#10471=CYLINDRICAL_SURFACE('',#12008,0.5);
#10472=CYLINDRICAL_SURFACE('',#12014,0.225);
#10473=CYLINDRICAL_SURFACE('',#12017,0.225);
#10474=CYLINDRICAL_SURFACE('',#12020,0.225);
#10475=CYLINDRICAL_SURFACE('',#12023,1.59);
#10476=CYLINDRICAL_SURFACE('',#12028,1.2);
#10477=CYLINDRICAL_SURFACE('',#12030,2.2);
#10478=CYLINDRICAL_SURFACE('',#12036,0.225);
#10479=CYLINDRICAL_SURFACE('',#12039,0.225);
#10480=CYLINDRICAL_SURFACE('',#12042,0.225);
#10481=CYLINDRICAL_SURFACE('',#12045,2.34);
#10482=CYLINDRICAL_SURFACE('',#12050,1.8);
#10483=CYLINDRICAL_SURFACE('',#12052,3.);
#10484=CYLINDRICAL_SURFACE('',#12058,0.225);
#10485=CYLINDRICAL_SURFACE('',#12061,0.225);
#10486=CYLINDRICAL_SURFACE('',#12064,0.225);
#10487=CYLINDRICAL_SURFACE('',#12067,1.59);
#10488=CYLINDRICAL_SURFACE('',#12072,1.2);
#10489=CYLINDRICAL_SURFACE('',#12074,2.2);
#10490=CYLINDRICAL_SURFACE('',#12080,0.225);
#10491=CYLINDRICAL_SURFACE('',#12083,0.225);
#10492=CYLINDRICAL_SURFACE('',#12086,0.225);
#10493=CYLINDRICAL_SURFACE('',#12089,2.34);
#10494=CYLINDRICAL_SURFACE('',#12094,1.8);
#10495=CYLINDRICAL_SURFACE('',#12096,3.);
#10496=CYLINDRICAL_SURFACE('',#12106,0.425);
#10497=CYLINDRICAL_SURFACE('',#12114,0.24505);
#10498=CYLINDRICAL_SURFACE('',#12132,0.5);
#10499=CYLINDRICAL_SURFACE('',#12140,0.2942);
#10500=CYLINDRICAL_SURFACE('',#12161,1.070235);
#10501=CYLINDRICAL_SURFACE('',#12163,0.6);
#10502=CYLINDRICAL_SURFACE('',#12169,1.070235);
#10503=CYLINDRICAL_SURFACE('',#12181,1.129765);
#10504=CYLINDRICAL_SURFACE('',#12188,1.6);
#10505=CYLINDRICAL_SURFACE('',#12193,1.129765);
#10506=CYLINDRICAL_SURFACE('',#12213,1.123812);
#10507=CYLINDRICAL_SURFACE('',#12249,1.076188);
#10508=CYLINDRICAL_SURFACE('',#12263,1.119765);
#10509=CYLINDRICAL_SURFACE('',#12267,1.085235);
#10510=CYLINDRICAL_SURFACE('',#12271,1.119765);
#10511=CYLINDRICAL_SURFACE('',#12275,1.085235);
#10512=CYLINDRICAL_SURFACE('',#12289,1.63531);
#10513=CYLINDRICAL_SURFACE('',#12291,1.);
#10514=CYLINDRICAL_SURFACE('',#12297,1.63531);
#10515=CYLINDRICAL_SURFACE('',#12309,1.71469);
#10516=CYLINDRICAL_SURFACE('',#12316,2.35);
#10517=CYLINDRICAL_SURFACE('',#12321,1.71469);
#10518=CYLINDRICAL_SURFACE('',#12343,1.706752);
#10519=CYLINDRICAL_SURFACE('',#12383,1.643248);
#10520=CYLINDRICAL_SURFACE('',#12397,1.70469);
#10521=CYLINDRICAL_SURFACE('',#12401,1.65031);
#10522=CYLINDRICAL_SURFACE('',#12405,1.70469);
#10523=CYLINDRICAL_SURFACE('',#12409,1.65031);
#10524=CYLINDRICAL_SURFACE('',#12420,0.35);
#10525=CYLINDRICAL_SURFACE('',#12428,0.1954);
#10526=CYLINDRICAL_SURFACE('',#12489,0.6);
#10527=CYLINDRICAL_SURFACE('',#12495,0.61);
#10528=CYLINDRICAL_SURFACE('',#12498,0.9);
#10529=CYLINDRICAL_SURFACE('',#12504,0.61);
#10530=CYLINDRICAL_SURFACE('',#12507,0.9);
#10531=CYLINDRICAL_SURFACE('',#12515,0.21);
#10532=CYLINDRICAL_SURFACE('',#12519,0.605);
#10533=CYLINDRICAL_SURFACE('',#12522,1.1);
#10534=CYLINDRICAL_SURFACE('',#12528,0.61);
#10535=CYLINDRICAL_SURFACE('',#12531,0.9);
#10536=CYLINDRICAL_SURFACE('',#12539,0.21);
#10537=CYLINDRICAL_SURFACE('',#12543,0.605);
#10538=CYLINDRICAL_SURFACE('',#12546,1.1);
#10539=CYLINDRICAL_SURFACE('',#12552,0.61);
#10540=CYLINDRICAL_SURFACE('',#12555,0.9);
#10541=CYLINDRICAL_SURFACE('',#12586,0.6);
#10542=CYLINDRICAL_SURFACE('',#12588,1.4);
#10543=CYLINDRICAL_SURFACE('',#12593,1.75);
#10544=CYLINDRICAL_SURFACE('',#12596,1.75);
#10545=CYLINDRICAL_SURFACE('',#12599,1.75);
#10546=CYLINDRICAL_SURFACE('',#12602,1.75);
#10547=CYLINDRICAL_SURFACE('',#12605,1.75);
#10548=CYLINDRICAL_SURFACE('',#12608,1.75);
#10549=CYLINDRICAL_SURFACE('',#12611,1.75);
#10550=CYLINDRICAL_SURFACE('',#12614,1.75);
#10551=CYLINDRICAL_SURFACE('',#12617,1.75);
#10552=CYLINDRICAL_SURFACE('',#12620,1.75);
#10553=CYLINDRICAL_SURFACE('',#12623,1.75);
#10554=CYLINDRICAL_SURFACE('',#12626,1.75);
#10555=CYLINDRICAL_SURFACE('',#12629,1.75);
#10556=CYLINDRICAL_SURFACE('',#12632,1.75);
#10557=CYLINDRICAL_SURFACE('',#12635,1.75);
#10558=CYLINDRICAL_SURFACE('',#12638,1.75);
#10559=CYLINDRICAL_SURFACE('',#12641,1.75);
#10560=CYLINDRICAL_SURFACE('',#12644,1.75);
#10561=CYLINDRICAL_SURFACE('',#12647,1.75);
#10562=CYLINDRICAL_SURFACE('',#12652,1.75);
#10563=CYLINDRICAL_SURFACE('',#12662,0.2);
#10564=CYLINDRICAL_SURFACE('',#12673,0.2);
#10565=CYLINDRICAL_SURFACE('',#12685,1.);
#10566=CYLINDRICAL_SURFACE('',#12691,1.01);
#10567=CYLINDRICAL_SURFACE('',#12694,1.35);
#10568=CYLINDRICAL_SURFACE('',#12700,1.01);
#10569=CYLINDRICAL_SURFACE('',#12703,1.35);
#10570=CYLINDRICAL_SURFACE('',#12711,0.21);
#10571=CYLINDRICAL_SURFACE('',#12715,1.005);
#10572=CYLINDRICAL_SURFACE('',#12718,1.6);
#10573=CYLINDRICAL_SURFACE('',#12724,1.01);
#10574=CYLINDRICAL_SURFACE('',#12727,1.35);
#10575=CYLINDRICAL_SURFACE('',#12735,0.21);
#10576=CYLINDRICAL_SURFACE('',#12739,1.005);
#10577=CYLINDRICAL_SURFACE('',#12742,1.6);
#10578=CYLINDRICAL_SURFACE('',#12748,1.01);
#10579=CYLINDRICAL_SURFACE('',#12751,1.35);
#10580=CYLINDRICAL_SURFACE('',#12802,1.);
#10581=CYLINDRICAL_SURFACE('',#12804,2.);
#10582=CYLINDRICAL_SURFACE('',#12809,3.75);
#10583=CYLINDRICAL_SURFACE('',#12812,3.75);
#10584=CYLINDRICAL_SURFACE('',#12815,3.75);
#10585=CYLINDRICAL_SURFACE('',#12818,3.75);
#10586=CYLINDRICAL_SURFACE('',#12821,3.75);
#10587=CYLINDRICAL_SURFACE('',#12824,3.75);
#10588=CYLINDRICAL_SURFACE('',#12827,3.75);
#10589=CYLINDRICAL_SURFACE('',#12830,3.75);
#10590=CYLINDRICAL_SURFACE('',#12833,3.75);
#10591=CYLINDRICAL_SURFACE('',#12836,3.75);
#10592=CYLINDRICAL_SURFACE('',#12839,3.75);
#10593=CYLINDRICAL_SURFACE('',#12842,3.75);
#10594=CYLINDRICAL_SURFACE('',#12845,3.75);
#10595=CYLINDRICAL_SURFACE('',#12848,3.75);
#10596=CYLINDRICAL_SURFACE('',#12851,3.75);
#10597=CYLINDRICAL_SURFACE('',#12854,3.75);
#10598=CYLINDRICAL_SURFACE('',#12857,3.75);
#10599=CYLINDRICAL_SURFACE('',#12860,3.75);
#10600=CYLINDRICAL_SURFACE('',#12863,3.75);
#10601=CYLINDRICAL_SURFACE('',#12866,3.75);
#10602=CYLINDRICAL_SURFACE('',#12869,3.75);
#10603=CYLINDRICAL_SURFACE('',#12872,3.75);
#10604=CYLINDRICAL_SURFACE('',#12875,3.75);
#10605=CYLINDRICAL_SURFACE('',#12878,3.75);
#10606=CYLINDRICAL_SURFACE('',#12881,3.75);
#10607=CYLINDRICAL_SURFACE('',#12884,3.75);
#10608=CYLINDRICAL_SURFACE('',#12887,3.75);
#10609=CYLINDRICAL_SURFACE('',#12890,3.75);
#10610=CYLINDRICAL_SURFACE('',#12893,3.75);
#10611=CYLINDRICAL_SURFACE('',#12896,3.75);
#10612=CYLINDRICAL_SURFACE('',#12899,3.75);
#10613=CYLINDRICAL_SURFACE('',#12902,3.75);
#10614=CYLINDRICAL_SURFACE('',#12905,3.75);
#10615=CYLINDRICAL_SURFACE('',#12908,3.75);
#10616=CYLINDRICAL_SURFACE('',#12911,3.75);
#10617=CYLINDRICAL_SURFACE('',#12914,3.75);
#10618=CYLINDRICAL_SURFACE('',#12917,3.75);
#10619=CYLINDRICAL_SURFACE('',#12920,3.75);
#10620=CYLINDRICAL_SURFACE('',#12923,3.75);
#10621=CYLINDRICAL_SURFACE('',#12928,3.75);
#10622=CYLINDRICAL_SURFACE('',#12952,0.24505);
#10623=ADVANCED_FACE('',(#1503),#10420,.F.);
#10624=ADVANCED_FACE('',(#1504),#10421,.F.);
#10625=ADVANCED_FACE('',(#1505),#10422,.F.);
#10626=ADVANCED_FACE('',(#1506),#10423,.F.);
#10627=ADVANCED_FACE('',(#1507),#1238,.T.);
#10628=ADVANCED_FACE('',(#1508),#1239,.T.);
#10629=ADVANCED_FACE('',(#1509),#1240,.T.);
#10630=ADVANCED_FACE('',(#1510),#1241,.T.);
#10631=ADVANCED_FACE('',(#1511,#1060,#1061,#1062,#1063),#1242,.T.);
#10632=ADVANCED_FACE('',(#1512,#1064,#1065,#1066,#1067),#1243,.F.);
#10633=ADVANCED_FACE('',(#1513),#10424,.F.);
#10634=ADVANCED_FACE('',(#1514),#10425,.F.);
#10635=ADVANCED_FACE('',(#1515),#10426,.F.);
#10636=ADVANCED_FACE('',(#1516),#10427,.F.);
#10637=ADVANCED_FACE('',(#1517),#10428,.F.);
#10638=ADVANCED_FACE('',(#1518),#10429,.F.);
#10639=ADVANCED_FACE('',(#1519),#10430,.F.);
#10640=ADVANCED_FACE('',(#1520,#1068),#1244,.F.);
#10641=ADVANCED_FACE('',(#1521),#10431,.F.);
#10642=ADVANCED_FACE('',(#1522,#1069),#1245,.F.);
#10643=ADVANCED_FACE('',(#1523),#10432,.F.);
#10644=ADVANCED_FACE('',(#1524,#1070),#1246,.F.);
#10645=ADVANCED_FACE('',(#1525),#10433,.F.);
#10646=ADVANCED_FACE('',(#1526,#1071),#1247,.F.);
#10647=ADVANCED_FACE('',(#1527),#10434,.F.);
#10648=ADVANCED_FACE('',(#1528),#10435,.F.);
#10649=ADVANCED_FACE('',(#1529),#10436,.F.);
#10650=ADVANCED_FACE('',(#1530),#10437,.F.);
#10651=ADVANCED_FACE('',(#1531),#10438,.F.);
#10652=ADVANCED_FACE('',(#1532),#1248,.F.);
#10653=ADVANCED_FACE('',(#1533),#10439,.F.);
#10654=ADVANCED_FACE('',(#1534),#1249,.F.);
#10655=ADVANCED_FACE('',(#1535),#10440,.F.);
#10656=ADVANCED_FACE('',(#1536,#1072),#1250,.F.);
#10657=ADVANCED_FACE('',(#1537),#10441,.F.);
#10658=ADVANCED_FACE('',(#1538),#10442,.F.);
#10659=ADVANCED_FACE('',(#1539,#1073),#1251,.F.);
#10660=ADVANCED_FACE('',(#1540),#10443,.F.);
#10661=ADVANCED_FACE('',(#1541,#1074,#1075,#1076,#1077,#1078,#1079,#1080,
#1081,#1082,#1083,#1084,#1085),#1252,.T.);
#10662=ADVANCED_FACE('',(#1542),#1253,.T.);
#10663=ADVANCED_FACE('',(#1543,#1086,#1087,#1088,#1089,#1090,#1091,#1092,
#1093,#1094,#1095,#1096,#1097),#1254,.T.);
#10664=ADVANCED_FACE('',(#1544),#1255,.T.);
#10665=ADVANCED_FACE('',(#1545),#1256,.T.);
#10666=ADVANCED_FACE('',(#1546,#1098,#1099),#1257,.F.);
#10667=ADVANCED_FACE('',(#1547),#10444,.F.);
#10668=ADVANCED_FACE('',(#1548),#10445,.F.);
#10669=ADVANCED_FACE('',(#1549),#10446,.F.);
#10670=ADVANCED_FACE('',(#1550),#10447,.F.);
#10671=ADVANCED_FACE('',(#1551),#10448,.F.);
#10672=ADVANCED_FACE('',(#1552),#10449,.F.);
#10673=ADVANCED_FACE('',(#1553),#10450,.F.);
#10674=ADVANCED_FACE('',(#1554,#1100),#1258,.T.);
#10675=ADVANCED_FACE('',(#1555),#10451,.F.);
#10676=ADVANCED_FACE('',(#1556,#1101),#1259,.T.);
#10677=ADVANCED_FACE('',(#1557),#10452,.F.);
#10678=ADVANCED_FACE('',(#1558,#1102),#1260,.T.);
#10679=ADVANCED_FACE('',(#1559),#10453,.F.);
#10680=ADVANCED_FACE('',(#1560,#1103),#1261,.T.);
#10681=ADVANCED_FACE('',(#1561),#10454,.F.);
#10682=ADVANCED_FACE('',(#1562),#10455,.F.);
#10683=ADVANCED_FACE('',(#1563),#10456,.F.);
#10684=ADVANCED_FACE('',(#1564),#10457,.F.);
#10685=ADVANCED_FACE('',(#1565),#10458,.F.);
#10686=ADVANCED_FACE('',(#1566),#1262,.F.);
#10687=ADVANCED_FACE('',(#1567),#10459,.F.);
#10688=ADVANCED_FACE('',(#1568),#1263,.F.);
#10689=ADVANCED_FACE('',(#1569),#10460,.F.);
#10690=ADVANCED_FACE('',(#1570,#1104),#1264,.T.);
#10691=ADVANCED_FACE('',(#1571),#10461,.F.);
#10692=ADVANCED_FACE('',(#1572),#10462,.F.);
#10693=ADVANCED_FACE('',(#1573,#1105),#1265,.T.);
#10694=ADVANCED_FACE('',(#1574),#10463,.F.);
#10695=ADVANCED_FACE('',(#1575,#1106,#1107,#1108,#1109,#1110,#1111,#1112,
#1113,#1114,#1115,#1116,#1117),#1266,.T.);
#10696=ADVANCED_FACE('',(#1576),#1267,.T.);
#10697=ADVANCED_FACE('',(#1577,#1118,#1119,#1120,#1121,#1122,#1123,#1124,
#1125,#1126,#1127,#1128,#1129),#1268,.T.);
#10698=ADVANCED_FACE('',(#1578),#1269,.T.);
#10699=ADVANCED_FACE('',(#1579),#1270,.T.);
#10700=ADVANCED_FACE('',(#1580,#1130,#1131),#1271,.F.);
#10701=ADVANCED_FACE('',(#1581),#10464,.F.);
#10702=ADVANCED_FACE('',(#1582),#10465,.T.);
#10703=ADVANCED_FACE('',(#1583,#1132),#1272,.T.);
#10704=ADVANCED_FACE('',(#1584,#1133),#1273,.F.);
#10705=ADVANCED_FACE('',(#1585),#10466,.F.);
#10706=ADVANCED_FACE('',(#1586),#10467,.T.);
#10707=ADVANCED_FACE('',(#1587,#1134),#1274,.T.);
#10708=ADVANCED_FACE('',(#1588,#1135),#1275,.F.);
#10709=ADVANCED_FACE('',(#1589),#10468,.F.);
#10710=ADVANCED_FACE('',(#1590),#10469,.T.);
#10711=ADVANCED_FACE('',(#1591,#1136),#1276,.T.);
#10712=ADVANCED_FACE('',(#1592,#1137),#1277,.F.);
#10713=ADVANCED_FACE('',(#1593),#10470,.F.);
#10714=ADVANCED_FACE('',(#1594),#10471,.T.);
#10715=ADVANCED_FACE('',(#1595,#1138),#1278,.T.);
#10716=ADVANCED_FACE('',(#1596,#1139),#1279,.F.);
#10717=ADVANCED_FACE('',(#1597),#10472,.F.);
#10718=ADVANCED_FACE('',(#1598),#10473,.F.);
#10719=ADVANCED_FACE('',(#1599),#10474,.F.);
#10720=ADVANCED_FACE('',(#1600),#10475,.T.);
#10721=ADVANCED_FACE('',(#1601,#1140),#1280,.T.);
#10722=ADVANCED_FACE('',(#1602),#10476,.F.);
#10723=ADVANCED_FACE('',(#1603),#10477,.T.);
#10724=ADVANCED_FACE('',(#1604,#1141,#1142,#1143,#1144),#1281,.T.);
#10725=ADVANCED_FACE('',(#1605,#1145,#1146,#1147,#1148),#1282,.F.);
#10726=ADVANCED_FACE('',(#1606),#10478,.F.);
#10727=ADVANCED_FACE('',(#1607),#10479,.F.);
#10728=ADVANCED_FACE('',(#1608),#10480,.F.);
#10729=ADVANCED_FACE('',(#1609),#10481,.T.);
#10730=ADVANCED_FACE('',(#1610,#1149),#1283,.T.);
#10731=ADVANCED_FACE('',(#1611),#10482,.F.);
#10732=ADVANCED_FACE('',(#1612),#10483,.T.);
#10733=ADVANCED_FACE('',(#1613,#1150,#1151,#1152,#1153),#1284,.T.);
#10734=ADVANCED_FACE('',(#1614,#1154,#1155,#1156,#1157),#1285,.F.);
#10735=ADVANCED_FACE('',(#1615),#10484,.F.);
#10736=ADVANCED_FACE('',(#1616),#10485,.F.);
#10737=ADVANCED_FACE('',(#1617),#10486,.F.);
#10738=ADVANCED_FACE('',(#1618),#10487,.T.);
#10739=ADVANCED_FACE('',(#1619,#1158),#1286,.F.);
#10740=ADVANCED_FACE('',(#1620),#10488,.F.);
#10741=ADVANCED_FACE('',(#1621),#10489,.T.);
#10742=ADVANCED_FACE('',(#1622,#1159,#1160,#1161,#1162),#1287,.T.);
#10743=ADVANCED_FACE('',(#1623,#1163,#1164,#1165,#1166),#1288,.F.);
#10744=ADVANCED_FACE('',(#1624),#10490,.F.);
#10745=ADVANCED_FACE('',(#1625),#10491,.F.);
#10746=ADVANCED_FACE('',(#1626),#10492,.F.);
#10747=ADVANCED_FACE('',(#1627),#10493,.T.);
#10748=ADVANCED_FACE('',(#1628,#1167),#1289,.F.);
#10749=ADVANCED_FACE('',(#1629),#10494,.F.);
#10750=ADVANCED_FACE('',(#1630),#10495,.T.);
#10751=ADVANCED_FACE('',(#1631,#1168,#1169,#1170,#1171),#1290,.T.);
#10752=ADVANCED_FACE('',(#1632,#1172,#1173,#1174,#1175),#1291,.F.);
#10753=ADVANCED_FACE('',(#1633),#1292,.T.);
#10754=ADVANCED_FACE('',(#1634),#832,.T.);
#10755=ADVANCED_FACE('',(#1635),#10496,.T.);
#10756=ADVANCED_FACE('',(#1636),#833,.T.);
#10757=ADVANCED_FACE('',(#1637,#1176),#1293,.T.);
#10758=ADVANCED_FACE('',(#1638),#834,.T.);
#10759=ADVANCED_FACE('',(#1639),#10497,.T.);
#10760=ADVANCED_FACE('',(#1640),#835,.T.);
#10761=ADVANCED_FACE('',(#1641),#1294,.T.);
#10762=ADVANCED_FACE('',(#1642),#1295,.F.);
#10763=ADVANCED_FACE('',(#1643),#1296,.F.);
#10764=ADVANCED_FACE('',(#1644),#1297,.F.);
#10765=ADVANCED_FACE('',(#1645),#1298,.F.);
#10766=ADVANCED_FACE('',(#1646),#1299,.F.);
#10767=ADVANCED_FACE('',(#1647),#1300,.F.);
#10768=ADVANCED_FACE('',(#1648),#1301,.F.);
#10769=ADVANCED_FACE('',(#1649),#1302,.F.);
#10770=ADVANCED_FACE('',(#1650),#1303,.T.);
#10771=ADVANCED_FACE('',(#1651),#836,.T.);
#10772=ADVANCED_FACE('',(#1652),#10498,.T.);
#10773=ADVANCED_FACE('',(#1653),#837,.T.);
#10774=ADVANCED_FACE('',(#1654,#1177),#1304,.T.);
#10775=ADVANCED_FACE('',(#1655),#838,.T.);
#10776=ADVANCED_FACE('',(#1656),#10499,.T.);
#10777=ADVANCED_FACE('',(#1657),#839,.T.);
#10778=ADVANCED_FACE('',(#1658),#1305,.T.);
#10779=ADVANCED_FACE('',(#1659),#1306,.F.);
#10780=ADVANCED_FACE('',(#1660),#1307,.F.);
#10781=ADVANCED_FACE('',(#1661),#1308,.F.);
#10782=ADVANCED_FACE('',(#1662),#1309,.F.);
#10783=ADVANCED_FACE('',(#1663),#1310,.F.);
#10784=ADVANCED_FACE('',(#1664),#1311,.F.);
#10785=ADVANCED_FACE('',(#1665),#1312,.F.);
#10786=ADVANCED_FACE('',(#1666),#1313,.F.);
#10787=ADVANCED_FACE('',(#1667),#825,.F.);
#10788=ADVANCED_FACE('',(#1668),#10500,.T.);
#10789=ADVANCED_FACE('',(#1669),#10501,.F.);
#10790=ADVANCED_FACE('',(#1670),#840,.F.);
#10791=ADVANCED_FACE('',(#1671,#1178),#1314,.T.);
#10792=ADVANCED_FACE('',(#1672),#10502,.T.);
#10793=ADVANCED_FACE('',(#1673,#1179),#1315,.T.);
#10794=ADVANCED_FACE('',(#1674),#841,.F.);
#10795=ADVANCED_FACE('',(#1675),#826,.F.);
#10796=ADVANCED_FACE('',(#1676),#10503,.F.);
#10797=ADVANCED_FACE('',(#1677,#1180),#1316,.T.);
#10798=ADVANCED_FACE('',(#1678),#842,.T.);
#10799=ADVANCED_FACE('',(#1679),#10504,.T.);
#10800=ADVANCED_FACE('',(#1680),#843,.T.);
#10801=ADVANCED_FACE('',(#1681,#1181),#1317,.T.);
#10802=ADVANCED_FACE('',(#1682),#10505,.F.);
#10803=ADVANCED_FACE('',(#1683),#795,.T.);
#10804=ADVANCED_FACE('',(#1684),#796,.T.);
#10805=ADVANCED_FACE('',(#1685),#797,.T.);
#10806=ADVANCED_FACE('',(#1686),#798,.T.);
#10807=ADVANCED_FACE('',(#1687),#799,.T.);
#10808=ADVANCED_FACE('',(#1688),#800,.T.);
#10809=ADVANCED_FACE('',(#1689),#801,.T.);
#10810=ADVANCED_FACE('',(#1690),#802,.F.);
#10811=ADVANCED_FACE('',(#1691),#10506,.T.);
#10812=ADVANCED_FACE('',(#1692),#1318,.T.);
#10813=ADVANCED_FACE('',(#1693),#803,.F.);
#10814=ADVANCED_FACE('',(#1694),#1319,.T.);
#10815=ADVANCED_FACE('',(#1695),#804,.F.);
#10816=ADVANCED_FACE('',(#1696),#1320,.T.);
#10817=ADVANCED_FACE('',(#1697),#805,.F.);
#10818=ADVANCED_FACE('',(#1698),#1321,.T.);
#10819=ADVANCED_FACE('',(#1699),#806,.F.);
#10820=ADVANCED_FACE('',(#1700),#1322,.T.);
#10821=ADVANCED_FACE('',(#1701),#807,.F.);
#10822=ADVANCED_FACE('',(#1702),#10507,.F.);
#10823=ADVANCED_FACE('',(#1703),#1323,.T.);
#10824=ADVANCED_FACE('',(#1704),#808,.F.);
#10825=ADVANCED_FACE('',(#1705,#1182),#1324,.T.);
#10826=ADVANCED_FACE('',(#1706),#1325,.T.);
#10827=ADVANCED_FACE('',(#1707,#1183),#1326,.T.);
#10828=ADVANCED_FACE('',(#1708),#10508,.T.);
#10829=ADVANCED_FACE('',(#1709,#1184),#1327,.T.);
#10830=ADVANCED_FACE('',(#1710),#10509,.F.);
#10831=ADVANCED_FACE('',(#1711,#1185),#1328,.T.);
#10832=ADVANCED_FACE('',(#1712),#10510,.T.);
#10833=ADVANCED_FACE('',(#1713,#1186),#1329,.T.);
#10834=ADVANCED_FACE('',(#1714),#10511,.F.);
#10835=ADVANCED_FACE('',(#1715),#827,.F.);
#10836=ADVANCED_FACE('',(#1716),#10512,.T.);
#10837=ADVANCED_FACE('',(#1717),#10513,.F.);
#10838=ADVANCED_FACE('',(#1718),#844,.F.);
#10839=ADVANCED_FACE('',(#1719,#1187),#1330,.T.);
#10840=ADVANCED_FACE('',(#1720),#10514,.T.);
#10841=ADVANCED_FACE('',(#1721,#1188),#1331,.T.);
#10842=ADVANCED_FACE('',(#1722),#845,.F.);
#10843=ADVANCED_FACE('',(#1723),#828,.F.);
#10844=ADVANCED_FACE('',(#1724),#10515,.F.);
#10845=ADVANCED_FACE('',(#1725,#1189),#1332,.T.);
#10846=ADVANCED_FACE('',(#1726),#846,.T.);
#10847=ADVANCED_FACE('',(#1727),#10516,.T.);
#10848=ADVANCED_FACE('',(#1728),#847,.T.);
#10849=ADVANCED_FACE('',(#1729,#1190),#1333,.T.);
#10850=ADVANCED_FACE('',(#1730),#10517,.F.);
#10851=ADVANCED_FACE('',(#1731),#809,.T.);
#10852=ADVANCED_FACE('',(#1732),#810,.T.);
#10853=ADVANCED_FACE('',(#1733),#811,.T.);
#10854=ADVANCED_FACE('',(#1734),#812,.T.);
#10855=ADVANCED_FACE('',(#1735),#813,.T.);
#10856=ADVANCED_FACE('',(#1736),#814,.T.);
#10857=ADVANCED_FACE('',(#1737),#815,.T.);
#10858=ADVANCED_FACE('',(#1738),#816,.T.);
#10859=ADVANCED_FACE('',(#1739),#817,.F.);
#10860=ADVANCED_FACE('',(#1740),#10518,.T.);
#10861=ADVANCED_FACE('',(#1741),#1334,.T.);
#10862=ADVANCED_FACE('',(#1742),#818,.F.);
#10863=ADVANCED_FACE('',(#1743),#1335,.T.);
#10864=ADVANCED_FACE('',(#1744),#819,.F.);
#10865=ADVANCED_FACE('',(#1745),#1336,.T.);
#10866=ADVANCED_FACE('',(#1746),#820,.F.);
#10867=ADVANCED_FACE('',(#1747),#1337,.T.);
#10868=ADVANCED_FACE('',(#1748),#821,.F.);
#10869=ADVANCED_FACE('',(#1749),#1338,.T.);
#10870=ADVANCED_FACE('',(#1750),#822,.F.);
#10871=ADVANCED_FACE('',(#1751),#1339,.T.);
#10872=ADVANCED_FACE('',(#1752),#823,.F.);
#10873=ADVANCED_FACE('',(#1753),#10519,.F.);
#10874=ADVANCED_FACE('',(#1754),#1340,.T.);
#10875=ADVANCED_FACE('',(#1755),#824,.F.);
#10876=ADVANCED_FACE('',(#1756,#1191),#1341,.T.);
#10877=ADVANCED_FACE('',(#1757),#1342,.T.);
#10878=ADVANCED_FACE('',(#1758,#1192),#1343,.T.);
#10879=ADVANCED_FACE('',(#1759),#10520,.T.);
#10880=ADVANCED_FACE('',(#1760,#1193),#1344,.T.);
#10881=ADVANCED_FACE('',(#1761),#10521,.F.);
#10882=ADVANCED_FACE('',(#1762,#1194),#1345,.T.);
#10883=ADVANCED_FACE('',(#1763),#10522,.T.);
#10884=ADVANCED_FACE('',(#1764,#1195),#1346,.T.);
#10885=ADVANCED_FACE('',(#1765),#10523,.F.);
#10886=ADVANCED_FACE('',(#1766),#1347,.T.);
#10887=ADVANCED_FACE('',(#1767),#848,.T.);
#10888=ADVANCED_FACE('',(#1768),#10524,.T.);
#10889=ADVANCED_FACE('',(#1769),#849,.T.);
#10890=ADVANCED_FACE('',(#1770,#1196),#1348,.T.);
#10891=ADVANCED_FACE('',(#1771),#850,.T.);
#10892=ADVANCED_FACE('',(#1772),#10525,.T.);
#10893=ADVANCED_FACE('',(#1773),#851,.T.);
#10894=ADVANCED_FACE('',(#1774),#1349,.T.);
#10895=ADVANCED_FACE('',(#1775),#1350,.F.);
#10896=ADVANCED_FACE('',(#1776),#1351,.F.);
#10897=ADVANCED_FACE('',(#1777),#1352,.F.);
#10898=ADVANCED_FACE('',(#1778),#1353,.F.);
#10899=ADVANCED_FACE('',(#1779),#1354,.F.);
#10900=ADVANCED_FACE('',(#1780),#1355,.F.);
#10901=ADVANCED_FACE('',(#1781),#1356,.F.);
#10902=ADVANCED_FACE('',(#1782),#1357,.F.);
#10903=ADVANCED_FACE('',(#1783),#1358,.F.);
#10904=ADVANCED_FACE('',(#1784),#1359,.T.);
#10905=ADVANCED_FACE('',(#1785),#1360,.F.);
#10906=ADVANCED_FACE('',(#1786),#1361,.F.);
#10907=ADVANCED_FACE('',(#1787),#1362,.F.);
#10908=ADVANCED_FACE('',(#1788,#1197),#10526,.T.);
#10909=ADVANCED_FACE('',(#1789),#1363,.T.);
#10910=ADVANCED_FACE('',(#1790),#1364,.F.);
#10911=ADVANCED_FACE('',(#1791),#10527,.F.);
#10912=ADVANCED_FACE('',(#1792),#10528,.T.);
#10913=ADVANCED_FACE('',(#1793,#1198),#1365,.T.);
#10914=ADVANCED_FACE('',(#1794,#1199),#1366,.F.);
#10915=ADVANCED_FACE('',(#1795),#10529,.F.);
#10916=ADVANCED_FACE('',(#1796),#10530,.T.);
#10917=ADVANCED_FACE('',(#1797,#1200),#1367,.T.);
#10918=ADVANCED_FACE('',(#1798,#1201),#1368,.F.);
#10919=ADVANCED_FACE('',(#1799),#1369,.T.);
#10920=ADVANCED_FACE('',(#1800),#10531,.F.);
#10921=ADVANCED_FACE('',(#1801),#1370,.T.);
#10922=ADVANCED_FACE('',(#1802,#1202),#10532,.F.);
#10923=ADVANCED_FACE('',(#1803,#1203),#10533,.T.);
#10924=ADVANCED_FACE('',(#1804,#1204),#1371,.T.);
#10925=ADVANCED_FACE('',(#1805,#1205),#1372,.F.);
#10926=ADVANCED_FACE('',(#1806),#10534,.F.);
#10927=ADVANCED_FACE('',(#1807),#10535,.T.);
#10928=ADVANCED_FACE('',(#1808,#1206),#1373,.T.);
#10929=ADVANCED_FACE('',(#1809,#1207),#1374,.F.);
#10930=ADVANCED_FACE('',(#1810),#1375,.T.);
#10931=ADVANCED_FACE('',(#1811),#10536,.F.);
#10932=ADVANCED_FACE('',(#1812),#1376,.T.);
#10933=ADVANCED_FACE('',(#1813,#1208),#10537,.F.);
#10934=ADVANCED_FACE('',(#1814,#1209),#10538,.T.);
#10935=ADVANCED_FACE('',(#1815,#1210),#1377,.T.);
#10936=ADVANCED_FACE('',(#1816,#1211),#1378,.F.);
#10937=ADVANCED_FACE('',(#1817),#10539,.F.);
#10938=ADVANCED_FACE('',(#1818),#10540,.T.);
#10939=ADVANCED_FACE('',(#1819,#1212),#1379,.T.);
#10940=ADVANCED_FACE('',(#1820,#1213),#1380,.F.);
#10941=ADVANCED_FACE('',(#1821),#1381,.F.);
#10942=ADVANCED_FACE('',(#1822),#1382,.F.);
#10943=ADVANCED_FACE('',(#1823),#1383,.F.);
#10944=ADVANCED_FACE('',(#1824,#1214),#1384,.F.);
#10945=ADVANCED_FACE('',(#1825),#10541,.F.);
#10946=ADVANCED_FACE('',(#1826),#10542,.T.);
#10947=ADVANCED_FACE('',(#1827,#1215),#1385,.T.);
#10948=ADVANCED_FACE('',(#1828),#11,.T.);
#10949=ADVANCED_FACE('',(#1829),#1386,.T.);
#10950=ADVANCED_FACE('',(#1830),#12,.T.);
#10951=ADVANCED_FACE('',(#1831),#10543,.T.);
#10952=ADVANCED_FACE('',(#1832),#13,.T.);
#10953=ADVANCED_FACE('',(#1833),#1387,.T.);
#10954=ADVANCED_FACE('',(#1834),#14,.T.);
#10955=ADVANCED_FACE('',(#1835),#10544,.T.);
#10956=ADVANCED_FACE('',(#1836),#15,.T.);
#10957=ADVANCED_FACE('',(#1837),#1388,.T.);
#10958=ADVANCED_FACE('',(#1838),#16,.T.);
#10959=ADVANCED_FACE('',(#1839),#10545,.T.);
#10960=ADVANCED_FACE('',(#1840),#17,.T.);
#10961=ADVANCED_FACE('',(#1841),#1389,.T.);
#10962=ADVANCED_FACE('',(#1842),#18,.T.);
#10963=ADVANCED_FACE('',(#1843),#10546,.T.);
#10964=ADVANCED_FACE('',(#1844),#19,.T.);
#10965=ADVANCED_FACE('',(#1845),#1390,.T.);
#10966=ADVANCED_FACE('',(#1846),#20,.T.);
#10967=ADVANCED_FACE('',(#1847),#10547,.T.);
#10968=ADVANCED_FACE('',(#1848),#21,.T.);
#10969=ADVANCED_FACE('',(#1849),#1391,.T.);
#10970=ADVANCED_FACE('',(#1850),#22,.T.);
#10971=ADVANCED_FACE('',(#1851),#10548,.T.);
#10972=ADVANCED_FACE('',(#1852),#23,.T.);
#10973=ADVANCED_FACE('',(#1853),#1392,.T.);
#10974=ADVANCED_FACE('',(#1854),#24,.T.);
#10975=ADVANCED_FACE('',(#1855),#10549,.T.);
#10976=ADVANCED_FACE('',(#1856),#25,.T.);
#10977=ADVANCED_FACE('',(#1857),#1393,.T.);
#10978=ADVANCED_FACE('',(#1858),#26,.T.);
#10979=ADVANCED_FACE('',(#1859),#10550,.T.);
#10980=ADVANCED_FACE('',(#1860),#27,.T.);
#10981=ADVANCED_FACE('',(#1861),#1394,.T.);
#10982=ADVANCED_FACE('',(#1862),#28,.T.);
#10983=ADVANCED_FACE('',(#1863),#10551,.T.);
#10984=ADVANCED_FACE('',(#1864),#29,.T.);
#10985=ADVANCED_FACE('',(#1865),#1395,.T.);
#10986=ADVANCED_FACE('',(#1866),#30,.T.);
#10987=ADVANCED_FACE('',(#1867),#10552,.T.);
#10988=ADVANCED_FACE('',(#1868),#31,.T.);
#10989=ADVANCED_FACE('',(#1869),#1396,.T.);
#10990=ADVANCED_FACE('',(#1870),#32,.T.);
#10991=ADVANCED_FACE('',(#1871),#10553,.T.);
#10992=ADVANCED_FACE('',(#1872),#33,.T.);
#10993=ADVANCED_FACE('',(#1873),#1397,.T.);
#10994=ADVANCED_FACE('',(#1874),#34,.T.);
#10995=ADVANCED_FACE('',(#1875),#10554,.T.);
#10996=ADVANCED_FACE('',(#1876),#35,.T.);
#10997=ADVANCED_FACE('',(#1877),#1398,.T.);
#10998=ADVANCED_FACE('',(#1878),#36,.T.);
#10999=ADVANCED_FACE('',(#1879),#10555,.T.);
#11000=ADVANCED_FACE('',(#1880),#37,.T.);
#11001=ADVANCED_FACE('',(#1881),#1399,.T.);
#11002=ADVANCED_FACE('',(#1882),#38,.T.);
#11003=ADVANCED_FACE('',(#1883),#10556,.T.);
#11004=ADVANCED_FACE('',(#1884),#39,.T.);
#11005=ADVANCED_FACE('',(#1885),#1400,.T.);
#11006=ADVANCED_FACE('',(#1886),#40,.T.);
#11007=ADVANCED_FACE('',(#1887),#10557,.T.);
#11008=ADVANCED_FACE('',(#1888),#41,.T.);
#11009=ADVANCED_FACE('',(#1889),#1401,.T.);
#11010=ADVANCED_FACE('',(#1890),#42,.T.);
#11011=ADVANCED_FACE('',(#1891),#10558,.T.);
#11012=ADVANCED_FACE('',(#1892),#43,.T.);
#11013=ADVANCED_FACE('',(#1893),#1402,.T.);
#11014=ADVANCED_FACE('',(#1894),#44,.T.);
#11015=ADVANCED_FACE('',(#1895),#10559,.T.);
#11016=ADVANCED_FACE('',(#1896),#45,.T.);
#11017=ADVANCED_FACE('',(#1897),#1403,.T.);
#11018=ADVANCED_FACE('',(#1898),#46,.T.);
#11019=ADVANCED_FACE('',(#1899),#10560,.T.);
#11020=ADVANCED_FACE('',(#1900),#47,.T.);
#11021=ADVANCED_FACE('',(#1901),#1404,.T.);
#11022=ADVANCED_FACE('',(#1902),#48,.T.);
#11023=ADVANCED_FACE('',(#1903),#10561,.T.);
#11024=ADVANCED_FACE('',(#1904),#49,.T.);
#11025=ADVANCED_FACE('',(#1905),#1405,.T.);
#11026=ADVANCED_FACE('',(#1906),#50,.T.);
#11027=ADVANCED_FACE('',(#1907,#1216),#1406,.T.);
#11028=ADVANCED_FACE('',(#1908),#10562,.T.);
#11029=ADVANCED_FACE('',(#1909),#1407,.T.);
#11030=ADVANCED_FACE('',(#1910),#852,.T.);
#11031=ADVANCED_FACE('',(#1911),#1408,.T.);
#11032=ADVANCED_FACE('',(#1912),#853,.T.);
#11033=ADVANCED_FACE('',(#1913),#10563,.T.);
#11034=ADVANCED_FACE('',(#1914),#1409,.T.);
#11035=ADVANCED_FACE('',(#1915),#1410,.T.);
#11036=ADVANCED_FACE('',(#1916),#1411,.T.);
#11037=ADVANCED_FACE('',(#1917),#854,.T.);
#11038=ADVANCED_FACE('',(#1918),#1412,.T.);
#11039=ADVANCED_FACE('',(#1919),#855,.T.);
#11040=ADVANCED_FACE('',(#1920),#10564,.T.);
#11041=ADVANCED_FACE('',(#1921),#1413,.F.);
#11042=ADVANCED_FACE('',(#1922),#1414,.T.);
#11043=ADVANCED_FACE('',(#1923),#1415,.F.);
#11044=ADVANCED_FACE('',(#1924),#1416,.T.);
#11045=ADVANCED_FACE('',(#1925),#1417,.F.);
#11046=ADVANCED_FACE('',(#1926),#1418,.F.);
#11047=ADVANCED_FACE('',(#1927),#1419,.F.);
#11048=ADVANCED_FACE('',(#1928,#1217),#10565,.T.);
#11049=ADVANCED_FACE('',(#1929),#1420,.T.);
#11050=ADVANCED_FACE('',(#1930),#1421,.F.);
#11051=ADVANCED_FACE('',(#1931),#10566,.F.);
#11052=ADVANCED_FACE('',(#1932),#10567,.T.);
#11053=ADVANCED_FACE('',(#1933,#1218),#1422,.T.);
#11054=ADVANCED_FACE('',(#1934,#1219),#1423,.F.);
#11055=ADVANCED_FACE('',(#1935),#10568,.F.);
#11056=ADVANCED_FACE('',(#1936),#10569,.T.);
#11057=ADVANCED_FACE('',(#1937,#1220),#1424,.T.);
#11058=ADVANCED_FACE('',(#1938,#1221),#1425,.F.);
#11059=ADVANCED_FACE('',(#1939),#1426,.T.);
#11060=ADVANCED_FACE('',(#1940),#10570,.F.);
#11061=ADVANCED_FACE('',(#1941),#1427,.T.);
#11062=ADVANCED_FACE('',(#1942,#1222),#10571,.F.);
#11063=ADVANCED_FACE('',(#1943,#1223),#10572,.T.);
#11064=ADVANCED_FACE('',(#1944,#1224),#1428,.T.);
#11065=ADVANCED_FACE('',(#1945,#1225),#1429,.F.);
#11066=ADVANCED_FACE('',(#1946),#10573,.F.);
#11067=ADVANCED_FACE('',(#1947),#10574,.T.);
#11068=ADVANCED_FACE('',(#1948,#1226),#1430,.T.);
#11069=ADVANCED_FACE('',(#1949,#1227),#1431,.F.);
#11070=ADVANCED_FACE('',(#1950),#1432,.T.);
#11071=ADVANCED_FACE('',(#1951),#10575,.F.);
#11072=ADVANCED_FACE('',(#1952),#1433,.T.);
#11073=ADVANCED_FACE('',(#1953,#1228),#10576,.F.);
#11074=ADVANCED_FACE('',(#1954,#1229),#10577,.T.);
#11075=ADVANCED_FACE('',(#1955,#1230),#1434,.T.);
#11076=ADVANCED_FACE('',(#1956,#1231),#1435,.F.);
#11077=ADVANCED_FACE('',(#1957),#10578,.F.);
#11078=ADVANCED_FACE('',(#1958),#10579,.T.);
#11079=ADVANCED_FACE('',(#1959,#1232),#1436,.T.);
#11080=ADVANCED_FACE('',(#1960,#1233),#1437,.F.);
#11081=ADVANCED_FACE('',(#1961),#1438,.F.);
#11082=ADVANCED_FACE('',(#1962),#1439,.F.);
#11083=ADVANCED_FACE('',(#1963),#1440,.F.);
#11084=ADVANCED_FACE('',(#1964,#1234),#1441,.F.);
#11085=ADVANCED_FACE('',(#1965),#10580,.F.);
#11086=ADVANCED_FACE('',(#1966),#10581,.T.);
#11087=ADVANCED_FACE('',(#1967,#1235),#1442,.T.);
#11088=ADVANCED_FACE('',(#1968),#51,.T.);
#11089=ADVANCED_FACE('',(#1969),#52,.T.);
#11090=ADVANCED_FACE('',(#1970),#1443,.T.);
#11091=ADVANCED_FACE('',(#1971),#10582,.T.);
#11092=ADVANCED_FACE('',(#1972),#53,.T.);
#11093=ADVANCED_FACE('',(#1973),#54,.T.);
#11094=ADVANCED_FACE('',(#1974),#1444,.T.);
#11095=ADVANCED_FACE('',(#1975),#10583,.T.);
#11096=ADVANCED_FACE('',(#1976),#55,.T.);
#11097=ADVANCED_FACE('',(#1977),#56,.T.);
#11098=ADVANCED_FACE('',(#1978),#1445,.T.);
#11099=ADVANCED_FACE('',(#1979),#10584,.T.);
#11100=ADVANCED_FACE('',(#1980),#57,.T.);
#11101=ADVANCED_FACE('',(#1981),#58,.T.);
#11102=ADVANCED_FACE('',(#1982),#1446,.T.);
#11103=ADVANCED_FACE('',(#1983),#10585,.T.);
#11104=ADVANCED_FACE('',(#1984),#59,.T.);
#11105=ADVANCED_FACE('',(#1985),#60,.T.);
#11106=ADVANCED_FACE('',(#1986),#1447,.T.);
#11107=ADVANCED_FACE('',(#1987),#10586,.T.);
#11108=ADVANCED_FACE('',(#1988),#61,.T.);
#11109=ADVANCED_FACE('',(#1989),#62,.T.);
#11110=ADVANCED_FACE('',(#1990),#1448,.T.);
#11111=ADVANCED_FACE('',(#1991),#10587,.T.);
#11112=ADVANCED_FACE('',(#1992),#63,.T.);
#11113=ADVANCED_FACE('',(#1993),#64,.T.);
#11114=ADVANCED_FACE('',(#1994),#1449,.T.);
#11115=ADVANCED_FACE('',(#1995),#10588,.T.);
#11116=ADVANCED_FACE('',(#1996),#65,.T.);
#11117=ADVANCED_FACE('',(#1997),#66,.T.);
#11118=ADVANCED_FACE('',(#1998),#1450,.T.);
#11119=ADVANCED_FACE('',(#1999),#10589,.T.);
#11120=ADVANCED_FACE('',(#2000),#67,.T.);
#11121=ADVANCED_FACE('',(#2001),#68,.T.);
#11122=ADVANCED_FACE('',(#2002),#1451,.T.);
#11123=ADVANCED_FACE('',(#2003),#10590,.T.);
#11124=ADVANCED_FACE('',(#2004),#69,.T.);
#11125=ADVANCED_FACE('',(#2005),#70,.T.);
#11126=ADVANCED_FACE('',(#2006),#1452,.T.);
#11127=ADVANCED_FACE('',(#2007),#10591,.T.);
#11128=ADVANCED_FACE('',(#2008),#71,.T.);
#11129=ADVANCED_FACE('',(#2009),#72,.T.);
#11130=ADVANCED_FACE('',(#2010),#1453,.T.);
#11131=ADVANCED_FACE('',(#2011),#10592,.T.);
#11132=ADVANCED_FACE('',(#2012),#73,.T.);
#11133=ADVANCED_FACE('',(#2013),#74,.T.);
#11134=ADVANCED_FACE('',(#2014),#1454,.T.);
#11135=ADVANCED_FACE('',(#2015),#10593,.T.);
#11136=ADVANCED_FACE('',(#2016),#75,.T.);
#11137=ADVANCED_FACE('',(#2017),#76,.T.);
#11138=ADVANCED_FACE('',(#2018),#1455,.T.);
#11139=ADVANCED_FACE('',(#2019),#10594,.T.);
#11140=ADVANCED_FACE('',(#2020),#77,.T.);
#11141=ADVANCED_FACE('',(#2021),#78,.T.);
#11142=ADVANCED_FACE('',(#2022),#1456,.T.);
#11143=ADVANCED_FACE('',(#2023),#10595,.T.);
#11144=ADVANCED_FACE('',(#2024),#79,.T.);
#11145=ADVANCED_FACE('',(#2025),#80,.T.);
#11146=ADVANCED_FACE('',(#2026),#1457,.T.);
#11147=ADVANCED_FACE('',(#2027),#10596,.T.);
#11148=ADVANCED_FACE('',(#2028),#81,.T.);
#11149=ADVANCED_FACE('',(#2029),#82,.T.);
#11150=ADVANCED_FACE('',(#2030),#1458,.T.);
#11151=ADVANCED_FACE('',(#2031),#10597,.T.);
#11152=ADVANCED_FACE('',(#2032),#83,.T.);
#11153=ADVANCED_FACE('',(#2033),#84,.T.);
#11154=ADVANCED_FACE('',(#2034),#1459,.T.);
#11155=ADVANCED_FACE('',(#2035),#10598,.T.);
#11156=ADVANCED_FACE('',(#2036),#85,.T.);
#11157=ADVANCED_FACE('',(#2037),#86,.T.);
#11158=ADVANCED_FACE('',(#2038),#1460,.T.);
#11159=ADVANCED_FACE('',(#2039),#10599,.T.);
#11160=ADVANCED_FACE('',(#2040),#87,.T.);
#11161=ADVANCED_FACE('',(#2041),#88,.T.);
#11162=ADVANCED_FACE('',(#2042),#1461,.T.);
#11163=ADVANCED_FACE('',(#2043),#10600,.T.);
#11164=ADVANCED_FACE('',(#2044),#89,.T.);
#11165=ADVANCED_FACE('',(#2045),#90,.T.);
#11166=ADVANCED_FACE('',(#2046),#1462,.T.);
#11167=ADVANCED_FACE('',(#2047),#10601,.T.);
#11168=ADVANCED_FACE('',(#2048),#91,.T.);
#11169=ADVANCED_FACE('',(#2049),#92,.T.);
#11170=ADVANCED_FACE('',(#2050),#1463,.T.);
#11171=ADVANCED_FACE('',(#2051),#10602,.T.);
#11172=ADVANCED_FACE('',(#2052),#93,.T.);
#11173=ADVANCED_FACE('',(#2053),#94,.T.);
#11174=ADVANCED_FACE('',(#2054),#1464,.T.);
#11175=ADVANCED_FACE('',(#2055),#10603,.T.);
#11176=ADVANCED_FACE('',(#2056),#95,.T.);
#11177=ADVANCED_FACE('',(#2057),#96,.T.);
#11178=ADVANCED_FACE('',(#2058),#1465,.T.);
#11179=ADVANCED_FACE('',(#2059),#10604,.T.);
#11180=ADVANCED_FACE('',(#2060),#97,.T.);
#11181=ADVANCED_FACE('',(#2061),#98,.T.);
#11182=ADVANCED_FACE('',(#2062),#1466,.T.);
#11183=ADVANCED_FACE('',(#2063),#10605,.T.);
#11184=ADVANCED_FACE('',(#2064),#99,.T.);
#11185=ADVANCED_FACE('',(#2065),#100,.T.);
#11186=ADVANCED_FACE('',(#2066),#1467,.T.);
#11187=ADVANCED_FACE('',(#2067),#10606,.T.);
#11188=ADVANCED_FACE('',(#2068),#101,.T.);
#11189=ADVANCED_FACE('',(#2069),#102,.T.);
#11190=ADVANCED_FACE('',(#2070),#1468,.T.);
#11191=ADVANCED_FACE('',(#2071),#10607,.T.);
#11192=ADVANCED_FACE('',(#2072),#103,.T.);
#11193=ADVANCED_FACE('',(#2073),#104,.T.);
#11194=ADVANCED_FACE('',(#2074),#1469,.T.);
#11195=ADVANCED_FACE('',(#2075),#10608,.T.);
#11196=ADVANCED_FACE('',(#2076),#105,.T.);
#11197=ADVANCED_FACE('',(#2077),#106,.T.);
#11198=ADVANCED_FACE('',(#2078),#1470,.T.);
#11199=ADVANCED_FACE('',(#2079),#10609,.T.);
#11200=ADVANCED_FACE('',(#2080),#107,.T.);
#11201=ADVANCED_FACE('',(#2081),#108,.T.);
#11202=ADVANCED_FACE('',(#2082),#1471,.T.);
#11203=ADVANCED_FACE('',(#2083),#10610,.T.);
#11204=ADVANCED_FACE('',(#2084),#109,.T.);
#11205=ADVANCED_FACE('',(#2085),#110,.T.);
#11206=ADVANCED_FACE('',(#2086),#1472,.T.);
#11207=ADVANCED_FACE('',(#2087),#10611,.T.);
#11208=ADVANCED_FACE('',(#2088),#111,.T.);
#11209=ADVANCED_FACE('',(#2089),#112,.T.);
#11210=ADVANCED_FACE('',(#2090),#1473,.T.);
#11211=ADVANCED_FACE('',(#2091),#10612,.T.);
#11212=ADVANCED_FACE('',(#2092),#113,.T.);
#11213=ADVANCED_FACE('',(#2093),#114,.T.);
#11214=ADVANCED_FACE('',(#2094),#1474,.T.);
#11215=ADVANCED_FACE('',(#2095),#10613,.T.);
#11216=ADVANCED_FACE('',(#2096),#115,.T.);
#11217=ADVANCED_FACE('',(#2097),#116,.T.);
#11218=ADVANCED_FACE('',(#2098),#1475,.T.);
#11219=ADVANCED_FACE('',(#2099),#10614,.T.);
#11220=ADVANCED_FACE('',(#2100),#117,.T.);
#11221=ADVANCED_FACE('',(#2101),#118,.T.);
#11222=ADVANCED_FACE('',(#2102),#1476,.T.);
#11223=ADVANCED_FACE('',(#2103),#10615,.T.);
#11224=ADVANCED_FACE('',(#2104),#119,.T.);
#11225=ADVANCED_FACE('',(#2105),#120,.T.);
#11226=ADVANCED_FACE('',(#2106),#1477,.T.);
#11227=ADVANCED_FACE('',(#2107),#10616,.T.);
#11228=ADVANCED_FACE('',(#2108),#121,.T.);
#11229=ADVANCED_FACE('',(#2109),#122,.T.);
#11230=ADVANCED_FACE('',(#2110),#1478,.T.);
#11231=ADVANCED_FACE('',(#2111),#10617,.T.);
#11232=ADVANCED_FACE('',(#2112),#123,.T.);
#11233=ADVANCED_FACE('',(#2113),#124,.T.);
#11234=ADVANCED_FACE('',(#2114),#1479,.T.);
#11235=ADVANCED_FACE('',(#2115),#10618,.T.);
#11236=ADVANCED_FACE('',(#2116),#125,.T.);
#11237=ADVANCED_FACE('',(#2117),#126,.T.);
#11238=ADVANCED_FACE('',(#2118),#1480,.T.);
#11239=ADVANCED_FACE('',(#2119),#10619,.T.);
#11240=ADVANCED_FACE('',(#2120),#127,.T.);
#11241=ADVANCED_FACE('',(#2121),#1481,.T.);
#11242=ADVANCED_FACE('',(#2122),#128,.T.);
#11243=ADVANCED_FACE('',(#2123),#10620,.T.);
#11244=ADVANCED_FACE('',(#2124),#129,.T.);
#11245=ADVANCED_FACE('',(#2125),#130,.T.);
#11246=ADVANCED_FACE('',(#2126),#1482,.T.);
#11247=ADVANCED_FACE('',(#2127,#1236),#1483,.T.);
#11248=ADVANCED_FACE('',(#2128),#10621,.T.);
#11249=ADVANCED_FACE('',(#2129),#1484,.F.);
#11250=ADVANCED_FACE('',(#2130),#1485,.T.);
#11251=ADVANCED_FACE('',(#2131),#1486,.T.);
#11252=ADVANCED_FACE('',(#2132),#1487,.T.);
#11253=ADVANCED_FACE('',(#2133),#1488,.T.);
#11254=ADVANCED_FACE('',(#2134),#1489,.T.);
#11255=ADVANCED_FACE('',(#2135),#1490,.F.);
#11256=ADVANCED_FACE('',(#2136),#1491,.T.);
#11257=ADVANCED_FACE('',(#2137),#1492,.T.);
#11258=ADVANCED_FACE('',(#2138),#1493,.T.);
#11259=ADVANCED_FACE('',(#2139),#1494,.F.);
#11260=ADVANCED_FACE('',(#2140),#1495,.F.);
#11261=ADVANCED_FACE('',(#2141),#1496,.F.);
#11262=ADVANCED_FACE('',(#2142),#1497,.F.);
#11263=ADVANCED_FACE('',(#2143),#1498,.F.);
#11264=ADVANCED_FACE('',(#2144),#1499,.F.);
#11265=ADVANCED_FACE('',(#2145),#1500,.F.);
#11266=ADVANCED_FACE('',(#2146,#1237),#1501,.T.);
#11267=ADVANCED_FACE('',(#2147),#856,.T.);
#11268=ADVANCED_FACE('',(#2148),#10622,.T.);
#11269=ADVANCED_FACE('',(#2149),#857,.T.);
#11270=ADVANCED_FACE('',(#2150),#1502,.T.);
#11271=CLOSED_SHELL('',(#10623,#10624,#10625,#10626,#10627,#10628,#10629,
#10630,#10631,#10632));
#11272=CLOSED_SHELL('',(#10633,#10634,#10635,#10636,#10637,#10638,#10639,
#10640,#10641,#10642,#10643,#10644,#10645,#10646,#10647,#10648,#10649,#10650,
#10651,#10652,#10653,#10654,#10655,#10656,#10657,#10658,#10659,#10660,#10661,
#10662,#10663,#10664,#10665,#10666));
#11273=CLOSED_SHELL('',(#10667,#10668,#10669,#10670,#10671,#10672,#10673,
#10674,#10675,#10676,#10677,#10678,#10679,#10680,#10681,#10682,#10683,#10684,
#10685,#10686,#10687,#10688,#10689,#10690,#10691,#10692,#10693,#10694,#10695,
#10696,#10697,#10698,#10699,#10700));
#11274=CLOSED_SHELL('',(#10701,#10702,#10703,#10704));
#11275=CLOSED_SHELL('',(#10705,#10706,#10707,#10708));
#11276=CLOSED_SHELL('',(#10709,#10710,#10711,#10712));
#11277=CLOSED_SHELL('',(#10713,#10714,#10715,#10716));
#11278=CLOSED_SHELL('',(#10717,#10718,#10719,#10720,#10721,#10722,#10723,
#10724,#10725));
#11279=CLOSED_SHELL('',(#10726,#10727,#10728,#10729,#10730,#10731,#10732,
#10733,#10734));
#11280=CLOSED_SHELL('',(#10735,#10736,#10737,#10738,#10739,#10740,#10741,
#10742,#10743));
#11281=CLOSED_SHELL('',(#10744,#10745,#10746,#10747,#10748,#10749,#10750,
#10751,#10752));
#11282=CLOSED_SHELL('',(#10753,#10754,#10755,#10756,#10757,#10758,#10759,
#10760,#10761));
#11283=CLOSED_SHELL('',(#10762,#10763,#10764,#10765,#10766,#10767,#10768,
#10769));
#11284=CLOSED_SHELL('',(#10770,#10771,#10772,#10773,#10774,#10775,#10776,
#10777,#10778));
#11285=CLOSED_SHELL('',(#10779,#10780,#10781,#10782,#10783,#10784,#10785,
#10786));
#11286=CLOSED_SHELL('',(#10787,#10788,#10789,#10790,#10791,#10792,#10793,
#10794));
#11287=CLOSED_SHELL('',(#10795,#10796,#10797,#10798,#10799,#10800,#10801,
#10802));
#11288=CLOSED_SHELL('',(#10803));
#11289=CLOSED_SHELL('',(#10804));
#11290=CLOSED_SHELL('',(#10805));
#11291=CLOSED_SHELL('',(#10806));
#11292=CLOSED_SHELL('',(#10807));
#11293=CLOSED_SHELL('',(#10808));
#11294=CLOSED_SHELL('',(#10809));
#11295=CLOSED_SHELL('',(#10810,#10811,#10812,#10813,#10814,#10815,#10816,
#10817,#10818,#10819,#10820,#10821,#10822,#10823,#10824,#10825,#10826));
#11296=CLOSED_SHELL('',(#10827,#10828,#10829,#10830));
#11297=CLOSED_SHELL('',(#10831,#10832,#10833,#10834));
#11298=CLOSED_SHELL('',(#10835,#10836,#10837,#10838,#10839,#10840,#10841,
#10842));
#11299=CLOSED_SHELL('',(#10843,#10844,#10845,#10846,#10847,#10848,#10849,
#10850));
#11300=CLOSED_SHELL('',(#10851));
#11301=CLOSED_SHELL('',(#10852));
#11302=CLOSED_SHELL('',(#10853));
#11303=CLOSED_SHELL('',(#10854));
#11304=CLOSED_SHELL('',(#10855));
#11305=CLOSED_SHELL('',(#10856));
#11306=CLOSED_SHELL('',(#10857));
#11307=CLOSED_SHELL('',(#10858));
#11308=CLOSED_SHELL('',(#10859,#10860,#10861,#10862,#10863,#10864,#10865,
#10866,#10867,#10868,#10869,#10870,#10871,#10872,#10873,#10874,#10875,#10876,
#10877));
#11309=CLOSED_SHELL('',(#10878,#10879,#10880,#10881));
#11310=CLOSED_SHELL('',(#10882,#10883,#10884,#10885));
#11311=CLOSED_SHELL('',(#10886,#10887,#10888,#10889,#10890,#10891,#10892,
#10893,#10894));
#11312=CLOSED_SHELL('',(#10895,#10896,#10897,#10898,#10899,#10900,#10901,
#10902));
#11313=CLOSED_SHELL('',(#10903,#10904,#10905,#10906,#10907,#10908,#10909,
#10910));
#11314=CLOSED_SHELL('',(#10911,#10912,#10913,#10914));
#11315=CLOSED_SHELL('',(#10915,#10916,#10917,#10918));
#11316=CLOSED_SHELL('',(#10919,#10920,#10921,#10922,#10923,#10924,#10925));
#11317=CLOSED_SHELL('',(#10926,#10927,#10928,#10929));
#11318=CLOSED_SHELL('',(#10930,#10931,#10932,#10933,#10934,#10935,#10936));
#11319=CLOSED_SHELL('',(#10937,#10938,#10939,#10940));
#11320=CLOSED_SHELL('',(#10941,#10942,#10943,#10944,#10945,#10946,#10947,
#10948,#10949,#10950,#10951,#10952,#10953,#10954,#10955,#10956,#10957,#10958,
#10959,#10960,#10961,#10962,#10963,#10964,#10965,#10966,#10967,#10968,#10969,
#10970,#10971,#10972,#10973,#10974,#10975,#10976,#10977,#10978,#10979,#10980,
#10981,#10982,#10983,#10984,#10985,#10986,#10987,#10988,#10989,#10990,#10991,
#10992,#10993,#10994,#10995,#10996,#10997,#10998,#10999,#11000,#11001,#11002,
#11003,#11004,#11005,#11006,#11007,#11008,#11009,#11010,#11011,#11012,#11013,
#11014,#11015,#11016,#11017,#11018,#11019,#11020,#11021,#11022,#11023,#11024,
#11025,#11026,#11027,#11028));
#11321=CLOSED_SHELL('',(#11029,#11030,#11031,#11032,#11033,#11034,#11035,
#11036,#11037,#11038,#11039,#11040,#11041,#11042));
#11322=CLOSED_SHELL('',(#11043,#11044,#11045,#11046,#11047,#11048,#11049,
#11050));
#11323=CLOSED_SHELL('',(#11051,#11052,#11053,#11054));
#11324=CLOSED_SHELL('',(#11055,#11056,#11057,#11058));
#11325=CLOSED_SHELL('',(#11059,#11060,#11061,#11062,#11063,#11064,#11065));
#11326=CLOSED_SHELL('',(#11066,#11067,#11068,#11069));
#11327=CLOSED_SHELL('',(#11070,#11071,#11072,#11073,#11074,#11075,#11076));
#11328=CLOSED_SHELL('',(#11077,#11078,#11079,#11080));
#11329=CLOSED_SHELL('',(#11081,#11082,#11083,#11084,#11085,#11086,#11087,
#11088,#11089,#11090,#11091,#11092,#11093,#11094,#11095,#11096,#11097,#11098,
#11099,#11100,#11101,#11102,#11103,#11104,#11105,#11106,#11107,#11108,#11109,
#11110,#11111,#11112,#11113,#11114,#11115,#11116,#11117,#11118,#11119,#11120,
#11121,#11122,#11123,#11124,#11125,#11126,#11127,#11128,#11129,#11130,#11131,
#11132,#11133,#11134,#11135,#11136,#11137,#11138,#11139,#11140,#11141,#11142,
#11143,#11144,#11145,#11146,#11147,#11148,#11149,#11150,#11151,#11152,#11153,
#11154,#11155,#11156,#11157,#11158,#11159,#11160,#11161,#11162,#11163,#11164,
#11165,#11166,#11167,#11168,#11169,#11170,#11171,#11172,#11173,#11174,#11175,
#11176,#11177,#11178,#11179,#11180,#11181,#11182,#11183,#11184,#11185,#11186,
#11187,#11188,#11189,#11190,#11191,#11192,#11193,#11194,#11195,#11196,#11197,
#11198,#11199,#11200,#11201,#11202,#11203,#11204,#11205,#11206,#11207,#11208,
#11209,#11210,#11211,#11212,#11213,#11214,#11215,#11216,#11217,#11218,#11219,
#11220,#11221,#11222,#11223,#11224,#11225,#11226,#11227,#11228,#11229,#11230,
#11231,#11232,#11233,#11234,#11235,#11236,#11237,#11238,#11239,#11240,#11241,
#11242,#11243,#11244,#11245,#11246,#11247,#11248));
#11330=CLOSED_SHELL('',(#11249,#11250,#11251,#11252,#11253,#11254,#11255,
#11256,#11257,#11258));
#11331=CLOSED_SHELL('',(#11259,#11260,#11261,#11262,#11263,#11264,#11265,
#11266,#11267,#11268,#11269,#11270));
#11332=DERIVED_UNIT_ELEMENT(#11418,1.);
#11333=DERIVED_UNIT_ELEMENT(#53911,-3.);
#11334=DERIVED_UNIT_ELEMENT(#11418,1.);
#11335=DERIVED_UNIT_ELEMENT(#53911,-3.);
#11336=DERIVED_UNIT_ELEMENT(#11418,1.);
#11337=DERIVED_UNIT_ELEMENT(#53911,-3.);
#11338=DERIVED_UNIT_ELEMENT(#11418,1.);
#11339=DERIVED_UNIT_ELEMENT(#53911,-3.);
#11340=DERIVED_UNIT_ELEMENT(#11418,1.);
#11341=DERIVED_UNIT_ELEMENT(#53911,-3.);
#11342=DERIVED_UNIT_ELEMENT(#11418,1.);
#11343=DERIVED_UNIT_ELEMENT(#53911,-3.);
#11344=DERIVED_UNIT_ELEMENT(#11418,1.);
#11345=DERIVED_UNIT_ELEMENT(#53911,-3.);
#11346=DERIVED_UNIT_ELEMENT(#11418,1.);
#11347=DERIVED_UNIT_ELEMENT(#53911,-3.);
#11348=DERIVED_UNIT_ELEMENT(#11418,1.);
#11349=DERIVED_UNIT_ELEMENT(#53911,-3.);
#11350=DERIVED_UNIT_ELEMENT(#11418,1.);
#11351=DERIVED_UNIT_ELEMENT(#53911,-3.);
#11352=DERIVED_UNIT_ELEMENT(#11418,1.);
#11353=DERIVED_UNIT_ELEMENT(#53911,-3.);
#11354=DERIVED_UNIT_ELEMENT(#11418,1.);
#11355=DERIVED_UNIT_ELEMENT(#53911,-3.);
#11356=DERIVED_UNIT_ELEMENT(#11418,1.);
#11357=DERIVED_UNIT_ELEMENT(#53911,-3.);
#11358=DERIVED_UNIT_ELEMENT(#11418,1.);
#11359=DERIVED_UNIT_ELEMENT(#53911,-3.);
#11360=DERIVED_UNIT_ELEMENT(#11418,1.);
#11361=DERIVED_UNIT_ELEMENT(#53911,-3.);
#11362=DERIVED_UNIT_ELEMENT(#11418,1.);
#11363=DERIVED_UNIT_ELEMENT(#53911,-3.);
#11364=DERIVED_UNIT_ELEMENT(#11418,1.);
#11365=DERIVED_UNIT_ELEMENT(#53911,-3.);
#11366=DERIVED_UNIT_ELEMENT(#11418,1.);
#11367=DERIVED_UNIT_ELEMENT(#53911,-3.);
#11368=DERIVED_UNIT_ELEMENT(#11418,1.);
#11369=DERIVED_UNIT_ELEMENT(#53911,-3.);
#11370=DERIVED_UNIT_ELEMENT(#11418,1.);
#11371=DERIVED_UNIT_ELEMENT(#53911,-3.);
#11372=DERIVED_UNIT_ELEMENT(#11418,1.);
#11373=DERIVED_UNIT_ELEMENT(#53911,-3.);
#11374=DERIVED_UNIT_ELEMENT(#11418,1.);
#11375=DERIVED_UNIT_ELEMENT(#53911,-3.);
#11376=DERIVED_UNIT_ELEMENT(#11418,1.);
#11377=DERIVED_UNIT_ELEMENT(#53911,-3.);
#11378=DERIVED_UNIT_ELEMENT(#11418,1.);
#11379=DERIVED_UNIT_ELEMENT(#53911,-3.);
#11380=DERIVED_UNIT_ELEMENT(#11418,1.);
#11381=DERIVED_UNIT_ELEMENT(#53911,-3.);
#11382=DERIVED_UNIT_ELEMENT(#11418,1.);
#11383=DERIVED_UNIT_ELEMENT(#53911,-3.);
#11384=DERIVED_UNIT_ELEMENT(#11418,1.);
#11385=DERIVED_UNIT_ELEMENT(#53911,-3.);
#11386=DERIVED_UNIT_ELEMENT(#11418,1.);
#11387=DERIVED_UNIT_ELEMENT(#53911,-3.);
#11388=DERIVED_UNIT_ELEMENT(#11418,1.);
#11389=DERIVED_UNIT_ELEMENT(#53911,-3.);
#11390=DERIVED_UNIT_ELEMENT(#11418,1.);
#11391=DERIVED_UNIT_ELEMENT(#53911,-3.);
#11392=DERIVED_UNIT_ELEMENT(#11418,1.);
#11393=DERIVED_UNIT_ELEMENT(#53911,-3.);
#11394=DERIVED_UNIT_ELEMENT(#11418,1.);
#11395=DERIVED_UNIT_ELEMENT(#53911,-3.);
#11396=DERIVED_UNIT_ELEMENT(#11418,1.);
#11397=DERIVED_UNIT_ELEMENT(#53911,-3.);
#11398=DERIVED_UNIT_ELEMENT(#11418,1.);
#11399=DERIVED_UNIT_ELEMENT(#53911,-3.);
#11400=DERIVED_UNIT_ELEMENT(#11418,1.);
#11401=DERIVED_UNIT_ELEMENT(#53911,-3.);
#11402=DERIVED_UNIT_ELEMENT(#11418,1.);
#11403=DERIVED_UNIT_ELEMENT(#53911,-3.);
#11404=DERIVED_UNIT_ELEMENT(#11418,1.);
#11405=DERIVED_UNIT_ELEMENT(#53911,-3.);
#11406=DERIVED_UNIT_ELEMENT(#11418,1.);
#11407=DERIVED_UNIT_ELEMENT(#53911,-3.);
#11408=DERIVED_UNIT_ELEMENT(#11418,1.);
#11409=DERIVED_UNIT_ELEMENT(#53911,-3.);
#11410=DERIVED_UNIT_ELEMENT(#11418,1.);
#11411=DERIVED_UNIT_ELEMENT(#53911,-3.);
#11412=DERIVED_UNIT_ELEMENT(#11418,1.);
#11413=DERIVED_UNIT_ELEMENT(#53911,-3.);
#11414=DERIVED_UNIT_ELEMENT(#11418,1.);
#11415=DERIVED_UNIT_ELEMENT(#53911,-3.);
#11416=DERIVED_UNIT_ELEMENT(#11418,1.);
#11417=DERIVED_UNIT_ELEMENT(#53911,-3.);
#11418=(
MASS_UNIT()
NAMED_UNIT(*)
SI_UNIT(.KILO.,.GRAM.)
);
#11419=DERIVED_UNIT((#11332,#11333));
#11420=DERIVED_UNIT((#11334,#11335));
#11421=DERIVED_UNIT((#11336,#11337));
#11422=DERIVED_UNIT((#11338,#11339));
#11423=DERIVED_UNIT((#11340,#11341));
#11424=DERIVED_UNIT((#11342,#11343));
#11425=DERIVED_UNIT((#11344,#11345));
#11426=DERIVED_UNIT((#11346,#11347));
#11427=DERIVED_UNIT((#11348,#11349));
#11428=DERIVED_UNIT((#11350,#11351));
#11429=DERIVED_UNIT((#11352,#11353));
#11430=DERIVED_UNIT((#11354,#11355));
#11431=DERIVED_UNIT((#11356,#11357));
#11432=DERIVED_UNIT((#11358,#11359));
#11433=DERIVED_UNIT((#11360,#11361));
#11434=DERIVED_UNIT((#11362,#11363));
#11435=DERIVED_UNIT((#11364,#11365));
#11436=DERIVED_UNIT((#11366,#11367));
#11437=DERIVED_UNIT((#11368,#11369));
#11438=DERIVED_UNIT((#11370,#11371));
#11439=DERIVED_UNIT((#11372,#11373));
#11440=DERIVED_UNIT((#11374,#11375));
#11441=DERIVED_UNIT((#11376,#11377));
#11442=DERIVED_UNIT((#11378,#11379));
#11443=DERIVED_UNIT((#11380,#11381));
#11444=DERIVED_UNIT((#11382,#11383));
#11445=DERIVED_UNIT((#11384,#11385));
#11446=DERIVED_UNIT((#11386,#11387));
#11447=DERIVED_UNIT((#11388,#11389));
#11448=DERIVED_UNIT((#11390,#11391));
#11449=DERIVED_UNIT((#11392,#11393));
#11450=DERIVED_UNIT((#11394,#11395));
#11451=DERIVED_UNIT((#11396,#11397));
#11452=DERIVED_UNIT((#11398,#11399));
#11453=DERIVED_UNIT((#11400,#11401));
#11454=DERIVED_UNIT((#11402,#11403));
#11455=DERIVED_UNIT((#11404,#11405));
#11456=DERIVED_UNIT((#11406,#11407));
#11457=DERIVED_UNIT((#11408,#11409));
#11458=DERIVED_UNIT((#11410,#11411));
#11459=DERIVED_UNIT((#11412,#11413));
#11460=DERIVED_UNIT((#11414,#11415));
#11461=DERIVED_UNIT((#11416,#11417));
#11462=MEASURE_REPRESENTATION_ITEM('density measure',
POSITIVE_RATIO_MEASURE(7850.),#11419);
#11463=MEASURE_REPRESENTATION_ITEM('density measure',
POSITIVE_RATIO_MEASURE(7850.),#11420);
#11464=MEASURE_REPRESENTATION_ITEM('density measure',
POSITIVE_RATIO_MEASURE(7850.),#11421);
#11465=MEASURE_REPRESENTATION_ITEM('density measure',
POSITIVE_RATIO_MEASURE(7850.),#11422);
#11466=MEASURE_REPRESENTATION_ITEM('density measure',
POSITIVE_RATIO_MEASURE(7850.),#11423);
#11467=MEASURE_REPRESENTATION_ITEM('density measure',
POSITIVE_RATIO_MEASURE(7850.),#11424);
#11468=MEASURE_REPRESENTATION_ITEM('density measure',
POSITIVE_RATIO_MEASURE(7850.),#11425);
#11469=MEASURE_REPRESENTATION_ITEM('density measure',
POSITIVE_RATIO_MEASURE(7850.),#11426);
#11470=MEASURE_REPRESENTATION_ITEM('density measure',
POSITIVE_RATIO_MEASURE(7850.),#11427);
#11471=MEASURE_REPRESENTATION_ITEM('density measure',
POSITIVE_RATIO_MEASURE(7850.),#11428);
#11472=MEASURE_REPRESENTATION_ITEM('density measure',
POSITIVE_RATIO_MEASURE(7850.),#11429);
#11473=MEASURE_REPRESENTATION_ITEM('density measure',
POSITIVE_RATIO_MEASURE(7850.),#11430);
#11474=MEASURE_REPRESENTATION_ITEM('density measure',
POSITIVE_RATIO_MEASURE(7850.),#11431);
#11475=MEASURE_REPRESENTATION_ITEM('density measure',
POSITIVE_RATIO_MEASURE(7850.),#11432);
#11476=MEASURE_REPRESENTATION_ITEM('density measure',
POSITIVE_RATIO_MEASURE(7850.),#11433);
#11477=MEASURE_REPRESENTATION_ITEM('density measure',
POSITIVE_RATIO_MEASURE(7850.),#11434);
#11478=MEASURE_REPRESENTATION_ITEM('density measure',
POSITIVE_RATIO_MEASURE(7850.),#11435);
#11479=MEASURE_REPRESENTATION_ITEM('density measure',
POSITIVE_RATIO_MEASURE(7850.),#11436);
#11480=MEASURE_REPRESENTATION_ITEM('density measure',
POSITIVE_RATIO_MEASURE(7850.),#11437);
#11481=MEASURE_REPRESENTATION_ITEM('density measure',
POSITIVE_RATIO_MEASURE(7850.),#11438);
#11482=MEASURE_REPRESENTATION_ITEM('density measure',
POSITIVE_RATIO_MEASURE(7850.),#11439);
#11483=MEASURE_REPRESENTATION_ITEM('density measure',
POSITIVE_RATIO_MEASURE(7850.),#11440);
#11484=MEASURE_REPRESENTATION_ITEM('density measure',
POSITIVE_RATIO_MEASURE(7850.),#11441);
#11485=MEASURE_REPRESENTATION_ITEM('density measure',
POSITIVE_RATIO_MEASURE(7850.),#11442);
#11486=MEASURE_REPRESENTATION_ITEM('density measure',
POSITIVE_RATIO_MEASURE(7850.),#11443);
#11487=MEASURE_REPRESENTATION_ITEM('density measure',
POSITIVE_RATIO_MEASURE(7850.),#11444);
#11488=MEASURE_REPRESENTATION_ITEM('density measure',
POSITIVE_RATIO_MEASURE(7850.),#11445);
#11489=MEASURE_REPRESENTATION_ITEM('density measure',
POSITIVE_RATIO_MEASURE(7850.),#11446);
#11490=MEASURE_REPRESENTATION_ITEM('density measure',
POSITIVE_RATIO_MEASURE(7850.),#11447);
#11491=MEASURE_REPRESENTATION_ITEM('density measure',
POSITIVE_RATIO_MEASURE(7850.),#11448);
#11492=MEASURE_REPRESENTATION_ITEM('density measure',
POSITIVE_RATIO_MEASURE(7850.),#11449);
#11493=MEASURE_REPRESENTATION_ITEM('density measure',
POSITIVE_RATIO_MEASURE(7850.),#11450);
#11494=MEASURE_REPRESENTATION_ITEM('density measure',
POSITIVE_RATIO_MEASURE(7850.),#11451);
#11495=MEASURE_REPRESENTATION_ITEM('density measure',
POSITIVE_RATIO_MEASURE(7850.),#11452);
#11496=MEASURE_REPRESENTATION_ITEM('density measure',
POSITIVE_RATIO_MEASURE(7850.),#11453);
#11497=MEASURE_REPRESENTATION_ITEM('density measure',
POSITIVE_RATIO_MEASURE(7850.),#11454);
#11498=MEASURE_REPRESENTATION_ITEM('density measure',
POSITIVE_RATIO_MEASURE(7850.),#11455);
#11499=MEASURE_REPRESENTATION_ITEM('density measure',
POSITIVE_RATIO_MEASURE(7850.),#11456);
#11500=MEASURE_REPRESENTATION_ITEM('density measure',
POSITIVE_RATIO_MEASURE(7850.),#11457);
#11501=MEASURE_REPRESENTATION_ITEM('density measure',
POSITIVE_RATIO_MEASURE(7850.),#11458);
#11502=MEASURE_REPRESENTATION_ITEM('density measure',
POSITIVE_RATIO_MEASURE(7850.),#11459);
#11503=MEASURE_REPRESENTATION_ITEM('density measure',
POSITIVE_RATIO_MEASURE(7850.),#11460);
#11504=MEASURE_REPRESENTATION_ITEM('density measure',
POSITIVE_RATIO_MEASURE(7850.),#11461);
#11505=PROPERTY_DEFINITION_REPRESENTATION(#11720,#11591);
#11506=PROPERTY_DEFINITION_REPRESENTATION(#11721,#11592);
#11507=PROPERTY_DEFINITION_REPRESENTATION(#11722,#11593);
#11508=PROPERTY_DEFINITION_REPRESENTATION(#11723,#11594);
#11509=PROPERTY_DEFINITION_REPRESENTATION(#11724,#11595);
#11510=PROPERTY_DEFINITION_REPRESENTATION(#11725,#11596);
#11511=PROPERTY_DEFINITION_REPRESENTATION(#11726,#11597);
#11512=PROPERTY_DEFINITION_REPRESENTATION(#11727,#11598);
#11513=PROPERTY_DEFINITION_REPRESENTATION(#11728,#11599);
#11514=PROPERTY_DEFINITION_REPRESENTATION(#11729,#11600);
#11515=PROPERTY_DEFINITION_REPRESENTATION(#11730,#11601);
#11516=PROPERTY_DEFINITION_REPRESENTATION(#11731,#11602);
#11517=PROPERTY_DEFINITION_REPRESENTATION(#11732,#11603);
#11518=PROPERTY_DEFINITION_REPRESENTATION(#11733,#11604);
#11519=PROPERTY_DEFINITION_REPRESENTATION(#11734,#11605);
#11520=PROPERTY_DEFINITION_REPRESENTATION(#11735,#11606);
#11521=PROPERTY_DEFINITION_REPRESENTATION(#11736,#11607);
#11522=PROPERTY_DEFINITION_REPRESENTATION(#11737,#11608);
#11523=PROPERTY_DEFINITION_REPRESENTATION(#11738,#11609);
#11524=PROPERTY_DEFINITION_REPRESENTATION(#11739,#11610);
#11525=PROPERTY_DEFINITION_REPRESENTATION(#11740,#11611);
#11526=PROPERTY_DEFINITION_REPRESENTATION(#11741,#11612);
#11527=PROPERTY_DEFINITION_REPRESENTATION(#11742,#11613);
#11528=PROPERTY_DEFINITION_REPRESENTATION(#11743,#11614);
#11529=PROPERTY_DEFINITION_REPRESENTATION(#11744,#11615);
#11530=PROPERTY_DEFINITION_REPRESENTATION(#11745,#11616);
#11531=PROPERTY_DEFINITION_REPRESENTATION(#11746,#11617);
#11532=PROPERTY_DEFINITION_REPRESENTATION(#11747,#11618);
#11533=PROPERTY_DEFINITION_REPRESENTATION(#11748,#11619);
#11534=PROPERTY_DEFINITION_REPRESENTATION(#11749,#11620);
#11535=PROPERTY_DEFINITION_REPRESENTATION(#11750,#11621);
#11536=PROPERTY_DEFINITION_REPRESENTATION(#11751,#11622);
#11537=PROPERTY_DEFINITION_REPRESENTATION(#11752,#11623);
#11538=PROPERTY_DEFINITION_REPRESENTATION(#11753,#11624);
#11539=PROPERTY_DEFINITION_REPRESENTATION(#11754,#11625);
#11540=PROPERTY_DEFINITION_REPRESENTATION(#11755,#11626);
#11541=PROPERTY_DEFINITION_REPRESENTATION(#11756,#11627);
#11542=PROPERTY_DEFINITION_REPRESENTATION(#11757,#11628);
#11543=PROPERTY_DEFINITION_REPRESENTATION(#11758,#11629);
#11544=PROPERTY_DEFINITION_REPRESENTATION(#11759,#11630);
#11545=PROPERTY_DEFINITION_REPRESENTATION(#11760,#11631);
#11546=PROPERTY_DEFINITION_REPRESENTATION(#11761,#11632);
#11547=PROPERTY_DEFINITION_REPRESENTATION(#11762,#11633);
#11548=PROPERTY_DEFINITION_REPRESENTATION(#11763,#11634);
#11549=PROPERTY_DEFINITION_REPRESENTATION(#11764,#11635);
#11550=PROPERTY_DEFINITION_REPRESENTATION(#11765,#11636);
#11551=PROPERTY_DEFINITION_REPRESENTATION(#11766,#11637);
#11552=PROPERTY_DEFINITION_REPRESENTATION(#11767,#11638);
#11553=PROPERTY_DEFINITION_REPRESENTATION(#11768,#11639);
#11554=PROPERTY_DEFINITION_REPRESENTATION(#11769,#11640);
#11555=PROPERTY_DEFINITION_REPRESENTATION(#11770,#11641);
#11556=PROPERTY_DEFINITION_REPRESENTATION(#11771,#11642);
#11557=PROPERTY_DEFINITION_REPRESENTATION(#11772,#11643);
#11558=PROPERTY_DEFINITION_REPRESENTATION(#11773,#11644);
#11559=PROPERTY_DEFINITION_REPRESENTATION(#11774,#11645);
#11560=PROPERTY_DEFINITION_REPRESENTATION(#11775,#11646);
#11561=PROPERTY_DEFINITION_REPRESENTATION(#11776,#11647);
#11562=PROPERTY_DEFINITION_REPRESENTATION(#11777,#11648);
#11563=PROPERTY_DEFINITION_REPRESENTATION(#11778,#11649);
#11564=PROPERTY_DEFINITION_REPRESENTATION(#11779,#11650);
#11565=PROPERTY_DEFINITION_REPRESENTATION(#11780,#11651);
#11566=PROPERTY_DEFINITION_REPRESENTATION(#11781,#11652);
#11567=PROPERTY_DEFINITION_REPRESENTATION(#11782,#11653);
#11568=PROPERTY_DEFINITION_REPRESENTATION(#11783,#11654);
#11569=PROPERTY_DEFINITION_REPRESENTATION(#11784,#11655);
#11570=PROPERTY_DEFINITION_REPRESENTATION(#11785,#11656);
#11571=PROPERTY_DEFINITION_REPRESENTATION(#11786,#11657);
#11572=PROPERTY_DEFINITION_REPRESENTATION(#11787,#11658);
#11573=PROPERTY_DEFINITION_REPRESENTATION(#11788,#11659);
#11574=PROPERTY_DEFINITION_REPRESENTATION(#11789,#11660);
#11575=PROPERTY_DEFINITION_REPRESENTATION(#11790,#11661);
#11576=PROPERTY_DEFINITION_REPRESENTATION(#11791,#11662);
#11577=PROPERTY_DEFINITION_REPRESENTATION(#11792,#11663);
#11578=PROPERTY_DEFINITION_REPRESENTATION(#11793,#11664);
#11579=PROPERTY_DEFINITION_REPRESENTATION(#11794,#11665);
#11580=PROPERTY_DEFINITION_REPRESENTATION(#11795,#11666);
#11581=PROPERTY_DEFINITION_REPRESENTATION(#11796,#11667);
#11582=PROPERTY_DEFINITION_REPRESENTATION(#11797,#11668);
#11583=PROPERTY_DEFINITION_REPRESENTATION(#11798,#11669);
#11584=PROPERTY_DEFINITION_REPRESENTATION(#11799,#11670);
#11585=PROPERTY_DEFINITION_REPRESENTATION(#11800,#11671);
#11586=PROPERTY_DEFINITION_REPRESENTATION(#11801,#11672);
#11587=PROPERTY_DEFINITION_REPRESENTATION(#11802,#11673);
#11588=PROPERTY_DEFINITION_REPRESENTATION(#11803,#11674);
#11589=PROPERTY_DEFINITION_REPRESENTATION(#11804,#11675);
#11590=PROPERTY_DEFINITION_REPRESENTATION(#11805,#11676);
#11591=REPRESENTATION('material name',(#11677),#53862);
#11592=REPRESENTATION('density',(#11462),#53862);
#11593=REPRESENTATION('material name',(#11678),#53863);
#11594=REPRESENTATION('density',(#11463),#53863);
#11595=REPRESENTATION('material name',(#11679),#53864);
#11596=REPRESENTATION('density',(#11464),#53864);
#11597=REPRESENTATION('material name',(#11680),#53865);
#11598=REPRESENTATION('density',(#11465),#53865);
#11599=REPRESENTATION('material name',(#11681),#53866);
#11600=REPRESENTATION('density',(#11466),#53866);
#11601=REPRESENTATION('material name',(#11682),#53867);
#11602=REPRESENTATION('density',(#11467),#53867);
#11603=REPRESENTATION('material name',(#11683),#53868);
#11604=REPRESENTATION('density',(#11468),#53868);
#11605=REPRESENTATION('material name',(#11684),#53869);
#11606=REPRESENTATION('density',(#11469),#53869);
#11607=REPRESENTATION('material name',(#11685),#53870);
#11608=REPRESENTATION('density',(#11470),#53870);
#11609=REPRESENTATION('material name',(#11686),#53871);
#11610=REPRESENTATION('density',(#11471),#53871);
#11611=REPRESENTATION('material name',(#11687),#53872);
#11612=REPRESENTATION('density',(#11472),#53872);
#11613=REPRESENTATION('material name',(#11688),#53873);
#11614=REPRESENTATION('density',(#11473),#53873);
#11615=REPRESENTATION('material name',(#11689),#53874);
#11616=REPRESENTATION('density',(#11474),#53874);
#11617=REPRESENTATION('material name',(#11690),#53876);
#11618=REPRESENTATION('density',(#11475),#53876);
#11619=REPRESENTATION('material name',(#11691),#53877);
#11620=REPRESENTATION('density',(#11476),#53877);
#11621=REPRESENTATION('material name',(#11692),#53878);
#11622=REPRESENTATION('density',(#11477),#53878);
#11623=REPRESENTATION('material name',(#11693),#53879);
#11624=REPRESENTATION('density',(#11478),#53879);
#11625=REPRESENTATION('material name',(#11694),#53880);
#11626=REPRESENTATION('density',(#11479),#53880);
#11627=REPRESENTATION('material name',(#11695),#53882);
#11628=REPRESENTATION('density',(#11480),#53882);
#11629=REPRESENTATION('material name',(#11696),#53883);
#11630=REPRESENTATION('density',(#11481),#53883);
#11631=REPRESENTATION('material name',(#11697),#53884);
#11632=REPRESENTATION('density',(#11482),#53884);
#11633=REPRESENTATION('material name',(#11698),#53885);
#11634=REPRESENTATION('density',(#11483),#53885);
#11635=REPRESENTATION('material name',(#11699),#53886);
#11636=REPRESENTATION('density',(#11484),#53886);
#11637=REPRESENTATION('material name',(#11700),#53887);
#11638=REPRESENTATION('density',(#11485),#53887);
#11639=REPRESENTATION('material name',(#11701),#53889);
#11640=REPRESENTATION('density',(#11486),#53889);
#11641=REPRESENTATION('material name',(#11702),#53890);
#11642=REPRESENTATION('density',(#11487),#53890);
#11643=REPRESENTATION('material name',(#11703),#53891);
#11644=REPRESENTATION('density',(#11488),#53891);
#11645=REPRESENTATION('material name',(#11704),#53892);
#11646=REPRESENTATION('density',(#11489),#53892);
#11647=REPRESENTATION('material name',(#11705),#53893);
#11648=REPRESENTATION('density',(#11490),#53893);
#11649=REPRESENTATION('material name',(#11706),#53894);
#11650=REPRESENTATION('density',(#11491),#53894);
#11651=REPRESENTATION('material name',(#11707),#53895);
#11652=REPRESENTATION('density',(#11492),#53895);
#11653=REPRESENTATION('material name',(#11708),#53896);
#11654=REPRESENTATION('density',(#11493),#53896);
#11655=REPRESENTATION('material name',(#11709),#53897);
#11656=REPRESENTATION('density',(#11494),#53897);
#11657=REPRESENTATION('material name',(#11710),#53899);
#11658=REPRESENTATION('density',(#11495),#53899);
#11659=REPRESENTATION('material name',(#11711),#53900);
#11660=REPRESENTATION('density',(#11496),#53900);
#11661=REPRESENTATION('material name',(#11712),#53901);
#11662=REPRESENTATION('density',(#11497),#53901);
#11663=REPRESENTATION('material name',(#11713),#53902);
#11664=REPRESENTATION('density',(#11498),#53902);
#11665=REPRESENTATION('material name',(#11714),#53903);
#11666=REPRESENTATION('density',(#11499),#53903);
#11667=REPRESENTATION('material name',(#11715),#53904);
#11668=REPRESENTATION('density',(#11500),#53904);
#11669=REPRESENTATION('material name',(#11716),#53905);
#11670=REPRESENTATION('density',(#11501),#53905);
#11671=REPRESENTATION('material name',(#11717),#53906);
#11672=REPRESENTATION('density',(#11502),#53906);
#11673=REPRESENTATION('material name',(#11718),#53907);
#11674=REPRESENTATION('density',(#11503),#53907);
#11675=REPRESENTATION('material name',(#11719),#53908);
#11676=REPRESENTATION('density',(#11504),#53908);
#11677=DESCRIPTIVE_REPRESENTATION_ITEM('Steel','Steel');
#11678=DESCRIPTIVE_REPRESENTATION_ITEM('Steel','Steel');
#11679=DESCRIPTIVE_REPRESENTATION_ITEM('Steel','Steel');
#11680=DESCRIPTIVE_REPRESENTATION_ITEM('Steel','Steel');
#11681=DESCRIPTIVE_REPRESENTATION_ITEM('Steel','Steel');
#11682=DESCRIPTIVE_REPRESENTATION_ITEM('Steel','Steel');
#11683=DESCRIPTIVE_REPRESENTATION_ITEM('Steel','Steel');
#11684=DESCRIPTIVE_REPRESENTATION_ITEM('Steel','Steel');
#11685=DESCRIPTIVE_REPRESENTATION_ITEM('Steel','Steel');
#11686=DESCRIPTIVE_REPRESENTATION_ITEM('Steel','Steel');
#11687=DESCRIPTIVE_REPRESENTATION_ITEM('Steel','Steel');
#11688=DESCRIPTIVE_REPRESENTATION_ITEM('Steel','Steel');
#11689=DESCRIPTIVE_REPRESENTATION_ITEM('Steel','Steel');
#11690=DESCRIPTIVE_REPRESENTATION_ITEM('Steel','Steel');
#11691=DESCRIPTIVE_REPRESENTATION_ITEM('Steel','Steel');
#11692=DESCRIPTIVE_REPRESENTATION_ITEM('Steel','Steel');
#11693=DESCRIPTIVE_REPRESENTATION_ITEM('Steel','Steel');
#11694=DESCRIPTIVE_REPRESENTATION_ITEM('Steel','Steel');
#11695=DESCRIPTIVE_REPRESENTATION_ITEM('Steel','Steel');
#11696=DESCRIPTIVE_REPRESENTATION_ITEM('Steel','Steel');
#11697=DESCRIPTIVE_REPRESENTATION_ITEM('Steel','Steel');
#11698=DESCRIPTIVE_REPRESENTATION_ITEM('Steel','Steel');
#11699=DESCRIPTIVE_REPRESENTATION_ITEM('Steel','Steel');
#11700=DESCRIPTIVE_REPRESENTATION_ITEM('Steel','Steel');
#11701=DESCRIPTIVE_REPRESENTATION_ITEM('Steel','Steel');
#11702=DESCRIPTIVE_REPRESENTATION_ITEM('Steel','Steel');
#11703=DESCRIPTIVE_REPRESENTATION_ITEM('Steel','Steel');
#11704=DESCRIPTIVE_REPRESENTATION_ITEM('Steel','Steel');
#11705=DESCRIPTIVE_REPRESENTATION_ITEM('Steel','Steel');
#11706=DESCRIPTIVE_REPRESENTATION_ITEM('Steel','Steel');
#11707=DESCRIPTIVE_REPRESENTATION_ITEM('Steel','Steel');
#11708=DESCRIPTIVE_REPRESENTATION_ITEM('Steel','Steel');
#11709=DESCRIPTIVE_REPRESENTATION_ITEM('Steel','Steel');
#11710=DESCRIPTIVE_REPRESENTATION_ITEM('Steel','Steel');
#11711=DESCRIPTIVE_REPRESENTATION_ITEM('Steel','Steel');
#11712=DESCRIPTIVE_REPRESENTATION_ITEM('Steel','Steel');
#11713=DESCRIPTIVE_REPRESENTATION_ITEM('Steel','Steel');
#11714=DESCRIPTIVE_REPRESENTATION_ITEM('Steel','Steel');
#11715=DESCRIPTIVE_REPRESENTATION_ITEM('Steel','Steel');
#11716=DESCRIPTIVE_REPRESENTATION_ITEM('Steel','Steel');
#11717=DESCRIPTIVE_REPRESENTATION_ITEM('Steel','Steel');
#11718=DESCRIPTIVE_REPRESENTATION_ITEM('Steel','Steel');
#11719=DESCRIPTIVE_REPRESENTATION_ITEM('Steel','Steel');
#11720=PROPERTY_DEFINITION('material property','material name',#54138);
#11721=PROPERTY_DEFINITION('material property','density of part',#54138);
#11722=PROPERTY_DEFINITION('material property','material name',#54139);
#11723=PROPERTY_DEFINITION('material property','density of part',#54139);
#11724=PROPERTY_DEFINITION('material property','material name',#54140);
#11725=PROPERTY_DEFINITION('material property','density of part',#54140);
#11726=PROPERTY_DEFINITION('material property','material name',#54141);
#11727=PROPERTY_DEFINITION('material property','density of part',#54141);
#11728=PROPERTY_DEFINITION('material property','material name',#54142);
#11729=PROPERTY_DEFINITION('material property','density of part',#54142);
#11730=PROPERTY_DEFINITION('material property','material name',#54143);
#11731=PROPERTY_DEFINITION('material property','density of part',#54143);
#11732=PROPERTY_DEFINITION('material property','material name',#54144);
#11733=PROPERTY_DEFINITION('material property','density of part',#54144);
#11734=PROPERTY_DEFINITION('material property','material name',#54145);
#11735=PROPERTY_DEFINITION('material property','density of part',#54145);
#11736=PROPERTY_DEFINITION('material property','material name',#54146);
#11737=PROPERTY_DEFINITION('material property','density of part',#54146);
#11738=PROPERTY_DEFINITION('material property','material name',#54147);
#11739=PROPERTY_DEFINITION('material property','density of part',#54147);
#11740=PROPERTY_DEFINITION('material property','material name',#54148);
#11741=PROPERTY_DEFINITION('material property','density of part',#54148);
#11742=PROPERTY_DEFINITION('material property','material name',#54149);
#11743=PROPERTY_DEFINITION('material property','density of part',#54149);
#11744=PROPERTY_DEFINITION('material property','material name',#54150);
#11745=PROPERTY_DEFINITION('material property','density of part',#54150);
#11746=PROPERTY_DEFINITION('material property','material name',#54152);
#11747=PROPERTY_DEFINITION('material property','density of part',#54152);
#11748=PROPERTY_DEFINITION('material property','material name',#54153);
#11749=PROPERTY_DEFINITION('material property','density of part',#54153);
#11750=PROPERTY_DEFINITION('material property','material name',#54154);
#11751=PROPERTY_DEFINITION('material property','density of part',#54154);
#11752=PROPERTY_DEFINITION('material property','material name',#54155);
#11753=PROPERTY_DEFINITION('material property','density of part',#54155);
#11754=PROPERTY_DEFINITION('material property','material name',#54156);
#11755=PROPERTY_DEFINITION('material property','density of part',#54156);
#11756=PROPERTY_DEFINITION('material property','material name',#54158);
#11757=PROPERTY_DEFINITION('material property','density of part',#54158);
#11758=PROPERTY_DEFINITION('material property','material name',#54159);
#11759=PROPERTY_DEFINITION('material property','density of part',#54159);
#11760=PROPERTY_DEFINITION('material property','material name',#54160);
#11761=PROPERTY_DEFINITION('material property','density of part',#54160);
#11762=PROPERTY_DEFINITION('material property','material name',#54161);
#11763=PROPERTY_DEFINITION('material property','density of part',#54161);
#11764=PROPERTY_DEFINITION('material property','material name',#54162);
#11765=PROPERTY_DEFINITION('material property','density of part',#54162);
#11766=PROPERTY_DEFINITION('material property','material name',#54163);
#11767=PROPERTY_DEFINITION('material property','density of part',#54163);
#11768=PROPERTY_DEFINITION('material property','material name',#54165);
#11769=PROPERTY_DEFINITION('material property','density of part',#54165);
#11770=PROPERTY_DEFINITION('material property','material name',#54166);
#11771=PROPERTY_DEFINITION('material property','density of part',#54166);
#11772=PROPERTY_DEFINITION('material property','material name',#54167);
#11773=PROPERTY_DEFINITION('material property','density of part',#54167);
#11774=PROPERTY_DEFINITION('material property','material name',#54168);
#11775=PROPERTY_DEFINITION('material property','density of part',#54168);
#11776=PROPERTY_DEFINITION('material property','material name',#54169);
#11777=PROPERTY_DEFINITION('material property','density of part',#54169);
#11778=PROPERTY_DEFINITION('material property','material name',#54170);
#11779=PROPERTY_DEFINITION('material property','density of part',#54170);
#11780=PROPERTY_DEFINITION('material property','material name',#54171);
#11781=PROPERTY_DEFINITION('material property','density of part',#54171);
#11782=PROPERTY_DEFINITION('material property','material name',#54172);
#11783=PROPERTY_DEFINITION('material property','density of part',#54172);
#11784=PROPERTY_DEFINITION('material property','material name',#54173);
#11785=PROPERTY_DEFINITION('material property','density of part',#54173);
#11786=PROPERTY_DEFINITION('material property','material name',#54175);
#11787=PROPERTY_DEFINITION('material property','density of part',#54175);
#11788=PROPERTY_DEFINITION('material property','material name',#54176);
#11789=PROPERTY_DEFINITION('material property','density of part',#54176);
#11790=PROPERTY_DEFINITION('material property','material name',#54177);
#11791=PROPERTY_DEFINITION('material property','density of part',#54177);
#11792=PROPERTY_DEFINITION('material property','material name',#54178);
#11793=PROPERTY_DEFINITION('material property','density of part',#54178);
#11794=PROPERTY_DEFINITION('material property','material name',#54179);
#11795=PROPERTY_DEFINITION('material property','density of part',#54179);
#11796=PROPERTY_DEFINITION('material property','material name',#54180);
#11797=PROPERTY_DEFINITION('material property','density of part',#54180);
#11798=PROPERTY_DEFINITION('material property','material name',#54181);
#11799=PROPERTY_DEFINITION('material property','density of part',#54181);
#11800=PROPERTY_DEFINITION('material property','material name',#54182);
#11801=PROPERTY_DEFINITION('material property','density of part',#54182);
#11802=PROPERTY_DEFINITION('material property','material name',#54183);
#11803=PROPERTY_DEFINITION('material property','density of part',#54183);
#11804=PROPERTY_DEFINITION('material property','material name',#54184);
#11805=PROPERTY_DEFINITION('material property','density of part',#54184);
#11806=AXIS2_PLACEMENT_3D('',#15975,#12982,#12983);
#11807=AXIS2_PLACEMENT_3D('',#15976,#12984,#12985);
#11808=AXIS2_PLACEMENT_3D('',#15977,#12986,#12987);
#11809=AXIS2_PLACEMENT_3D('',#15978,#12988,#12989);
#11810=AXIS2_PLACEMENT_3D('',#15980,#12990,#12991);
#11811=AXIS2_PLACEMENT_3D('',#15983,#12993,#12994);
#11812=AXIS2_PLACEMENT_3D('',#15984,#12995,#12996);
#11813=AXIS2_PLACEMENT_3D('',#15986,#12997,#12998);
#11814=AXIS2_PLACEMENT_3D('',#15989,#13000,#13001);
#11815=AXIS2_PLACEMENT_3D('',#15990,#13002,#13003);
#11816=AXIS2_PLACEMENT_3D('',#15992,#13004,#13005);
#11817=AXIS2_PLACEMENT_3D('',#15995,#13007,#13008);
#11818=AXIS2_PLACEMENT_3D('',#15996,#13009,#13010);
#11819=AXIS2_PLACEMENT_3D('',#15998,#13011,#13012);
#11820=AXIS2_PLACEMENT_3D('',#16001,#13014,#13015);
#11821=AXIS2_PLACEMENT_3D('',#16002,#13016,#13017);
#11822=AXIS2_PLACEMENT_3D('',#16011,#13022,#13023);
#11823=AXIS2_PLACEMENT_3D('',#16017,#13027,#13028);
#11824=AXIS2_PLACEMENT_3D('',#16023,#13032,#13033);
#11825=AXIS2_PLACEMENT_3D('',#16026,#13036,#13037);
#11826=AXIS2_PLACEMENT_3D('',#16027,#13038,#13039);
#11827=AXIS2_PLACEMENT_3D('',#16028,#13040,#13041);
#11828=AXIS2_PLACEMENT_3D('',#16029,#13042,#13043);
#11829=AXIS2_PLACEMENT_3D('',#16031,#13044,#13045);
#11830=AXIS2_PLACEMENT_3D('',#16034,#13047,#13048);
#11831=AXIS2_PLACEMENT_3D('',#16035,#13049,#13050);
#11832=AXIS2_PLACEMENT_3D('',#16037,#13051,#13052);
#11833=AXIS2_PLACEMENT_3D('',#16040,#13054,#13055);
#11834=AXIS2_PLACEMENT_3D('',#16041,#13056,#13057);
#11835=AXIS2_PLACEMENT_3D('',#16043,#13058,#13059);
#11836=AXIS2_PLACEMENT_3D('',#16046,#13061,#13062);
#11837=AXIS2_PLACEMENT_3D('',#16047,#13063,#13064);
#11838=AXIS2_PLACEMENT_3D('',#16049,#13065,#13066);
#11839=AXIS2_PLACEMENT_3D('',#16052,#13068,#13069);
#11840=AXIS2_PLACEMENT_3D('',#16053,#13070,#13071);
#11841=AXIS2_PLACEMENT_3D('',#16055,#13072,#13073);
#11842=AXIS2_PLACEMENT_3D('',#16058,#13075,#13076);
#11843=AXIS2_PLACEMENT_3D('',#16059,#13077,#13078);
#11844=AXIS2_PLACEMENT_3D('',#16061,#13079,#13080);
#11845=AXIS2_PLACEMENT_3D('',#16064,#13082,#13083);
#11846=AXIS2_PLACEMENT_3D('',#16065,#13084,#13085);
#11847=AXIS2_PLACEMENT_3D('',#16067,#13086,#13087);
#11848=AXIS2_PLACEMENT_3D('',#16070,#13089,#13090);
#11849=AXIS2_PLACEMENT_3D('',#16071,#13091,#13092);
#11850=AXIS2_PLACEMENT_3D('',#16073,#13093,#13094);
#11851=AXIS2_PLACEMENT_3D('',#16074,#13095,#13096);
#11852=AXIS2_PLACEMENT_3D('',#16076,#13097,#13098);
#11853=AXIS2_PLACEMENT_3D('',#16079,#13100,#13101);
#11854=AXIS2_PLACEMENT_3D('',#16080,#13102,#13103);
#11855=AXIS2_PLACEMENT_3D('',#16082,#13104,#13105);
#11856=AXIS2_PLACEMENT_3D('',#16083,#13106,#13107);
#11857=AXIS2_PLACEMENT_3D('',#16085,#13108,#13109);
#11858=AXIS2_PLACEMENT_3D('',#16088,#13111,#13112);
#11859=AXIS2_PLACEMENT_3D('',#16089,#13113,#13114);
#11860=AXIS2_PLACEMENT_3D('',#16091,#13115,#13116);
#11861=AXIS2_PLACEMENT_3D('',#16092,#13117,#13118);
#11862=AXIS2_PLACEMENT_3D('',#16094,#13119,#13120);
#11863=AXIS2_PLACEMENT_3D('',#16097,#13122,#13123);
#11864=AXIS2_PLACEMENT_3D('',#16098,#13124,#13125);
#11865=AXIS2_PLACEMENT_3D('',#16100,#13126,#13127);
#11866=AXIS2_PLACEMENT_3D('',#16101,#13128,#13129);
#11867=AXIS2_PLACEMENT_3D('',#16104,#13131,#13132);
#11868=AXIS2_PLACEMENT_3D('',#16105,#13133,#13134);
#11869=AXIS2_PLACEMENT_3D('',#16108,#13136,#13137);
#11870=AXIS2_PLACEMENT_3D('',#16109,#13138,#13139);
#11871=AXIS2_PLACEMENT_3D('',#16112,#13141,#13142);
#11872=AXIS2_PLACEMENT_3D('',#16113,#13143,#13144);
#11873=AXIS2_PLACEMENT_3D('',#16116,#13146,#13147);
#11874=AXIS2_PLACEMENT_3D('',#16117,#13148,#13149);
#11875=AXIS2_PLACEMENT_3D('',#16119,#13150,#13151);
#11876=AXIS2_PLACEMENT_3D('',#16122,#13153,#13154);
#11877=AXIS2_PLACEMENT_3D('',#16123,#13155,#13156);
#11878=AXIS2_PLACEMENT_3D('',#16124,#13157,#13158);
#11879=AXIS2_PLACEMENT_3D('',#16126,#13159,#13160);
#11880=AXIS2_PLACEMENT_3D('',#16129,#13162,#13163);
#11881=AXIS2_PLACEMENT_3D('',#16130,#13164,#13165);
#11882=AXIS2_PLACEMENT_3D('',#16131,#13166,#13167);
#11883=AXIS2_PLACEMENT_3D('',#16133,#13168,#13169);
#11884=AXIS2_PLACEMENT_3D('',#16136,#13171,#13172);
#11885=AXIS2_PLACEMENT_3D('',#16137,#13173,#13174);
#11886=AXIS2_PLACEMENT_3D('',#16139,#13175,#13176);
#11887=AXIS2_PLACEMENT_3D('',#16140,#13177,#13178);
#11888=AXIS2_PLACEMENT_3D('',#16143,#13180,#13181);
#11889=AXIS2_PLACEMENT_3D('',#16144,#13182,#13183);
#11890=AXIS2_PLACEMENT_3D('',#16146,#13184,#13185);
#11891=AXIS2_PLACEMENT_3D('',#16149,#13187,#13188);
#11892=AXIS2_PLACEMENT_3D('',#16150,#13189,#13190);
#11893=AXIS2_PLACEMENT_3D('',#16152,#13191,#13192);
#11894=AXIS2_PLACEMENT_3D('',#16153,#13193,#13194);
#11895=AXIS2_PLACEMENT_3D('',#16156,#13196,#13197);
#11896=AXIS2_PLACEMENT_3D('',#16157,#13198,#13199);
#11897=AXIS2_PLACEMENT_3D('',#16166,#13204,#13205);
#11898=AXIS2_PLACEMENT_3D('',#16172,#13209,#13210);
#11899=AXIS2_PLACEMENT_3D('',#16178,#13214,#13215);
#11900=AXIS2_PLACEMENT_3D('',#16181,#13218,#13219);
#11901=AXIS2_PLACEMENT_3D('',#16182,#13220,#13221);
#11902=AXIS2_PLACEMENT_3D('',#16183,#13222,#13223);
#11903=AXIS2_PLACEMENT_3D('',#16184,#13224,#13225);
#11904=AXIS2_PLACEMENT_3D('',#16186,#13226,#13227);
#11905=AXIS2_PLACEMENT_3D('',#16189,#13229,#13230);
#11906=AXIS2_PLACEMENT_3D('',#16190,#13231,#13232);
#11907=AXIS2_PLACEMENT_3D('',#16192,#13233,#13234);
#11908=AXIS2_PLACEMENT_3D('',#16195,#13236,#13237);
#11909=AXIS2_PLACEMENT_3D('',#16196,#13238,#13239);
#11910=AXIS2_PLACEMENT_3D('',#16198,#13240,#13241);
#11911=AXIS2_PLACEMENT_3D('',#16201,#13243,#13244);
#11912=AXIS2_PLACEMENT_3D('',#16202,#13245,#13246);
#11913=AXIS2_PLACEMENT_3D('',#16204,#13247,#13248);
#11914=AXIS2_PLACEMENT_3D('',#16207,#13250,#13251);
#11915=AXIS2_PLACEMENT_3D('',#16208,#13252,#13253);
#11916=AXIS2_PLACEMENT_3D('',#16210,#13254,#13255);
#11917=AXIS2_PLACEMENT_3D('',#16213,#13257,#13258);
#11918=AXIS2_PLACEMENT_3D('',#16214,#13259,#13260);
#11919=AXIS2_PLACEMENT_3D('',#16216,#13261,#13262);
#11920=AXIS2_PLACEMENT_3D('',#16219,#13264,#13265);
#11921=AXIS2_PLACEMENT_3D('',#16220,#13266,#13267);
#11922=AXIS2_PLACEMENT_3D('',#16222,#13268,#13269);
#11923=AXIS2_PLACEMENT_3D('',#16225,#13271,#13272);
#11924=AXIS2_PLACEMENT_3D('',#16226,#13273,#13274);
#11925=AXIS2_PLACEMENT_3D('',#16228,#13275,#13276);
#11926=AXIS2_PLACEMENT_3D('',#16229,#13277,#13278);
#11927=AXIS2_PLACEMENT_3D('',#16231,#13279,#13280);
#11928=AXIS2_PLACEMENT_3D('',#16234,#13282,#13283);
#11929=AXIS2_PLACEMENT_3D('',#16235,#13284,#13285);
#11930=AXIS2_PLACEMENT_3D('',#16237,#13286,#13287);
#11931=AXIS2_PLACEMENT_3D('',#16238,#13288,#13289);
#11932=AXIS2_PLACEMENT_3D('',#16240,#13290,#13291);
#11933=AXIS2_PLACEMENT_3D('',#16243,#13293,#13294);
#11934=AXIS2_PLACEMENT_3D('',#16244,#13295,#13296);
#11935=AXIS2_PLACEMENT_3D('',#16246,#13297,#13298);
#11936=AXIS2_PLACEMENT_3D('',#16247,#13299,#13300);
#11937=AXIS2_PLACEMENT_3D('',#16249,#13301,#13302);
#11938=AXIS2_PLACEMENT_3D('',#16252,#13304,#13305);
#11939=AXIS2_PLACEMENT_3D('',#16253,#13306,#13307);
#11940=AXIS2_PLACEMENT_3D('',#16255,#13308,#13309);
#11941=AXIS2_PLACEMENT_3D('',#16256,#13310,#13311);
#11942=AXIS2_PLACEMENT_3D('',#16258,#13312,#13313);
#11943=AXIS2_PLACEMENT_3D('',#16260,#13315,#13316);
#11944=AXIS2_PLACEMENT_3D('',#16262,#13317,#13318);
#11945=AXIS2_PLACEMENT_3D('',#16264,#13320,#13321);
#11946=AXIS2_PLACEMENT_3D('',#16266,#13322,#13323);
#11947=AXIS2_PLACEMENT_3D('',#16268,#13325,#13326);
#11948=AXIS2_PLACEMENT_3D('',#16270,#13327,#13328);
#11949=AXIS2_PLACEMENT_3D('',#16272,#13330,#13331);
#11950=AXIS2_PLACEMENT_3D('',#16274,#13332,#13333);
#11951=AXIS2_PLACEMENT_3D('',#16277,#13335,#13336);
#11952=AXIS2_PLACEMENT_3D('',#16278,#13337,#13338);
#11953=AXIS2_PLACEMENT_3D('',#16279,#13339,#13340);
#11954=AXIS2_PLACEMENT_3D('',#16281,#13341,#13342);
#11955=AXIS2_PLACEMENT_3D('',#16284,#13344,#13345);
#11956=AXIS2_PLACEMENT_3D('',#16285,#13346,#13347);
#11957=AXIS2_PLACEMENT_3D('',#16286,#13348,#13349);
#11958=AXIS2_PLACEMENT_3D('',#16288,#13350,#13351);
#11959=AXIS2_PLACEMENT_3D('',#16291,#13353,#13354);
#11960=AXIS2_PLACEMENT_3D('',#16292,#13355,#13356);
#11961=AXIS2_PLACEMENT_3D('',#16294,#13357,#13358);
#11962=AXIS2_PLACEMENT_3D('',#16295,#13359,#13360);
#11963=AXIS2_PLACEMENT_3D('',#16297,#13361,#13362);
#11964=AXIS2_PLACEMENT_3D('',#16299,#13364,#13365);
#11965=AXIS2_PLACEMENT_3D('',#16301,#13366,#13367);
#11966=AXIS2_PLACEMENT_3D('',#16304,#13369,#13370);
#11967=AXIS2_PLACEMENT_3D('',#16305,#13371,#13372);
#11968=AXIS2_PLACEMENT_3D('',#16307,#13373,#13374);
#11969=AXIS2_PLACEMENT_3D('',#16308,#13375,#13376);
#11970=AXIS2_PLACEMENT_3D('',#16310,#13377,#13378);
#11971=AXIS2_PLACEMENT_3D('',#16312,#13380,#13381);
#11972=AXIS2_PLACEMENT_3D('',#16321,#13386,#13387);
#11973=AXIS2_PLACEMENT_3D('',#16327,#13391,#13392);
#11974=AXIS2_PLACEMENT_3D('',#16333,#13396,#13397);
#11975=AXIS2_PLACEMENT_3D('',#16336,#13400,#13401);
#11976=AXIS2_PLACEMENT_3D('',#16337,#13402,#13403);
#11977=AXIS2_PLACEMENT_3D('',#16338,#13404,#13405);
#11978=AXIS2_PLACEMENT_3D('',#16339,#13406,#13407);
#11979=AXIS2_PLACEMENT_3D('',#16341,#13408,#13409);
#11980=AXIS2_PLACEMENT_3D('',#16344,#13411,#13412);
#11981=AXIS2_PLACEMENT_3D('',#16345,#13413,#13414);
#11982=AXIS2_PLACEMENT_3D('',#16347,#13415,#13416);
#11983=AXIS2_PLACEMENT_3D('',#16350,#13418,#13419);
#11984=AXIS2_PLACEMENT_3D('',#16351,#13420,#13421);
#11985=AXIS2_PLACEMENT_3D('',#16352,#13422,#13423);
#11986=AXIS2_PLACEMENT_3D('',#16353,#13424,#13425);
#11987=AXIS2_PLACEMENT_3D('',#16354,#13426,#13427);
#11988=AXIS2_PLACEMENT_3D('',#16356,#13428,#13429);
#11989=AXIS2_PLACEMENT_3D('',#16359,#13431,#13432);
#11990=AXIS2_PLACEMENT_3D('',#16360,#13433,#13434);
#11991=AXIS2_PLACEMENT_3D('',#16362,#13435,#13436);
#11992=AXIS2_PLACEMENT_3D('',#16365,#13438,#13439);
#11993=AXIS2_PLACEMENT_3D('',#16366,#13440,#13441);
#11994=AXIS2_PLACEMENT_3D('',#16367,#13442,#13443);
#11995=AXIS2_PLACEMENT_3D('',#16368,#13444,#13445);
#11996=AXIS2_PLACEMENT_3D('',#16369,#13446,#13447);
#11997=AXIS2_PLACEMENT_3D('',#16371,#13448,#13449);
#11998=AXIS2_PLACEMENT_3D('',#16374,#13451,#13452);
#11999=AXIS2_PLACEMENT_3D('',#16375,#13453,#13454);
#12000=AXIS2_PLACEMENT_3D('',#16377,#13455,#13456);
#12001=AXIS2_PLACEMENT_3D('',#16380,#13458,#13459);
#12002=AXIS2_PLACEMENT_3D('',#16381,#13460,#13461);
#12003=AXIS2_PLACEMENT_3D('',#16382,#13462,#13463);
#12004=AXIS2_PLACEMENT_3D('',#16383,#13464,#13465);
#12005=AXIS2_PLACEMENT_3D('',#16384,#13466,#13467);
#12006=AXIS2_PLACEMENT_3D('',#16386,#13468,#13469);
#12007=AXIS2_PLACEMENT_3D('',#16389,#13471,#13472);
#12008=AXIS2_PLACEMENT_3D('',#16390,#13473,#13474);
#12009=AXIS2_PLACEMENT_3D('',#16392,#13475,#13476);
#12010=AXIS2_PLACEMENT_3D('',#16395,#13478,#13479);
#12011=AXIS2_PLACEMENT_3D('',#16396,#13480,#13481);
#12012=AXIS2_PLACEMENT_3D('',#16397,#13482,#13483);
#12013=AXIS2_PLACEMENT_3D('',#16398,#13484,#13485);
#12014=AXIS2_PLACEMENT_3D('',#16399,#13486,#13487);
#12015=AXIS2_PLACEMENT_3D('',#16401,#13488,#13489);
#12016=AXIS2_PLACEMENT_3D('',#16404,#13491,#13492);
#12017=AXIS2_PLACEMENT_3D('',#16405,#13493,#13494);
#12018=AXIS2_PLACEMENT_3D('',#16407,#13495,#13496);
#12019=AXIS2_PLACEMENT_3D('',#16410,#13498,#13499);
#12020=AXIS2_PLACEMENT_3D('',#16411,#13500,#13501);
#12021=AXIS2_PLACEMENT_3D('',#16413,#13502,#13503);
#12022=AXIS2_PLACEMENT_3D('',#16416,#13505,#13506);
#12023=AXIS2_PLACEMENT_3D('',#16417,#13507,#13508);
#12024=AXIS2_PLACEMENT_3D('',#16419,#13509,#13510);
#12025=AXIS2_PLACEMENT_3D('',#16422,#13512,#13513);
#12026=AXIS2_PLACEMENT_3D('',#16423,#13514,#13515);
#12027=AXIS2_PLACEMENT_3D('',#16425,#13516,#13517);
#12028=AXIS2_PLACEMENT_3D('',#16426,#13518,#13519);
#12029=AXIS2_PLACEMENT_3D('',#16429,#13521,#13522);
#12030=AXIS2_PLACEMENT_3D('',#16430,#13523,#13524);
#12031=AXIS2_PLACEMENT_3D('',#16432,#13525,#13526);
#12032=AXIS2_PLACEMENT_3D('',#16435,#13528,#13529);
#12033=AXIS2_PLACEMENT_3D('',#16436,#13530,#13531);
#12034=AXIS2_PLACEMENT_3D('',#16437,#13532,#13533);
#12035=AXIS2_PLACEMENT_3D('',#16438,#13534,#13535);
#12036=AXIS2_PLACEMENT_3D('',#16439,#13536,#13537);
#12037=AXIS2_PLACEMENT_3D('',#16441,#13538,#13539);
#12038=AXIS2_PLACEMENT_3D('',#16444,#13541,#13542);
#12039=AXIS2_PLACEMENT_3D('',#16445,#13543,#13544);
#12040=AXIS2_PLACEMENT_3D('',#16447,#13545,#13546);
#12041=AXIS2_PLACEMENT_3D('',#16450,#13548,#13549);
#12042=AXIS2_PLACEMENT_3D('',#16451,#13550,#13551);
#12043=AXIS2_PLACEMENT_3D('',#16453,#13552,#13553);
#12044=AXIS2_PLACEMENT_3D('',#16456,#13555,#13556);
#12045=AXIS2_PLACEMENT_3D('',#16457,#13557,#13558);
#12046=AXIS2_PLACEMENT_3D('',#16459,#13559,#13560);
#12047=AXIS2_PLACEMENT_3D('',#16462,#13562,#13563);
#12048=AXIS2_PLACEMENT_3D('',#16463,#13564,#13565);
#12049=AXIS2_PLACEMENT_3D('',#16465,#13566,#13567);
#12050=AXIS2_PLACEMENT_3D('',#16466,#13568,#13569);
#12051=AXIS2_PLACEMENT_3D('',#16469,#13571,#13572);
#12052=AXIS2_PLACEMENT_3D('',#16470,#13573,#13574);
#12053=AXIS2_PLACEMENT_3D('',#16472,#13575,#13576);
#12054=AXIS2_PLACEMENT_3D('',#16475,#13578,#13579);
#12055=AXIS2_PLACEMENT_3D('',#16476,#13580,#13581);
#12056=AXIS2_PLACEMENT_3D('',#16477,#13582,#13583);
#12057=AXIS2_PLACEMENT_3D('',#16478,#13584,#13585);
#12058=AXIS2_PLACEMENT_3D('',#16479,#13586,#13587);
#12059=AXIS2_PLACEMENT_3D('',#16481,#13588,#13589);
#12060=AXIS2_PLACEMENT_3D('',#16484,#13591,#13592);
#12061=AXIS2_PLACEMENT_3D('',#16485,#13593,#13594);
#12062=AXIS2_PLACEMENT_3D('',#16487,#13595,#13596);
#12063=AXIS2_PLACEMENT_3D('',#16490,#13598,#13599);
#12064=AXIS2_PLACEMENT_3D('',#16491,#13600,#13601);
#12065=AXIS2_PLACEMENT_3D('',#16493,#13602,#13603);
#12066=AXIS2_PLACEMENT_3D('',#16496,#13605,#13606);
#12067=AXIS2_PLACEMENT_3D('',#16497,#13607,#13608);
#12068=AXIS2_PLACEMENT_3D('',#16499,#13609,#13610);
#12069=AXIS2_PLACEMENT_3D('',#16502,#13612,#13613);
#12070=AXIS2_PLACEMENT_3D('',#16503,#13614,#13615);
#12071=AXIS2_PLACEMENT_3D('',#16505,#13616,#13617);
#12072=AXIS2_PLACEMENT_3D('',#16506,#13618,#13619);
#12073=AXIS2_PLACEMENT_3D('',#16508,#13620,#13621);
#12074=AXIS2_PLACEMENT_3D('',#16510,#13623,#13624);
#12075=AXIS2_PLACEMENT_3D('',#16512,#13625,#13626);
#12076=AXIS2_PLACEMENT_3D('',#16515,#13628,#13629);
#12077=AXIS2_PLACEMENT_3D('',#16516,#13630,#13631);
#12078=AXIS2_PLACEMENT_3D('',#16517,#13632,#13633);
#12079=AXIS2_PLACEMENT_3D('',#16518,#13634,#13635);
#12080=AXIS2_PLACEMENT_3D('',#16519,#13636,#13637);
#12081=AXIS2_PLACEMENT_3D('',#16521,#13638,#13639);
#12082=AXIS2_PLACEMENT_3D('',#16524,#13641,#13642);
#12083=AXIS2_PLACEMENT_3D('',#16525,#13643,#13644);
#12084=AXIS2_PLACEMENT_3D('',#16527,#13645,#13646);
#12085=AXIS2_PLACEMENT_3D('',#16530,#13648,#13649);
#12086=AXIS2_PLACEMENT_3D('',#16531,#13650,#13651);
#12087=AXIS2_PLACEMENT_3D('',#16533,#13652,#13653);
#12088=AXIS2_PLACEMENT_3D('',#16536,#13655,#13656);
#12089=AXIS2_PLACEMENT_3D('',#16537,#13657,#13658);
#12090=AXIS2_PLACEMENT_3D('',#16539,#13659,#13660);
#12091=AXIS2_PLACEMENT_3D('',#16542,#13662,#13663);
#12092=AXIS2_PLACEMENT_3D('',#16543,#13664,#13665);
#12093=AXIS2_PLACEMENT_3D('',#16545,#13666,#13667);
#12094=AXIS2_PLACEMENT_3D('',#16546,#13668,#13669);
#12095=AXIS2_PLACEMENT_3D('',#16548,#13670,#13671);
#12096=AXIS2_PLACEMENT_3D('',#16550,#13673,#13674);
#12097=AXIS2_PLACEMENT_3D('',#16552,#13675,#13676);
#12098=AXIS2_PLACEMENT_3D('',#16555,#13678,#13679);
#12099=AXIS2_PLACEMENT_3D('',#16556,#13680,#13681);
#12100=AXIS2_PLACEMENT_3D('',#16557,#13682,#13683);
#12101=AXIS2_PLACEMENT_3D('',#16558,#13684,#13685);
#12102=AXIS2_PLACEMENT_3D('',#16559,#13686,#13687);
#12103=AXIS2_PLACEMENT_3D('',#16561,#13688,#13689);
#12104=AXIS2_PLACEMENT_3D('',#16562,#13690,#13691);
#12105=AXIS2_PLACEMENT_3D('',#16564,#13692,#13693);
#12106=AXIS2_PLACEMENT_3D('',#16566,#13695,#13696);
#12107=AXIS2_PLACEMENT_3D('',#16568,#13697,#13698);
#12108=AXIS2_PLACEMENT_3D('',#16570,#13700,#13701);
#12109=AXIS2_PLACEMENT_3D('',#16572,#13702,#13703);
#12110=AXIS2_PLACEMENT_3D('',#16574,#13705,#13706);
#12111=AXIS2_PLACEMENT_3D('',#16576,#13707,#13708);
#12112=AXIS2_PLACEMENT_3D('',#16577,#13709,#13710);
#12113=AXIS2_PLACEMENT_3D('',#16579,#13711,#13712);
#12114=AXIS2_PLACEMENT_3D('',#16581,#13714,#13715);
#12115=AXIS2_PLACEMENT_3D('',#16583,#13716,#13717);
#12116=AXIS2_PLACEMENT_3D('',#16585,#13719,#13720);
#12117=AXIS2_PLACEMENT_3D('',#16587,#13721,#13722);
#12118=AXIS2_PLACEMENT_3D('',#16589,#13724,#13725);
#12119=AXIS2_PLACEMENT_3D('',#16590,#13726,#13727);
#12120=AXIS2_PLACEMENT_3D('',#16599,#13732,#13733);
#12121=AXIS2_PLACEMENT_3D('',#16605,#13737,#13738);
#12122=AXIS2_PLACEMENT_3D('',#16611,#13742,#13743);
#12123=AXIS2_PLACEMENT_3D('',#16617,#13747,#13748);
#12124=AXIS2_PLACEMENT_3D('',#16623,#13752,#13753);
#12125=AXIS2_PLACEMENT_3D('',#16626,#13756,#13757);
#12126=AXIS2_PLACEMENT_3D('',#16627,#13758,#13759);
#12127=AXIS2_PLACEMENT_3D('',#16628,#13760,#13761);
#12128=AXIS2_PLACEMENT_3D('',#16629,#13762,#13763);
#12129=AXIS2_PLACEMENT_3D('',#16631,#13764,#13765);
#12130=AXIS2_PLACEMENT_3D('',#16632,#13766,#13767);
#12131=AXIS2_PLACEMENT_3D('',#16634,#13768,#13769);
#12132=AXIS2_PLACEMENT_3D('',#16636,#13771,#13772);
#12133=AXIS2_PLACEMENT_3D('',#16638,#13773,#13774);
#12134=AXIS2_PLACEMENT_3D('',#16640,#13776,#13777);
#12135=AXIS2_PLACEMENT_3D('',#16642,#13778,#13779);
#12136=AXIS2_PLACEMENT_3D('',#16644,#13781,#13782);
#12137=AXIS2_PLACEMENT_3D('',#16646,#13783,#13784);
#12138=AXIS2_PLACEMENT_3D('',#16647,#13785,#13786);
#12139=AXIS2_PLACEMENT_3D('',#16649,#13787,#13788);
#12140=AXIS2_PLACEMENT_3D('',#16651,#13790,#13791);
#12141=AXIS2_PLACEMENT_3D('',#16653,#13792,#13793);
#12142=AXIS2_PLACEMENT_3D('',#16655,#13795,#13796);
#12143=AXIS2_PLACEMENT_3D('',#16657,#13797,#13798);
#12144=AXIS2_PLACEMENT_3D('',#16659,#13800,#13801);
#12145=AXIS2_PLACEMENT_3D('',#16660,#13802,#13803);
#12146=AXIS2_PLACEMENT_3D('',#16669,#13808,#13809);
#12147=AXIS2_PLACEMENT_3D('',#16675,#13813,#13814);
#12148=AXIS2_PLACEMENT_3D('',#16681,#13818,#13819);
#12149=AXIS2_PLACEMENT_3D('',#16687,#13823,#13824);
#12150=AXIS2_PLACEMENT_3D('',#16693,#13828,#13829);
#12151=AXIS2_PLACEMENT_3D('',#16696,#13832,#13833);
#12152=AXIS2_PLACEMENT_3D('',#16697,#13834,#13835);
#12153=AXIS2_PLACEMENT_3D('',#16698,#13836,#13837);
#12154=AXIS2_PLACEMENT_3D('',#16699,#13838,#13839);
#12155=AXIS2_PLACEMENT_3D('',#16700,#13840,#13841);
#12156=AXIS2_PLACEMENT_3D('',#16703,#13842,#13843);
#12157=AXIS2_PLACEMENT_3D('',#16704,#13844,#13845);
#12158=AXIS2_PLACEMENT_3D('',#16706,#13846,#13847);
#12159=AXIS2_PLACEMENT_3D('',#16708,#13848,#13849);
#12160=AXIS2_PLACEMENT_3D('',#16709,#13850,#13851);
#12161=AXIS2_PLACEMENT_3D('',#16710,#13852,#13853);
#12162=AXIS2_PLACEMENT_3D('',#16713,#13855,#13856);
#12163=AXIS2_PLACEMENT_3D('',#16714,#13857,#13858);
#12164=AXIS2_PLACEMENT_3D('',#16716,#13859,#13860);
#12165=AXIS2_PLACEMENT_3D('',#16719,#13862,#13863);
#12166=AXIS2_PLACEMENT_3D('',#16720,#13864,#13865);
#12167=AXIS2_PLACEMENT_3D('',#16723,#13867,#13868);
#12168=AXIS2_PLACEMENT_3D('',#16724,#13869,#13870);
#12169=AXIS2_PLACEMENT_3D('',#16725,#13871,#13872);
#12170=AXIS2_PLACEMENT_3D('',#16727,#13873,#13874);
#12171=AXIS2_PLACEMENT_3D('',#16729,#13876,#13877);
#12172=AXIS2_PLACEMENT_3D('',#16731,#13878,#13879);
#12173=AXIS2_PLACEMENT_3D('',#16732,#13880,#13881);
#12174=AXIS2_PLACEMENT_3D('',#16734,#13883,#13884);
#12175=AXIS2_PLACEMENT_3D('',#16735,#13885,#13886);
#12176=AXIS2_PLACEMENT_3D('',#16738,#13887,#13888);
#12177=AXIS2_PLACEMENT_3D('',#16739,#13889,#13890);
#12178=AXIS2_PLACEMENT_3D('',#16741,#13891,#13892);
#12179=AXIS2_PLACEMENT_3D('',#16743,#13893,#13894);
#12180=AXIS2_PLACEMENT_3D('',#16744,#13895,#13896);
#12181=AXIS2_PLACEMENT_3D('',#16745,#13897,#13898);
#12182=AXIS2_PLACEMENT_3D('',#16747,#13899,#13900);
#12183=AXIS2_PLACEMENT_3D('',#16749,#13902,#13903);
#12184=AXIS2_PLACEMENT_3D('',#16751,#13904,#13905);
#12185=AXIS2_PLACEMENT_3D('',#16753,#13906,#13907);
#12186=AXIS2_PLACEMENT_3D('',#16754,#13908,#13909);
#12187=AXIS2_PLACEMENT_3D('',#16756,#13910,#13911);
#12188=AXIS2_PLACEMENT_3D('',#16758,#13913,#13914);
#12189=AXIS2_PLACEMENT_3D('',#16760,#13915,#13916);
#12190=AXIS2_PLACEMENT_3D('',#16762,#13918,#13919);
#12191=AXIS2_PLACEMENT_3D('',#16764,#13920,#13921);
#12192=AXIS2_PLACEMENT_3D('',#16766,#13923,#13924);
#12193=AXIS2_PLACEMENT_3D('',#16767,#13925,#13926);
#12194=AXIS2_PLACEMENT_3D('',#16769,#13928,#13929);
#12195=AXIS2_PLACEMENT_3D('',#16770,#13930,#13931);
#12196=AXIS2_PLACEMENT_3D('',#16773,#13932,#13933);
#12197=AXIS2_PLACEMENT_3D('',#16774,#13934,#13935);
#12198=AXIS2_PLACEMENT_3D('',#16777,#13936,#13937);
#12199=AXIS2_PLACEMENT_3D('',#16778,#13938,#13939);
#12200=AXIS2_PLACEMENT_3D('',#16781,#13940,#13941);
#12201=AXIS2_PLACEMENT_3D('',#16782,#13942,#13943);
#12202=AXIS2_PLACEMENT_3D('',#16785,#13944,#13945);
#12203=AXIS2_PLACEMENT_3D('',#16786,#13946,#13947);
#12204=AXIS2_PLACEMENT_3D('',#16789,#13948,#13949);
#12205=AXIS2_PLACEMENT_3D('',#16790,#13950,#13951);
#12206=AXIS2_PLACEMENT_3D('',#16793,#13952,#13953);
#12207=AXIS2_PLACEMENT_3D('',#16794,#13954,#13955);
#12208=AXIS2_PLACEMENT_3D('',#16797,#13956,#13957);
#12209=AXIS2_PLACEMENT_3D('',#16798,#13958,#13959);
#12210=AXIS2_PLACEMENT_3D('',#16799,#13960,#13961);
#12211=AXIS2_PLACEMENT_3D('',#16825,#13962,#13963);
#12212=AXIS2_PLACEMENT_3D('',#16849,#13964,#13965);
#12213=AXIS2_PLACEMENT_3D('',#16850,#13966,#13967);
#12214=AXIS2_PLACEMENT_3D('',#16852,#13968,#13969);
#12215=AXIS2_PLACEMENT_3D('',#16877,#13970,#13971);
#12216=AXIS2_PLACEMENT_3D('',#16902,#13972,#13973);
#12217=AXIS2_PLACEMENT_3D('',#16905,#13975,#13976);
#12218=AXIS2_PLACEMENT_3D('',#16907,#13977,#13978);
#12219=AXIS2_PLACEMENT_3D('',#16932,#13979,#13980);
#12220=AXIS2_PLACEMENT_3D('',#16957,#13981,#13982);
#12221=AXIS2_PLACEMENT_3D('',#16982,#13983,#13984);
#12222=AXIS2_PLACEMENT_3D('',#17006,#13985,#13986);
#12223=AXIS2_PLACEMENT_3D('',#17007,#13987,#13988);
#12224=AXIS2_PLACEMENT_3D('',#17009,#13989,#13990);
#12225=AXIS2_PLACEMENT_3D('',#17010,#13991,#13992);
#12226=AXIS2_PLACEMENT_3D('',#17011,#13993,#13994);
#12227=AXIS2_PLACEMENT_3D('',#17035,#13995,#13996);
#12228=AXIS2_PLACEMENT_3D('',#17036,#13997,#13998);
#12229=AXIS2_PLACEMENT_3D('',#17038,#13999,#14000);
#12230=AXIS2_PLACEMENT_3D('',#17039,#14001,#14002);
#12231=AXIS2_PLACEMENT_3D('',#17040,#14003,#14004);
#12232=AXIS2_PLACEMENT_3D('',#17064,#14005,#14006);
#12233=AXIS2_PLACEMENT_3D('',#17065,#14007,#14008);
#12234=AXIS2_PLACEMENT_3D('',#17067,#14009,#14010);
#12235=AXIS2_PLACEMENT_3D('',#17069,#14011,#14012);
#12236=AXIS2_PLACEMENT_3D('',#17070,#14013,#14014);
#12237=AXIS2_PLACEMENT_3D('',#17071,#14015,#14016);
#12238=AXIS2_PLACEMENT_3D('',#17095,#14017,#14018);
#12239=AXIS2_PLACEMENT_3D('',#17096,#14019,#14020);
#12240=AXIS2_PLACEMENT_3D('',#17098,#14021,#14022);
#12241=AXIS2_PLACEMENT_3D('',#17099,#14023,#14024);
#12242=AXIS2_PLACEMENT_3D('',#17100,#14025,#14026);
#12243=AXIS2_PLACEMENT_3D('',#17124,#14027,#14028);
#12244=AXIS2_PLACEMENT_3D('',#17125,#14029,#14030);
#12245=AXIS2_PLACEMENT_3D('',#17127,#14031,#14032);
#12246=AXIS2_PLACEMENT_3D('',#17128,#14033,#14034);
#12247=AXIS2_PLACEMENT_3D('',#17129,#14035,#14036);
#12248=AXIS2_PLACEMENT_3D('',#17153,#14037,#14038);
#12249=AXIS2_PLACEMENT_3D('',#17154,#14039,#14040);
#12250=AXIS2_PLACEMENT_3D('',#17156,#14041,#14042);
#12251=AXIS2_PLACEMENT_3D('',#17159,#14044,#14045);
#12252=AXIS2_PLACEMENT_3D('',#17183,#14046,#14047);
#12253=AXIS2_PLACEMENT_3D('',#17184,#14048,#14049);
#12254=AXIS2_PLACEMENT_3D('',#17185,#14050,#14051);
#12255=AXIS2_PLACEMENT_3D('',#17186,#14052,#14053);
#12256=AXIS2_PLACEMENT_3D('',#17187,#14054,#14055);
#12257=AXIS2_PLACEMENT_3D('',#17188,#14056,#14057);
#12258=AXIS2_PLACEMENT_3D('',#17189,#14058,#14059);
#12259=AXIS2_PLACEMENT_3D('',#17190,#14060,#14061);
#12260=AXIS2_PLACEMENT_3D('',#17191,#14062,#14063);
#12261=AXIS2_PLACEMENT_3D('',#17193,#14064,#14065);
#12262=AXIS2_PLACEMENT_3D('',#17195,#14066,#14067);
#12263=AXIS2_PLACEMENT_3D('',#17196,#14068,#14069);
#12264=AXIS2_PLACEMENT_3D('',#17198,#14070,#14071);
#12265=AXIS2_PLACEMENT_3D('',#17200,#14073,#14074);
#12266=AXIS2_PLACEMENT_3D('',#17202,#14075,#14076);
#12267=AXIS2_PLACEMENT_3D('',#17203,#14077,#14078);
#12268=AXIS2_PLACEMENT_3D('',#17205,#14080,#14081);
#12269=AXIS2_PLACEMENT_3D('',#17207,#14082,#14083);
#12270=AXIS2_PLACEMENT_3D('',#17209,#14084,#14085);
#12271=AXIS2_PLACEMENT_3D('',#17210,#14086,#14087);
#12272=AXIS2_PLACEMENT_3D('',#17212,#14088,#14089);
#12273=AXIS2_PLACEMENT_3D('',#17214,#14091,#14092);
#12274=AXIS2_PLACEMENT_3D('',#17216,#14093,#14094);
#12275=AXIS2_PLACEMENT_3D('',#17217,#14095,#14096);
#12276=AXIS2_PLACEMENT_3D('',#17219,#14098,#14099);
#12277=AXIS2_PLACEMENT_3D('',#17220,#14100,#14101);
#12278=AXIS2_PLACEMENT_3D('',#17221,#14102,#14103);
#12279=AXIS2_PLACEMENT_3D('',#17222,#14104,#14105);
#12280=AXIS2_PLACEMENT_3D('',#17223,#14106,#14107);
#12281=AXIS2_PLACEMENT_3D('',#17224,#14108,#14109);
#12282=AXIS2_PLACEMENT_3D('',#17225,#14110,#14111);
#12283=AXIS2_PLACEMENT_3D('',#17226,#14112,#14113);
#12284=AXIS2_PLACEMENT_3D('',#17229,#14114,#14115);
#12285=AXIS2_PLACEMENT_3D('',#17230,#14116,#14117);
#12286=AXIS2_PLACEMENT_3D('',#17232,#14118,#14119);
#12287=AXIS2_PLACEMENT_3D('',#17234,#14120,#14121);
#12288=AXIS2_PLACEMENT_3D('',#17235,#14122,#14123);
#12289=AXIS2_PLACEMENT_3D('',#17236,#14124,#14125);
#12290=AXIS2_PLACEMENT_3D('',#17239,#14127,#14128);
#12291=AXIS2_PLACEMENT_3D('',#17240,#14129,#14130);
#12292=AXIS2_PLACEMENT_3D('',#17242,#14131,#14132);
#12293=AXIS2_PLACEMENT_3D('',#17245,#14134,#14135);
#12294=AXIS2_PLACEMENT_3D('',#17246,#14136,#14137);
#12295=AXIS2_PLACEMENT_3D('',#17249,#14139,#14140);
#12296=AXIS2_PLACEMENT_3D('',#17250,#14141,#14142);
#12297=AXIS2_PLACEMENT_3D('',#17251,#14143,#14144);
#12298=AXIS2_PLACEMENT_3D('',#17253,#14145,#14146);
#12299=AXIS2_PLACEMENT_3D('',#17255,#14148,#14149);
#12300=AXIS2_PLACEMENT_3D('',#17257,#14150,#14151);
#12301=AXIS2_PLACEMENT_3D('',#17258,#14152,#14153);
#12302=AXIS2_PLACEMENT_3D('',#17260,#14155,#14156);
#12303=AXIS2_PLACEMENT_3D('',#17261,#14157,#14158);
#12304=AXIS2_PLACEMENT_3D('',#17264,#14159,#14160);
#12305=AXIS2_PLACEMENT_3D('',#17265,#14161,#14162);
#12306=AXIS2_PLACEMENT_3D('',#17267,#14163,#14164);
#12307=AXIS2_PLACEMENT_3D('',#17269,#14165,#14166);
#12308=AXIS2_PLACEMENT_3D('',#17270,#14167,#14168);
#12309=AXIS2_PLACEMENT_3D('',#17271,#14169,#14170);
#12310=AXIS2_PLACEMENT_3D('',#17273,#14171,#14172);
#12311=AXIS2_PLACEMENT_3D('',#17275,#14174,#14175);
#12312=AXIS2_PLACEMENT_3D('',#17277,#14176,#14177);
#12313=AXIS2_PLACEMENT_3D('',#17279,#14178,#14179);
#12314=AXIS2_PLACEMENT_3D('',#17280,#14180,#14181);
#12315=AXIS2_PLACEMENT_3D('',#17282,#14182,#14183);
#12316=AXIS2_PLACEMENT_3D('',#17284,#14185,#14186);
#12317=AXIS2_PLACEMENT_3D('',#17286,#14187,#14188);
#12318=AXIS2_PLACEMENT_3D('',#17288,#14190,#14191);
#12319=AXIS2_PLACEMENT_3D('',#17290,#14192,#14193);
#12320=AXIS2_PLACEMENT_3D('',#17292,#14195,#14196);
#12321=AXIS2_PLACEMENT_3D('',#17293,#14197,#14198);
#12322=AXIS2_PLACEMENT_3D('',#17295,#14200,#14201);
#12323=AXIS2_PLACEMENT_3D('',#17296,#14202,#14203);
#12324=AXIS2_PLACEMENT_3D('',#17299,#14204,#14205);
#12325=AXIS2_PLACEMENT_3D('',#17300,#14206,#14207);
#12326=AXIS2_PLACEMENT_3D('',#17303,#14208,#14209);
#12327=AXIS2_PLACEMENT_3D('',#17304,#14210,#14211);
#12328=AXIS2_PLACEMENT_3D('',#17307,#14212,#14213);
#12329=AXIS2_PLACEMENT_3D('',#17308,#14214,#14215);
#12330=AXIS2_PLACEMENT_3D('',#17311,#14216,#14217);
#12331=AXIS2_PLACEMENT_3D('',#17312,#14218,#14219);
#12332=AXIS2_PLACEMENT_3D('',#17315,#14220,#14221);
#12333=AXIS2_PLACEMENT_3D('',#17316,#14222,#14223);
#12334=AXIS2_PLACEMENT_3D('',#17319,#14224,#14225);
#12335=AXIS2_PLACEMENT_3D('',#17320,#14226,#14227);
#12336=AXIS2_PLACEMENT_3D('',#17323,#14228,#14229);
#12337=AXIS2_PLACEMENT_3D('',#17324,#14230,#14231);
#12338=AXIS2_PLACEMENT_3D('',#17327,#14232,#14233);
#12339=AXIS2_PLACEMENT_3D('',#17328,#14234,#14235);
#12340=AXIS2_PLACEMENT_3D('',#17329,#14236,#14237);
#12341=AXIS2_PLACEMENT_3D('',#17355,#14238,#14239);
#12342=AXIS2_PLACEMENT_3D('',#17379,#14240,#14241);
#12343=AXIS2_PLACEMENT_3D('',#17380,#14242,#14243);
#12344=AXIS2_PLACEMENT_3D('',#17382,#14244,#14245);
#12345=AXIS2_PLACEMENT_3D('',#17407,#14246,#14247);
#12346=AXIS2_PLACEMENT_3D('',#17432,#14248,#14249);
#12347=AXIS2_PLACEMENT_3D('',#17448,#14251,#14252);
#12348=AXIS2_PLACEMENT_3D('',#17463,#14253,#14254);
#12349=AXIS2_PLACEMENT_3D('',#17488,#14255,#14256);
#12350=AXIS2_PLACEMENT_3D('',#17513,#14257,#14258);
#12351=AXIS2_PLACEMENT_3D('',#17538,#14259,#14260);
#12352=AXIS2_PLACEMENT_3D('',#17562,#14261,#14262);
#12353=AXIS2_PLACEMENT_3D('',#17563,#14263,#14264);
#12354=AXIS2_PLACEMENT_3D('',#17565,#14265,#14266);
#12355=AXIS2_PLACEMENT_3D('',#17566,#14267,#14268);
#12356=AXIS2_PLACEMENT_3D('',#17567,#14269,#14270);
#12357=AXIS2_PLACEMENT_3D('',#17591,#14271,#14272);
#12358=AXIS2_PLACEMENT_3D('',#17592,#14273,#14274);
#12359=AXIS2_PLACEMENT_3D('',#17594,#14275,#14276);
#12360=AXIS2_PLACEMENT_3D('',#17595,#14277,#14278);
#12361=AXIS2_PLACEMENT_3D('',#17596,#14279,#14280);
#12362=AXIS2_PLACEMENT_3D('',#17620,#14281,#14282);
#12363=AXIS2_PLACEMENT_3D('',#17621,#14283,#14284);
#12364=AXIS2_PLACEMENT_3D('',#17623,#14285,#14286);
#12365=AXIS2_PLACEMENT_3D('',#17624,#14287,#14288);
#12366=AXIS2_PLACEMENT_3D('',#17625,#14289,#14290);
#12367=AXIS2_PLACEMENT_3D('',#17640,#14291,#14292);
#12368=AXIS2_PLACEMENT_3D('',#17653,#14293,#14294);
#12369=AXIS2_PLACEMENT_3D('',#17655,#14295,#14296);
#12370=AXIS2_PLACEMENT_3D('',#17656,#14297,#14298);
#12371=AXIS2_PLACEMENT_3D('',#17657,#14299,#14300);
#12372=AXIS2_PLACEMENT_3D('',#17681,#14301,#14302);
#12373=AXIS2_PLACEMENT_3D('',#17682,#14303,#14304);
#12374=AXIS2_PLACEMENT_3D('',#17684,#14305,#14306);
#12375=AXIS2_PLACEMENT_3D('',#17685,#14307,#14308);
#12376=AXIS2_PLACEMENT_3D('',#17686,#14309,#14310);
#12377=AXIS2_PLACEMENT_3D('',#17710,#14311,#14312);
#12378=AXIS2_PLACEMENT_3D('',#17711,#14313,#14314);
#12379=AXIS2_PLACEMENT_3D('',#17713,#14315,#14316);
#12380=AXIS2_PLACEMENT_3D('',#17714,#14317,#14318);
#12381=AXIS2_PLACEMENT_3D('',#17715,#14319,#14320);
#12382=AXIS2_PLACEMENT_3D('',#17739,#14321,#14322);
#12383=AXIS2_PLACEMENT_3D('',#17740,#14323,#14324);
#12384=AXIS2_PLACEMENT_3D('',#17742,#14325,#14326);
#12385=AXIS2_PLACEMENT_3D('',#17745,#14328,#14329);
#12386=AXIS2_PLACEMENT_3D('',#17769,#14330,#14331);
#12387=AXIS2_PLACEMENT_3D('',#17770,#14332,#14333);
#12388=AXIS2_PLACEMENT_3D('',#17771,#14334,#14335);
#12389=AXIS2_PLACEMENT_3D('',#17772,#14336,#14337);
#12390=AXIS2_PLACEMENT_3D('',#17773,#14338,#14339);
#12391=AXIS2_PLACEMENT_3D('',#17774,#14340,#14341);
#12392=AXIS2_PLACEMENT_3D('',#17775,#14342,#14343);
#12393=AXIS2_PLACEMENT_3D('',#17776,#14344,#14345);
#12394=AXIS2_PLACEMENT_3D('',#17777,#14346,#14347);
#12395=AXIS2_PLACEMENT_3D('',#17779,#14348,#14349);
#12396=AXIS2_PLACEMENT_3D('',#17781,#14350,#14351);
#12397=AXIS2_PLACEMENT_3D('',#17782,#14352,#14353);
#12398=AXIS2_PLACEMENT_3D('',#17784,#14354,#14355);
#12399=AXIS2_PLACEMENT_3D('',#17786,#14357,#14358);
#12400=AXIS2_PLACEMENT_3D('',#17788,#14359,#14360);
#12401=AXIS2_PLACEMENT_3D('',#17789,#14361,#14362);
#12402=AXIS2_PLACEMENT_3D('',#17791,#14364,#14365);
#12403=AXIS2_PLACEMENT_3D('',#17793,#14366,#14367);
#12404=AXIS2_PLACEMENT_3D('',#17795,#14368,#14369);
#12405=AXIS2_PLACEMENT_3D('',#17796,#14370,#14371);
#12406=AXIS2_PLACEMENT_3D('',#17798,#14372,#14373);
#12407=AXIS2_PLACEMENT_3D('',#17800,#14375,#14376);
#12408=AXIS2_PLACEMENT_3D('',#17802,#14377,#14378);
#12409=AXIS2_PLACEMENT_3D('',#17803,#14379,#14380);
#12410=AXIS2_PLACEMENT_3D('',#17805,#14382,#14383);
#12411=AXIS2_PLACEMENT_3D('',#17806,#14384,#14385);
#12412=AXIS2_PLACEMENT_3D('',#17807,#14386,#14387);
#12413=AXIS2_PLACEMENT_3D('',#17808,#14388,#14389);
#12414=AXIS2_PLACEMENT_3D('',#17809,#14390,#14391);
#12415=AXIS2_PLACEMENT_3D('',#17810,#14392,#14393);
#12416=AXIS2_PLACEMENT_3D('',#17811,#14394,#14395);
#12417=AXIS2_PLACEMENT_3D('',#17813,#14396,#14397);
#12418=AXIS2_PLACEMENT_3D('',#17814,#14398,#14399);
#12419=AXIS2_PLACEMENT_3D('',#17816,#14400,#14401);
#12420=AXIS2_PLACEMENT_3D('',#17818,#14403,#14404);
#12421=AXIS2_PLACEMENT_3D('',#17820,#14405,#14406);
#12422=AXIS2_PLACEMENT_3D('',#17822,#14408,#14409);
#12423=AXIS2_PLACEMENT_3D('',#17824,#14410,#14411);
#12424=AXIS2_PLACEMENT_3D('',#17826,#14413,#14414);
#12425=AXIS2_PLACEMENT_3D('',#17828,#14415,#14416);
#12426=AXIS2_PLACEMENT_3D('',#17829,#14417,#14418);
#12427=AXIS2_PLACEMENT_3D('',#17831,#14419,#14420);
#12428=AXIS2_PLACEMENT_3D('',#17833,#14422,#14423);
#12429=AXIS2_PLACEMENT_3D('',#17835,#14424,#14425);
#12430=AXIS2_PLACEMENT_3D('',#17837,#14427,#14428);
#12431=AXIS2_PLACEMENT_3D('',#17839,#14429,#14430);
#12432=AXIS2_PLACEMENT_3D('',#17841,#14432,#14433);
#12433=AXIS2_PLACEMENT_3D('',#17842,#14434,#14435);
#12434=AXIS2_PLACEMENT_3D('',#17851,#14440,#14441);
#12435=AXIS2_PLACEMENT_3D('',#17857,#14445,#14446);
#12436=AXIS2_PLACEMENT_3D('',#17863,#14450,#14451);
#12437=AXIS2_PLACEMENT_3D('',#17869,#14455,#14456);
#12438=AXIS2_PLACEMENT_3D('',#17875,#14460,#14461);
#12439=AXIS2_PLACEMENT_3D('',#17878,#14464,#14465);
#12440=AXIS2_PLACEMENT_3D('',#17879,#14466,#14467);
#12441=AXIS2_PLACEMENT_3D('',#17880,#14468,#14469);
#12442=AXIS2_PLACEMENT_3D('',#17881,#14470,#14471);
#12443=AXIS2_PLACEMENT_3D('',#17882,#14472,#14473);
#12444=AXIS2_PLACEMENT_3D('',#17883,#14474,#14475);
#12445=AXIS2_PLACEMENT_3D('',#17884,#14476,#14477);
#12446=AXIS2_PLACEMENT_3D('',#17885,#14478,#14479);
#12447=AXIS2_PLACEMENT_3D('',#17886,#14480,#14481);
#12448=AXIS2_PLACEMENT_3D('',#17887,#14482,#14483);
#12449=AXIS2_PLACEMENT_3D('',#17888,#14484,#14485);
#12450=AXIS2_PLACEMENT_3D('',#17889,#14486,#14487);
#12451=AXIS2_PLACEMENT_3D('',#17890,#14488,#14489);
#12452=AXIS2_PLACEMENT_3D('',#17891,#14490,#14491);
#12453=AXIS2_PLACEMENT_3D('',#17892,#14492,#14493);
#12454=AXIS2_PLACEMENT_3D('',#17893,#14494,#14495);
#12455=AXIS2_PLACEMENT_3D('',#17894,#14496,#14497);
#12456=AXIS2_PLACEMENT_3D('',#17895,#14498,#14499);
#12457=AXIS2_PLACEMENT_3D('',#17896,#14500,#14501);
#12458=AXIS2_PLACEMENT_3D('',#17897,#14502,#14503);
#12459=AXIS2_PLACEMENT_3D('',#17898,#14504,#14505);
#12460=AXIS2_PLACEMENT_3D('',#17899,#14506,#14507);
#12461=AXIS2_PLACEMENT_3D('',#17900,#14508,#14509);
#12462=AXIS2_PLACEMENT_3D('',#17901,#14510,#14511);
#12463=AXIS2_PLACEMENT_3D('',#17902,#14512,#14513);
#12464=AXIS2_PLACEMENT_3D('',#17903,#14514,#14515);
#12465=AXIS2_PLACEMENT_3D('',#17904,#14516,#14517);
#12466=AXIS2_PLACEMENT_3D('',#17905,#14518,#14519);
#12467=AXIS2_PLACEMENT_3D('',#17906,#14520,#14521);
#12468=AXIS2_PLACEMENT_3D('',#17907,#14522,#14523);
#12469=AXIS2_PLACEMENT_3D('',#17908,#14524,#14525);
#12470=AXIS2_PLACEMENT_3D('',#17909,#14526,#14527);
#12471=AXIS2_PLACEMENT_3D('',#17910,#14528,#14529);
#12472=AXIS2_PLACEMENT_3D('',#17911,#14530,#14531);
#12473=AXIS2_PLACEMENT_3D('',#17912,#14532,#14533);
#12474=AXIS2_PLACEMENT_3D('',#17913,#14534,#14535);
#12475=AXIS2_PLACEMENT_3D('',#17914,#14536,#14537);
#12476=AXIS2_PLACEMENT_3D('',#17915,#14538,#14539);
#12477=AXIS2_PLACEMENT_3D('',#17916,#14540,#14541);
#12478=AXIS2_PLACEMENT_3D('',#17917,#14542,#14543);
#12479=AXIS2_PLACEMENT_3D('',#17918,#14544,#14545);
#12480=AXIS2_PLACEMENT_3D('',#17919,#14546,#14547);
#12481=AXIS2_PLACEMENT_3D('',#17920,#14548,#14549);
#12482=AXIS2_PLACEMENT_3D('',#17921,#14550,#14551);
#12483=AXIS2_PLACEMENT_3D('',#17930,#14556,#14557);
#12484=AXIS2_PLACEMENT_3D('',#17932,#14558,#14559);
#12485=AXIS2_PLACEMENT_3D('',#17936,#14562,#14563);
#12486=AXIS2_PLACEMENT_3D('',#17942,#14567,#14568);
#12487=AXIS2_PLACEMENT_3D('',#17944,#14570,#14571);
#12488=AXIS2_PLACEMENT_3D('',#17945,#14572,#14573);
#12489=AXIS2_PLACEMENT_3D('',#17946,#14574,#14575);
#12490=AXIS2_PLACEMENT_3D('',#17948,#14576,#14577);
#12491=AXIS2_PLACEMENT_3D('',#17951,#14579,#14580);
#12492=AXIS2_PLACEMENT_3D('',#17952,#14581,#14582);
#12493=AXIS2_PLACEMENT_3D('',#17953,#14583,#14584);
#12494=AXIS2_PLACEMENT_3D('',#17954,#14585,#14586);
#12495=AXIS2_PLACEMENT_3D('',#17955,#14587,#14588);
#12496=AXIS2_PLACEMENT_3D('',#17957,#14589,#14590);
#12497=AXIS2_PLACEMENT_3D('',#17960,#14592,#14593);
#12498=AXIS2_PLACEMENT_3D('',#17961,#14594,#14595);
#12499=AXIS2_PLACEMENT_3D('',#17963,#14596,#14597);
#12500=AXIS2_PLACEMENT_3D('',#17966,#14599,#14600);
#12501=AXIS2_PLACEMENT_3D('',#17967,#14601,#14602);
#12502=AXIS2_PLACEMENT_3D('',#17968,#14603,#14604);
#12503=AXIS2_PLACEMENT_3D('',#17969,#14605,#14606);
#12504=AXIS2_PLACEMENT_3D('',#17970,#14607,#14608);
#12505=AXIS2_PLACEMENT_3D('',#17972,#14609,#14610);
#12506=AXIS2_PLACEMENT_3D('',#17975,#14612,#14613);
#12507=AXIS2_PLACEMENT_3D('',#17976,#14614,#14615);
#12508=AXIS2_PLACEMENT_3D('',#17978,#14616,#14617);
#12509=AXIS2_PLACEMENT_3D('',#17981,#14619,#14620);
#12510=AXIS2_PLACEMENT_3D('',#17982,#14621,#14622);
#12511=AXIS2_PLACEMENT_3D('',#17983,#14623,#14624);
#12512=AXIS2_PLACEMENT_3D('',#17984,#14625,#14626);
#12513=AXIS2_PLACEMENT_3D('',#17985,#14627,#14628);
#12514=AXIS2_PLACEMENT_3D('',#17989,#14630,#14631);
#12515=AXIS2_PLACEMENT_3D('',#17990,#14632,#14633);
#12516=AXIS2_PLACEMENT_3D('',#18003,#14634,#14635);
#12517=AXIS2_PLACEMENT_3D('',#18044,#14637,#14638);
#12518=AXIS2_PLACEMENT_3D('',#18055,#14639,#14640);
#12519=AXIS2_PLACEMENT_3D('',#18057,#14642,#14643);
#12520=AXIS2_PLACEMENT_3D('',#18059,#14644,#14645);
#12521=AXIS2_PLACEMENT_3D('',#18062,#14647,#14648);
#12522=AXIS2_PLACEMENT_3D('',#18063,#14649,#14650);
#12523=AXIS2_PLACEMENT_3D('',#18065,#14651,#14652);
#12524=AXIS2_PLACEMENT_3D('',#18068,#14654,#14655);
#12525=AXIS2_PLACEMENT_3D('',#18069,#14656,#14657);
#12526=AXIS2_PLACEMENT_3D('',#18070,#14658,#14659);
#12527=AXIS2_PLACEMENT_3D('',#18071,#14660,#14661);
#12528=AXIS2_PLACEMENT_3D('',#18072,#14662,#14663);
#12529=AXIS2_PLACEMENT_3D('',#18074,#14664,#14665);
#12530=AXIS2_PLACEMENT_3D('',#18077,#14667,#14668);
#12531=AXIS2_PLACEMENT_3D('',#18078,#14669,#14670);
#12532=AXIS2_PLACEMENT_3D('',#18080,#14671,#14672);
#12533=AXIS2_PLACEMENT_3D('',#18083,#14674,#14675);
#12534=AXIS2_PLACEMENT_3D('',#18084,#14676,#14677);
#12535=AXIS2_PLACEMENT_3D('',#18085,#14678,#14679);
#12536=AXIS2_PLACEMENT_3D('',#18086,#14680,#14681);
#12537=AXIS2_PLACEMENT_3D('',#18087,#14682,#14683);
#12538=AXIS2_PLACEMENT_3D('',#18091,#14685,#14686);
#12539=AXIS2_PLACEMENT_3D('',#18092,#14687,#14688);
#12540=AXIS2_PLACEMENT_3D('',#18105,#14689,#14690);
#12541=AXIS2_PLACEMENT_3D('',#18146,#14692,#14693);
#12542=AXIS2_PLACEMENT_3D('',#18157,#14694,#14695);
#12543=AXIS2_PLACEMENT_3D('',#18159,#14697,#14698);
#12544=AXIS2_PLACEMENT_3D('',#18161,#14699,#14700);
#12545=AXIS2_PLACEMENT_3D('',#18164,#14702,#14703);
#12546=AXIS2_PLACEMENT_3D('',#18165,#14704,#14705);
#12547=AXIS2_PLACEMENT_3D('',#18167,#14706,#14707);
#12548=AXIS2_PLACEMENT_3D('',#18170,#14709,#14710);
#12549=AXIS2_PLACEMENT_3D('',#18171,#14711,#14712);
#12550=AXIS2_PLACEMENT_3D('',#18172,#14713,#14714);
#12551=AXIS2_PLACEMENT_3D('',#18173,#14715,#14716);
#12552=AXIS2_PLACEMENT_3D('',#18174,#14717,#14718);
#12553=AXIS2_PLACEMENT_3D('',#18176,#14719,#14720);
#12554=AXIS2_PLACEMENT_3D('',#18179,#14722,#14723);
#12555=AXIS2_PLACEMENT_3D('',#18180,#14724,#14725);
#12556=AXIS2_PLACEMENT_3D('',#18182,#14726,#14727);
#12557=AXIS2_PLACEMENT_3D('',#18185,#14729,#14730);
#12558=AXIS2_PLACEMENT_3D('',#18186,#14731,#14732);
#12559=AXIS2_PLACEMENT_3D('',#18187,#14733,#14734);
#12560=AXIS2_PLACEMENT_3D('',#18188,#14735,#14736);
#12561=AXIS2_PLACEMENT_3D('',#18189,#14737,#14738);
#12562=AXIS2_PLACEMENT_3D('',#18198,#14743,#14744);
#12563=AXIS2_PLACEMENT_3D('',#18204,#14748,#14749);
#12564=AXIS2_PLACEMENT_3D('',#18210,#14753,#14754);
#12565=AXIS2_PLACEMENT_3D('',#18213,#14755,#14756);
#12566=AXIS2_PLACEMENT_3D('',#18359,#14758,#14759);
#12567=AXIS2_PLACEMENT_3D('',#18505,#14761,#14762);
#12568=AXIS2_PLACEMENT_3D('',#18651,#14764,#14765);
#12569=AXIS2_PLACEMENT_3D('',#18797,#14767,#14768);
#12570=AXIS2_PLACEMENT_3D('',#18943,#14770,#14771);
#12571=AXIS2_PLACEMENT_3D('',#19089,#14773,#14774);
#12572=AXIS2_PLACEMENT_3D('',#19235,#14776,#14777);
#12573=AXIS2_PLACEMENT_3D('',#19381,#14779,#14780);
#12574=AXIS2_PLACEMENT_3D('',#19527,#14782,#14783);
#12575=AXIS2_PLACEMENT_3D('',#19673,#14785,#14786);
#12576=AXIS2_PLACEMENT_3D('',#19819,#14788,#14789);
#12577=AXIS2_PLACEMENT_3D('',#19965,#14791,#14792);
#12578=AXIS2_PLACEMENT_3D('',#20111,#14794,#14795);
#12579=AXIS2_PLACEMENT_3D('',#20257,#14797,#14798);
#12580=AXIS2_PLACEMENT_3D('',#20403,#14800,#14801);
#12581=AXIS2_PLACEMENT_3D('',#20549,#14803,#14804);
#12582=AXIS2_PLACEMENT_3D('',#20695,#14806,#14807);
#12583=AXIS2_PLACEMENT_3D('',#20841,#14809,#14810);
#12584=AXIS2_PLACEMENT_3D('',#20987,#14812,#14813);
#12585=AXIS2_PLACEMENT_3D('',#21131,#14815,#14816);
#12586=AXIS2_PLACEMENT_3D('',#21132,#14817,#14818);
#12587=AXIS2_PLACEMENT_3D('',#21133,#14819,#14820);
#12588=AXIS2_PLACEMENT_3D('',#21134,#14821,#14822);
#12589=AXIS2_PLACEMENT_3D('',#21136,#14823,#14824);
#12590=AXIS2_PLACEMENT_3D('',#21139,#14826,#14827);
#12591=AXIS2_PLACEMENT_3D('',#21140,#14828,#14829);
#12592=AXIS2_PLACEMENT_3D('',#21355,#14832,#14833);
#12593=AXIS2_PLACEMENT_3D('',#21571,#14837,#14838);
#12594=AXIS2_PLACEMENT_3D('',#21573,#14839,#14840);
#12595=AXIS2_PLACEMENT_3D('',#21787,#14843,#14844);
#12596=AXIS2_PLACEMENT_3D('',#22003,#14848,#14849);
#12597=AXIS2_PLACEMENT_3D('',#22005,#14850,#14851);
#12598=AXIS2_PLACEMENT_3D('',#22219,#14854,#14855);
#12599=AXIS2_PLACEMENT_3D('',#22435,#14859,#14860);
#12600=AXIS2_PLACEMENT_3D('',#22437,#14861,#14862);
#12601=AXIS2_PLACEMENT_3D('',#22651,#14865,#14866);
#12602=AXIS2_PLACEMENT_3D('',#22867,#14870,#14871);
#12603=AXIS2_PLACEMENT_3D('',#22869,#14872,#14873);
#12604=AXIS2_PLACEMENT_3D('',#23083,#14876,#14877);
#12605=AXIS2_PLACEMENT_3D('',#23299,#14881,#14882);
#12606=AXIS2_PLACEMENT_3D('',#23301,#14883,#14884);
#12607=AXIS2_PLACEMENT_3D('',#23515,#14887,#14888);
#12608=AXIS2_PLACEMENT_3D('',#23731,#14892,#14893);
#12609=AXIS2_PLACEMENT_3D('',#23733,#14894,#14895);
#12610=AXIS2_PLACEMENT_3D('',#23947,#14898,#14899);
#12611=AXIS2_PLACEMENT_3D('',#24163,#14903,#14904);
#12612=AXIS2_PLACEMENT_3D('',#24165,#14905,#14906);
#12613=AXIS2_PLACEMENT_3D('',#24379,#14909,#14910);
#12614=AXIS2_PLACEMENT_3D('',#24595,#14914,#14915);
#12615=AXIS2_PLACEMENT_3D('',#24597,#14916,#14917);
#12616=AXIS2_PLACEMENT_3D('',#24811,#14920,#14921);
#12617=AXIS2_PLACEMENT_3D('',#25027,#14925,#14926);
#12618=AXIS2_PLACEMENT_3D('',#25029,#14927,#14928);
#12619=AXIS2_PLACEMENT_3D('',#25243,#14931,#14932);
#12620=AXIS2_PLACEMENT_3D('',#25459,#14936,#14937);
#12621=AXIS2_PLACEMENT_3D('',#25461,#14938,#14939);
#12622=AXIS2_PLACEMENT_3D('',#25675,#14942,#14943);
#12623=AXIS2_PLACEMENT_3D('',#25891,#14947,#14948);
#12624=AXIS2_PLACEMENT_3D('',#25893,#14949,#14950);
#12625=AXIS2_PLACEMENT_3D('',#26107,#14953,#14954);
#12626=AXIS2_PLACEMENT_3D('',#26323,#14958,#14959);
#12627=AXIS2_PLACEMENT_3D('',#26325,#14960,#14961);
#12628=AXIS2_PLACEMENT_3D('',#26539,#14964,#14965);
#12629=AXIS2_PLACEMENT_3D('',#26755,#14969,#14970);
#12630=AXIS2_PLACEMENT_3D('',#26757,#14971,#14972);
#12631=AXIS2_PLACEMENT_3D('',#26971,#14975,#14976);
#12632=AXIS2_PLACEMENT_3D('',#27187,#14980,#14981);
#12633=AXIS2_PLACEMENT_3D('',#27189,#14982,#14983);
#12634=AXIS2_PLACEMENT_3D('',#27403,#14986,#14987);
#12635=AXIS2_PLACEMENT_3D('',#27619,#14991,#14992);
#12636=AXIS2_PLACEMENT_3D('',#27621,#14993,#14994);
#12637=AXIS2_PLACEMENT_3D('',#27835,#14997,#14998);
#12638=AXIS2_PLACEMENT_3D('',#28051,#15002,#15003);
#12639=AXIS2_PLACEMENT_3D('',#28053,#15004,#15005);
#12640=AXIS2_PLACEMENT_3D('',#28267,#15008,#15009);
#12641=AXIS2_PLACEMENT_3D('',#28483,#15013,#15014);
#12642=AXIS2_PLACEMENT_3D('',#28485,#15015,#15016);
#12643=AXIS2_PLACEMENT_3D('',#28699,#15019,#15020);
#12644=AXIS2_PLACEMENT_3D('',#28915,#15024,#15025);
#12645=AXIS2_PLACEMENT_3D('',#28917,#15026,#15027);
#12646=AXIS2_PLACEMENT_3D('',#29131,#15030,#15031);
#12647=AXIS2_PLACEMENT_3D('',#29347,#15035,#15036);
#12648=AXIS2_PLACEMENT_3D('',#29349,#15037,#15038);
#12649=AXIS2_PLACEMENT_3D('',#29563,#15041,#15042);
#12650=AXIS2_PLACEMENT_3D('',#29779,#15046,#15047);
#12651=AXIS2_PLACEMENT_3D('',#29780,#15048,#15049);
#12652=AXIS2_PLACEMENT_3D('',#29781,#15050,#15051);
#12653=AXIS2_PLACEMENT_3D('',#29782,#15052,#15053);
#12654=AXIS2_PLACEMENT_3D('',#29783,#15054,#15055);
#12655=AXIS2_PLACEMENT_3D('',#29792,#15060,#15061);
#12656=AXIS2_PLACEMENT_3D('',#29796,#15063,#15064);
#12657=AXIS2_PLACEMENT_3D('',#29797,#15065,#15066);
#12658=AXIS2_PLACEMENT_3D('',#29798,#15067,#15068);
#12659=AXIS2_PLACEMENT_3D('',#29804,#15072,#15073);
#12660=AXIS2_PLACEMENT_3D('',#29805,#15074,#15075);
#12661=AXIS2_PLACEMENT_3D('',#29806,#15076,#15077);
#12662=AXIS2_PLACEMENT_3D('',#29807,#15078,#15079);
#12663=AXIS2_PLACEMENT_3D('',#29811,#15081,#15082);
#12664=AXIS2_PLACEMENT_3D('',#29813,#15084,#15085);
#12665=AXIS2_PLACEMENT_3D('',#29817,#15088,#15089);
#12666=AXIS2_PLACEMENT_3D('',#29818,#15090,#15091);
#12667=AXIS2_PLACEMENT_3D('',#29824,#15095,#15096);
#12668=AXIS2_PLACEMENT_3D('',#29827,#15098,#15099);
#12669=AXIS2_PLACEMENT_3D('',#29828,#15100,#15101);
#12670=AXIS2_PLACEMENT_3D('',#29834,#15105,#15106);
#12671=AXIS2_PLACEMENT_3D('',#29835,#15107,#15108);
#12672=AXIS2_PLACEMENT_3D('',#29836,#15109,#15110);
#12673=AXIS2_PLACEMENT_3D('',#29837,#15111,#15112);
#12674=AXIS2_PLACEMENT_3D('',#29839,#15114,#15115);
#12675=AXIS2_PLACEMENT_3D('',#29840,#15116,#15117);
#12676=AXIS2_PLACEMENT_3D('',#29841,#15118,#15119);
#12677=AXIS2_PLACEMENT_3D('',#29842,#15120,#15121);
#12678=AXIS2_PLACEMENT_3D('',#29843,#15122,#15123);
#12679=AXIS2_PLACEMENT_3D('',#29852,#15128,#15129);
#12680=AXIS2_PLACEMENT_3D('',#29854,#15130,#15131);
#12681=AXIS2_PLACEMENT_3D('',#29858,#15134,#15135);
#12682=AXIS2_PLACEMENT_3D('',#29864,#15139,#15140);
#12683=AXIS2_PLACEMENT_3D('',#29866,#15142,#15143);
#12684=AXIS2_PLACEMENT_3D('',#29867,#15144,#15145);
#12685=AXIS2_PLACEMENT_3D('',#29868,#15146,#15147);
#12686=AXIS2_PLACEMENT_3D('',#29870,#15148,#15149);
#12687=AXIS2_PLACEMENT_3D('',#29873,#15151,#15152);
#12688=AXIS2_PLACEMENT_3D('',#29874,#15153,#15154);
#12689=AXIS2_PLACEMENT_3D('',#29875,#15155,#15156);
#12690=AXIS2_PLACEMENT_3D('',#29876,#15157,#15158);
#12691=AXIS2_PLACEMENT_3D('',#29877,#15159,#15160);
#12692=AXIS2_PLACEMENT_3D('',#29879,#15161,#15162);
#12693=AXIS2_PLACEMENT_3D('',#29882,#15164,#15165);
#12694=AXIS2_PLACEMENT_3D('',#29883,#15166,#15167);
#12695=AXIS2_PLACEMENT_3D('',#29885,#15168,#15169);
#12696=AXIS2_PLACEMENT_3D('',#29888,#15171,#15172);
#12697=AXIS2_PLACEMENT_3D('',#29889,#15173,#15174);
#12698=AXIS2_PLACEMENT_3D('',#29890,#15175,#15176);
#12699=AXIS2_PLACEMENT_3D('',#29891,#15177,#15178);
#12700=AXIS2_PLACEMENT_3D('',#29892,#15179,#15180);
#12701=AXIS2_PLACEMENT_3D('',#29894,#15181,#15182);
#12702=AXIS2_PLACEMENT_3D('',#29897,#15184,#15185);
#12703=AXIS2_PLACEMENT_3D('',#29898,#15186,#15187);
#12704=AXIS2_PLACEMENT_3D('',#29900,#15188,#15189);
#12705=AXIS2_PLACEMENT_3D('',#29903,#15191,#15192);
#12706=AXIS2_PLACEMENT_3D('',#29904,#15193,#15194);
#12707=AXIS2_PLACEMENT_3D('',#29905,#15195,#15196);
#12708=AXIS2_PLACEMENT_3D('',#29906,#15197,#15198);
#12709=AXIS2_PLACEMENT_3D('',#29907,#15199,#15200);
#12710=AXIS2_PLACEMENT_3D('',#29911,#15202,#15203);
#12711=AXIS2_PLACEMENT_3D('',#29912,#15204,#15205);
#12712=AXIS2_PLACEMENT_3D('',#29929,#15206,#15207);
#12713=AXIS2_PLACEMENT_3D('',#29970,#15209,#15210);
#12714=AXIS2_PLACEMENT_3D('',#29985,#15211,#15212);
#12715=AXIS2_PLACEMENT_3D('',#29987,#15214,#15215);
#12716=AXIS2_PLACEMENT_3D('',#29989,#15216,#15217);
#12717=AXIS2_PLACEMENT_3D('',#29992,#15219,#15220);
#12718=AXIS2_PLACEMENT_3D('',#29993,#15221,#15222);
#12719=AXIS2_PLACEMENT_3D('',#29995,#15223,#15224);
#12720=AXIS2_PLACEMENT_3D('',#29998,#15226,#15227);
#12721=AXIS2_PLACEMENT_3D('',#29999,#15228,#15229);
#12722=AXIS2_PLACEMENT_3D('',#30000,#15230,#15231);
#12723=AXIS2_PLACEMENT_3D('',#30001,#15232,#15233);
#12724=AXIS2_PLACEMENT_3D('',#30002,#15234,#15235);
#12725=AXIS2_PLACEMENT_3D('',#30004,#15236,#15237);
#12726=AXIS2_PLACEMENT_3D('',#30007,#15239,#15240);
#12727=AXIS2_PLACEMENT_3D('',#30008,#15241,#15242);
#12728=AXIS2_PLACEMENT_3D('',#30010,#15243,#15244);
#12729=AXIS2_PLACEMENT_3D('',#30013,#15246,#15247);
#12730=AXIS2_PLACEMENT_3D('',#30014,#15248,#15249);
#12731=AXIS2_PLACEMENT_3D('',#30015,#15250,#15251);
#12732=AXIS2_PLACEMENT_3D('',#30016,#15252,#15253);
#12733=AXIS2_PLACEMENT_3D('',#30017,#15254,#15255);
#12734=AXIS2_PLACEMENT_3D('',#30021,#15257,#15258);
#12735=AXIS2_PLACEMENT_3D('',#30022,#15259,#15260);
#12736=AXIS2_PLACEMENT_3D('',#30039,#15261,#15262);
#12737=AXIS2_PLACEMENT_3D('',#30080,#15264,#15265);
#12738=AXIS2_PLACEMENT_3D('',#30095,#15266,#15267);
#12739=AXIS2_PLACEMENT_3D('',#30097,#15269,#15270);
#12740=AXIS2_PLACEMENT_3D('',#30099,#15271,#15272);
#12741=AXIS2_PLACEMENT_3D('',#30102,#15274,#15275);
#12742=AXIS2_PLACEMENT_3D('',#30103,#15276,#15277);
#12743=AXIS2_PLACEMENT_3D('',#30105,#15278,#15279);
#12744=AXIS2_PLACEMENT_3D('',#30108,#15281,#15282);
#12745=AXIS2_PLACEMENT_3D('',#30109,#15283,#15284);
#12746=AXIS2_PLACEMENT_3D('',#30110,#15285,#15286);
#12747=AXIS2_PLACEMENT_3D('',#30111,#15287,#15288);
#12748=AXIS2_PLACEMENT_3D('',#30112,#15289,#15290);
#12749=AXIS2_PLACEMENT_3D('',#30114,#15291,#15292);
#12750=AXIS2_PLACEMENT_3D('',#30117,#15294,#15295);
#12751=AXIS2_PLACEMENT_3D('',#30118,#15296,#15297);
#12752=AXIS2_PLACEMENT_3D('',#30120,#15298,#15299);
#12753=AXIS2_PLACEMENT_3D('',#30123,#15301,#15302);
#12754=AXIS2_PLACEMENT_3D('',#30124,#15303,#15304);
#12755=AXIS2_PLACEMENT_3D('',#30125,#15305,#15306);
#12756=AXIS2_PLACEMENT_3D('',#30126,#15307,#15308);
#12757=AXIS2_PLACEMENT_3D('',#30127,#15309,#15310);
#12758=AXIS2_PLACEMENT_3D('',#30136,#15315,#15316);
#12759=AXIS2_PLACEMENT_3D('',#30142,#15320,#15321);
#12760=AXIS2_PLACEMENT_3D('',#30148,#15325,#15326);
#12761=AXIS2_PLACEMENT_3D('',#30151,#15327,#15328);
#12762=AXIS2_PLACEMENT_3D('',#30297,#15330,#15331);
#12763=AXIS2_PLACEMENT_3D('',#30443,#15333,#15334);
#12764=AXIS2_PLACEMENT_3D('',#30589,#15336,#15337);
#12765=AXIS2_PLACEMENT_3D('',#30735,#15339,#15340);
#12766=AXIS2_PLACEMENT_3D('',#30881,#15342,#15343);
#12767=AXIS2_PLACEMENT_3D('',#31027,#15345,#15346);
#12768=AXIS2_PLACEMENT_3D('',#31173,#15348,#15349);
#12769=AXIS2_PLACEMENT_3D('',#31319,#15351,#15352);
#12770=AXIS2_PLACEMENT_3D('',#31465,#15354,#15355);
#12771=AXIS2_PLACEMENT_3D('',#31611,#15357,#15358);
#12772=AXIS2_PLACEMENT_3D('',#31757,#15360,#15361);
#12773=AXIS2_PLACEMENT_3D('',#31903,#15363,#15364);
#12774=AXIS2_PLACEMENT_3D('',#32049,#15366,#15367);
#12775=AXIS2_PLACEMENT_3D('',#32195,#15369,#15370);
#12776=AXIS2_PLACEMENT_3D('',#32341,#15372,#15373);
#12777=AXIS2_PLACEMENT_3D('',#32487,#15375,#15376);
#12778=AXIS2_PLACEMENT_3D('',#32633,#15378,#15379);
#12779=AXIS2_PLACEMENT_3D('',#32779,#15381,#15382);
#12780=AXIS2_PLACEMENT_3D('',#32925,#15384,#15385);
#12781=AXIS2_PLACEMENT_3D('',#33071,#15387,#15388);
#12782=AXIS2_PLACEMENT_3D('',#33217,#15390,#15391);
#12783=AXIS2_PLACEMENT_3D('',#33363,#15393,#15394);
#12784=AXIS2_PLACEMENT_3D('',#33509,#15396,#15397);
#12785=AXIS2_PLACEMENT_3D('',#33655,#15399,#15400);
#12786=AXIS2_PLACEMENT_3D('',#33801,#15402,#15403);
#12787=AXIS2_PLACEMENT_3D('',#33947,#15405,#15406);
#12788=AXIS2_PLACEMENT_3D('',#34093,#15408,#15409);
#12789=AXIS2_PLACEMENT_3D('',#34239,#15411,#15412);
#12790=AXIS2_PLACEMENT_3D('',#34385,#15414,#15415);
#12791=AXIS2_PLACEMENT_3D('',#34531,#15417,#15418);
#12792=AXIS2_PLACEMENT_3D('',#34677,#15420,#15421);
#12793=AXIS2_PLACEMENT_3D('',#34823,#15423,#15424);
#12794=AXIS2_PLACEMENT_3D('',#34969,#15426,#15427);
#12795=AXIS2_PLACEMENT_3D('',#35115,#15429,#15430);
#12796=AXIS2_PLACEMENT_3D('',#35261,#15432,#15433);
#12797=AXIS2_PLACEMENT_3D('',#35407,#15435,#15436);
#12798=AXIS2_PLACEMENT_3D('',#35553,#15438,#15439);
#12799=AXIS2_PLACEMENT_3D('',#35699,#15441,#15442);
#12800=AXIS2_PLACEMENT_3D('',#35845,#15444,#15445);
#12801=AXIS2_PLACEMENT_3D('',#35989,#15447,#15448);
#12802=AXIS2_PLACEMENT_3D('',#35990,#15449,#15450);
#12803=AXIS2_PLACEMENT_3D('',#35991,#15451,#15452);
#12804=AXIS2_PLACEMENT_3D('',#35992,#15453,#15454);
#12805=AXIS2_PLACEMENT_3D('',#35994,#15455,#15456);
#12806=AXIS2_PLACEMENT_3D('',#35997,#15458,#15459);
#12807=AXIS2_PLACEMENT_3D('',#35998,#15460,#15461);
#12808=AXIS2_PLACEMENT_3D('',#36437,#15464,#15465);
#12809=AXIS2_PLACEMENT_3D('',#36439,#15467,#15468);
#12810=AXIS2_PLACEMENT_3D('',#36441,#15469,#15470);
#12811=AXIS2_PLACEMENT_3D('',#36879,#15473,#15474);
#12812=AXIS2_PLACEMENT_3D('',#36881,#15476,#15477);
#12813=AXIS2_PLACEMENT_3D('',#36883,#15478,#15479);
#12814=AXIS2_PLACEMENT_3D('',#37321,#15482,#15483);
#12815=AXIS2_PLACEMENT_3D('',#37323,#15485,#15486);
#12816=AXIS2_PLACEMENT_3D('',#37325,#15487,#15488);
#12817=AXIS2_PLACEMENT_3D('',#37763,#15491,#15492);
#12818=AXIS2_PLACEMENT_3D('',#37765,#15494,#15495);
#12819=AXIS2_PLACEMENT_3D('',#37767,#15496,#15497);
#12820=AXIS2_PLACEMENT_3D('',#38205,#15500,#15501);
#12821=AXIS2_PLACEMENT_3D('',#38207,#15503,#15504);
#12822=AXIS2_PLACEMENT_3D('',#38209,#15505,#15506);
#12823=AXIS2_PLACEMENT_3D('',#38647,#15509,#15510);
#12824=AXIS2_PLACEMENT_3D('',#38649,#15512,#15513);
#12825=AXIS2_PLACEMENT_3D('',#38651,#15514,#15515);
#12826=AXIS2_PLACEMENT_3D('',#39089,#15518,#15519);
#12827=AXIS2_PLACEMENT_3D('',#39091,#15521,#15522);
#12828=AXIS2_PLACEMENT_3D('',#39093,#15523,#15524);
#12829=AXIS2_PLACEMENT_3D('',#39531,#15527,#15528);
#12830=AXIS2_PLACEMENT_3D('',#39533,#15530,#15531);
#12831=AXIS2_PLACEMENT_3D('',#39535,#15532,#15533);
#12832=AXIS2_PLACEMENT_3D('',#39973,#15536,#15537);
#12833=AXIS2_PLACEMENT_3D('',#39975,#15539,#15540);
#12834=AXIS2_PLACEMENT_3D('',#39977,#15541,#15542);
#12835=AXIS2_PLACEMENT_3D('',#40415,#15545,#15546);
#12836=AXIS2_PLACEMENT_3D('',#40417,#15548,#15549);
#12837=AXIS2_PLACEMENT_3D('',#40419,#15550,#15551);
#12838=AXIS2_PLACEMENT_3D('',#40857,#15554,#15555);
#12839=AXIS2_PLACEMENT_3D('',#40859,#15557,#15558);
#12840=AXIS2_PLACEMENT_3D('',#40861,#15559,#15560);
#12841=AXIS2_PLACEMENT_3D('',#41299,#15563,#15564);
#12842=AXIS2_PLACEMENT_3D('',#41301,#15566,#15567);
#12843=AXIS2_PLACEMENT_3D('',#41303,#15568,#15569);
#12844=AXIS2_PLACEMENT_3D('',#41741,#15572,#15573);
#12845=AXIS2_PLACEMENT_3D('',#41743,#15575,#15576);
#12846=AXIS2_PLACEMENT_3D('',#41745,#15577,#15578);
#12847=AXIS2_PLACEMENT_3D('',#42183,#15581,#15582);
#12848=AXIS2_PLACEMENT_3D('',#42185,#15584,#15585);
#12849=AXIS2_PLACEMENT_3D('',#42187,#15586,#15587);
#12850=AXIS2_PLACEMENT_3D('',#42625,#15590,#15591);
#12851=AXIS2_PLACEMENT_3D('',#42627,#15593,#15594);
#12852=AXIS2_PLACEMENT_3D('',#42629,#15595,#15596);
#12853=AXIS2_PLACEMENT_3D('',#43067,#15599,#15600);
#12854=AXIS2_PLACEMENT_3D('',#43069,#15602,#15603);
#12855=AXIS2_PLACEMENT_3D('',#43071,#15604,#15605);
#12856=AXIS2_PLACEMENT_3D('',#43509,#15608,#15609);
#12857=AXIS2_PLACEMENT_3D('',#43511,#15611,#15612);
#12858=AXIS2_PLACEMENT_3D('',#43513,#15613,#15614);
#12859=AXIS2_PLACEMENT_3D('',#43951,#15617,#15618);
#12860=AXIS2_PLACEMENT_3D('',#43953,#15620,#15621);
#12861=AXIS2_PLACEMENT_3D('',#43955,#15622,#15623);
#12862=AXIS2_PLACEMENT_3D('',#44393,#15626,#15627);
#12863=AXIS2_PLACEMENT_3D('',#44395,#15629,#15630);
#12864=AXIS2_PLACEMENT_3D('',#44397,#15631,#15632);
#12865=AXIS2_PLACEMENT_3D('',#44835,#15635,#15636);
#12866=AXIS2_PLACEMENT_3D('',#44837,#15638,#15639);
#12867=AXIS2_PLACEMENT_3D('',#44839,#15640,#15641);
#12868=AXIS2_PLACEMENT_3D('',#45277,#15644,#15645);
#12869=AXIS2_PLACEMENT_3D('',#45279,#15647,#15648);
#12870=AXIS2_PLACEMENT_3D('',#45281,#15649,#15650);
#12871=AXIS2_PLACEMENT_3D('',#45719,#15653,#15654);
#12872=AXIS2_PLACEMENT_3D('',#45721,#15656,#15657);
#12873=AXIS2_PLACEMENT_3D('',#45723,#15658,#15659);
#12874=AXIS2_PLACEMENT_3D('',#46161,#15662,#15663);
#12875=AXIS2_PLACEMENT_3D('',#46163,#15665,#15666);
#12876=AXIS2_PLACEMENT_3D('',#46165,#15667,#15668);
#12877=AXIS2_PLACEMENT_3D('',#46603,#15671,#15672);
#12878=AXIS2_PLACEMENT_3D('',#46605,#15674,#15675);
#12879=AXIS2_PLACEMENT_3D('',#46607,#15676,#15677);
#12880=AXIS2_PLACEMENT_3D('',#47045,#15680,#15681);
#12881=AXIS2_PLACEMENT_3D('',#47047,#15683,#15684);
#12882=AXIS2_PLACEMENT_3D('',#47049,#15685,#15686);
#12883=AXIS2_PLACEMENT_3D('',#47487,#15689,#15690);
#12884=AXIS2_PLACEMENT_3D('',#47489,#15692,#15693);
#12885=AXIS2_PLACEMENT_3D('',#47491,#15694,#15695);
#12886=AXIS2_PLACEMENT_3D('',#47929,#15698,#15699);
#12887=AXIS2_PLACEMENT_3D('',#47931,#15701,#15702);
#12888=AXIS2_PLACEMENT_3D('',#47933,#15703,#15704);
#12889=AXIS2_PLACEMENT_3D('',#48371,#15707,#15708);
#12890=AXIS2_PLACEMENT_3D('',#48373,#15710,#15711);
#12891=AXIS2_PLACEMENT_3D('',#48375,#15712,#15713);
#12892=AXIS2_PLACEMENT_3D('',#48813,#15716,#15717);
#12893=AXIS2_PLACEMENT_3D('',#48815,#15719,#15720);
#12894=AXIS2_PLACEMENT_3D('',#48817,#15721,#15722);
#12895=AXIS2_PLACEMENT_3D('',#49255,#15725,#15726);
#12896=AXIS2_PLACEMENT_3D('',#49257,#15728,#15729);
#12897=AXIS2_PLACEMENT_3D('',#49259,#15730,#15731);
#12898=AXIS2_PLACEMENT_3D('',#49697,#15734,#15735);
#12899=AXIS2_PLACEMENT_3D('',#49699,#15737,#15738);
#12900=AXIS2_PLACEMENT_3D('',#49701,#15739,#15740);
#12901=AXIS2_PLACEMENT_3D('',#50139,#15743,#15744);
#12902=AXIS2_PLACEMENT_3D('',#50141,#15746,#15747);
#12903=AXIS2_PLACEMENT_3D('',#50143,#15748,#15749);
#12904=AXIS2_PLACEMENT_3D('',#50581,#15752,#15753);
#12905=AXIS2_PLACEMENT_3D('',#50583,#15755,#15756);
#12906=AXIS2_PLACEMENT_3D('',#50585,#15757,#15758);
#12907=AXIS2_PLACEMENT_3D('',#51023,#15761,#15762);
#12908=AXIS2_PLACEMENT_3D('',#51025,#15764,#15765);
#12909=AXIS2_PLACEMENT_3D('',#51027,#15766,#15767);
#12910=AXIS2_PLACEMENT_3D('',#51465,#15770,#15771);
#12911=AXIS2_PLACEMENT_3D('',#51467,#15773,#15774);
#12912=AXIS2_PLACEMENT_3D('',#51469,#15775,#15776);
#12913=AXIS2_PLACEMENT_3D('',#51907,#15779,#15780);
#12914=AXIS2_PLACEMENT_3D('',#51909,#15782,#15783);
#12915=AXIS2_PLACEMENT_3D('',#51911,#15784,#15785);
#12916=AXIS2_PLACEMENT_3D('',#52349,#15788,#15789);
#12917=AXIS2_PLACEMENT_3D('',#52351,#15791,#15792);
#12918=AXIS2_PLACEMENT_3D('',#52353,#15793,#15794);
#12919=AXIS2_PLACEMENT_3D('',#52791,#15797,#15798);
#12920=AXIS2_PLACEMENT_3D('',#52793,#15800,#15801);
#12921=AXIS2_PLACEMENT_3D('',#52795,#15802,#15803);
#12922=AXIS2_PLACEMENT_3D('',#53014,#15805,#15806);
#12923=AXIS2_PLACEMENT_3D('',#53235,#15809,#15810);
#12924=AXIS2_PLACEMENT_3D('',#53237,#15811,#15812);
#12925=AXIS2_PLACEMENT_3D('',#53675,#15815,#15816);
#12926=AXIS2_PLACEMENT_3D('',#53677,#15818,#15819);
#12927=AXIS2_PLACEMENT_3D('',#53678,#15820,#15821);
#12928=AXIS2_PLACEMENT_3D('',#53679,#15822,#15823);
#12929=AXIS2_PLACEMENT_3D('',#53680,#15824,#15825);
#12930=AXIS2_PLACEMENT_3D('',#53681,#15826,#15827);
#12931=AXIS2_PLACEMENT_3D('',#53698,#15836,#15837);
#12932=AXIS2_PLACEMENT_3D('',#53704,#15841,#15842);
#12933=AXIS2_PLACEMENT_3D('',#53708,#15845,#15846);
#12934=AXIS2_PLACEMENT_3D('',#53712,#15849,#15850);
#12935=AXIS2_PLACEMENT_3D('',#53716,#15853,#15854);
#12936=AXIS2_PLACEMENT_3D('',#53724,#15859,#15860);
#12937=AXIS2_PLACEMENT_3D('',#53726,#15862,#15863);
#12938=AXIS2_PLACEMENT_3D('',#53728,#15865,#15866);
#12939=AXIS2_PLACEMENT_3D('',#53730,#15868,#15869);
#12940=AXIS2_PLACEMENT_3D('',#53731,#15870,#15871);
#12941=AXIS2_PLACEMENT_3D('',#53732,#15872,#15873);
#12942=AXIS2_PLACEMENT_3D('',#53741,#15878,#15879);
#12943=AXIS2_PLACEMENT_3D('',#53747,#15883,#15884);
#12944=AXIS2_PLACEMENT_3D('',#53753,#15888,#15889);
#12945=AXIS2_PLACEMENT_3D('',#53759,#15893,#15894);
#12946=AXIS2_PLACEMENT_3D('',#53765,#15898,#15899);
#12947=AXIS2_PLACEMENT_3D('',#53768,#15902,#15903);
#12948=AXIS2_PLACEMENT_3D('',#53769,#15904,#15905);
#12949=AXIS2_PLACEMENT_3D('',#53771,#15906,#15907);
#12950=AXIS2_PLACEMENT_3D('',#53772,#15908,#15909);
#12951=AXIS2_PLACEMENT_3D('',#53774,#15910,#15911);
#12952=AXIS2_PLACEMENT_3D('',#53776,#15913,#15914);
#12953=AXIS2_PLACEMENT_3D('',#53778,#15915,#15916);
#12954=AXIS2_PLACEMENT_3D('',#53780,#15918,#15919);
#12955=AXIS2_PLACEMENT_3D('',#53782,#15920,#15921);
#12956=AXIS2_PLACEMENT_3D('',#53784,#15923,#15924);
#12957=AXIS2_PLACEMENT_3D('',#53785,#15925,#15926);
#12958=AXIS2_PLACEMENT_3D('',#53786,#15927,#15928);
#12959=AXIS2_PLACEMENT_3D('',#53787,#15929,#15930);
#12960=AXIS2_PLACEMENT_3D('',#53788,#15931,#15932);
#12961=AXIS2_PLACEMENT_3D('',#53789,#15933,#15934);
#12962=AXIS2_PLACEMENT_3D('',#53790,#15935,#15936);
#12963=AXIS2_PLACEMENT_3D('',#53791,#15937,#15938);
#12964=AXIS2_PLACEMENT_3D('',#53792,#15939,#15940);
#12965=AXIS2_PLACEMENT_3D('',#53793,#15941,#15942);
#12966=AXIS2_PLACEMENT_3D('',#53794,#15943,#15944);
#12967=AXIS2_PLACEMENT_3D('',#53795,#15945,#15946);
#12968=AXIS2_PLACEMENT_3D('',#53796,#15947,#15948);
#12969=AXIS2_PLACEMENT_3D('',#53797,#15949,#15950);
#12970=AXIS2_PLACEMENT_3D('',#53798,#15951,#15952);
#12971=AXIS2_PLACEMENT_3D('',#53799,#15953,#15954);
#12972=AXIS2_PLACEMENT_3D('',#53800,#15955,#15956);
#12973=AXIS2_PLACEMENT_3D('',#53801,#15957,#15958);
#12974=AXIS2_PLACEMENT_3D('',#53802,#15959,#15960);
#12975=AXIS2_PLACEMENT_3D('',#53803,#15961,#15962);
#12976=AXIS2_PLACEMENT_3D('',#53804,#15963,#15964);
#12977=AXIS2_PLACEMENT_3D('',#53805,#15965,#15966);
#12978=AXIS2_PLACEMENT_3D('',#53806,#15967,#15968);
#12979=AXIS2_PLACEMENT_3D('',#53807,#15969,#15970);
#12980=AXIS2_PLACEMENT_3D('',#53808,#15971,#15972);
#12981=AXIS2_PLACEMENT_3D('',#53809,#15973,#15974);
#12982=DIRECTION('axis',(0.,0.,1.));
#12983=DIRECTION('refdir',(1.,0.,0.));
#12984=DIRECTION('axis',(0.,0.,1.));
#12985=DIRECTION('refdir',(1.,0.,0.));
#12986=DIRECTION('axis',(0.,0.,1.));
#12987=DIRECTION('refdir',(1.,0.,0.));
#12988=DIRECTION('center_axis',(0.,0.,1.));
#12989=DIRECTION('ref_axis',(1.,0.,0.));
#12990=DIRECTION('center_axis',(0.,0.,1.));
#12991=DIRECTION('ref_axis',(1.,0.,0.));
#12992=DIRECTION('',(0.,0.,1.));
#12993=DIRECTION('center_axis',(0.,0.,-1.));
#12994=DIRECTION('ref_axis',(1.,0.,0.));
#12995=DIRECTION('center_axis',(0.,0.,1.));
#12996=DIRECTION('ref_axis',(1.,0.,0.));
#12997=DIRECTION('center_axis',(0.,0.,1.));
#12998=DIRECTION('ref_axis',(1.,0.,0.));
#12999=DIRECTION('',(0.,0.,1.));
#13000=DIRECTION('center_axis',(0.,0.,-1.));
#13001=DIRECTION('ref_axis',(1.,0.,0.));
#13002=DIRECTION('center_axis',(0.,0.,1.));
#13003=DIRECTION('ref_axis',(1.,0.,0.));
#13004=DIRECTION('center_axis',(0.,0.,1.));
#13005=DIRECTION('ref_axis',(1.,0.,0.));
#13006=DIRECTION('',(0.,0.,1.));
#13007=DIRECTION('center_axis',(0.,0.,-1.));
#13008=DIRECTION('ref_axis',(1.,0.,0.));
#13009=DIRECTION('center_axis',(0.,0.,1.));
#13010=DIRECTION('ref_axis',(1.,0.,0.));
#13011=DIRECTION('center_axis',(0.,0.,1.));
#13012=DIRECTION('ref_axis',(1.,0.,0.));
#13013=DIRECTION('',(0.,0.,1.));
#13014=DIRECTION('center_axis',(0.,0.,-1.));
#13015=DIRECTION('ref_axis',(1.,0.,0.));
#13016=DIRECTION('center_axis',(0.,1.,0.));
#13017=DIRECTION('ref_axis',(-1.,0.,0.));
#13018=DIRECTION('',(-1.,0.,0.));
#13019=DIRECTION('',(0.,0.,1.));
#13020=DIRECTION('',(-1.,0.,0.));
#13021=DIRECTION('',(0.,0.,1.));
#13022=DIRECTION('center_axis',(1.,0.,0.));
#13023=DIRECTION('ref_axis',(0.,1.,0.));
#13024=DIRECTION('',(0.,1.,0.));
#13025=DIRECTION('',(0.,1.,0.));
#13026=DIRECTION('',(0.,0.,1.));
#13027=DIRECTION('center_axis',(0.,-1.,0.));
#13028=DIRECTION('ref_axis',(1.,0.,0.));
#13029=DIRECTION('',(1.,0.,0.));
#13030=DIRECTION('',(1.,0.,0.));
#13031=DIRECTION('',(0.,0.,1.));
#13032=DIRECTION('center_axis',(-1.,0.,0.));
#13033=DIRECTION('ref_axis',(0.,-1.,0.));
#13034=DIRECTION('',(0.,-1.,0.));
#13035=DIRECTION('',(0.,-1.,0.));
#13036=DIRECTION('center_axis',(0.,0.,1.));
#13037=DIRECTION('ref_axis',(1.,0.,0.));
#13038=DIRECTION('center_axis',(0.,0.,1.));
#13039=DIRECTION('ref_axis',(1.,0.,0.));
#13040=DIRECTION('axis',(0.,0.,1.));
#13041=DIRECTION('refdir',(1.,0.,0.));
#13042=DIRECTION('center_axis',(0.,1.,0.));
#13043=DIRECTION('ref_axis',(1.,0.,0.));
#13044=DIRECTION('center_axis',(0.,1.,0.));
#13045=DIRECTION('ref_axis',(1.,0.,0.));
#13046=DIRECTION('',(0.,1.,0.));
#13047=DIRECTION('center_axis',(0.,-1.,0.));
#13048=DIRECTION('ref_axis',(1.,0.,0.));
#13049=DIRECTION('center_axis',(0.,1.,0.));
#13050=DIRECTION('ref_axis',(1.,0.,0.));
#13051=DIRECTION('center_axis',(0.,1.,0.));
#13052=DIRECTION('ref_axis',(1.,0.,0.));
#13053=DIRECTION('',(0.,1.,0.));
#13054=DIRECTION('center_axis',(0.,-1.,0.));
#13055=DIRECTION('ref_axis',(1.,0.,0.));
#13056=DIRECTION('center_axis',(0.,1.,0.));
#13057=DIRECTION('ref_axis',(1.,0.,0.));
#13058=DIRECTION('center_axis',(0.,1.,0.));
#13059=DIRECTION('ref_axis',(1.,0.,0.));
#13060=DIRECTION('',(0.,1.,0.));
#13061=DIRECTION('center_axis',(0.,-1.,0.));
#13062=DIRECTION('ref_axis',(1.,0.,0.));
#13063=DIRECTION('center_axis',(0.,1.,0.));
#13064=DIRECTION('ref_axis',(1.,0.,0.));
#13065=DIRECTION('center_axis',(0.,1.,0.));
#13066=DIRECTION('ref_axis',(1.,0.,0.));
#13067=DIRECTION('',(0.,1.,0.));
#13068=DIRECTION('center_axis',(0.,-1.,0.));
#13069=DIRECTION('ref_axis',(1.,0.,0.));
#13070=DIRECTION('center_axis',(0.,1.,0.));
#13071=DIRECTION('ref_axis',(1.,0.,0.));
#13072=DIRECTION('center_axis',(0.,1.,0.));
#13073=DIRECTION('ref_axis',(1.,0.,0.));
#13074=DIRECTION('',(0.,1.,0.));
#13075=DIRECTION('center_axis',(0.,-1.,0.));
#13076=DIRECTION('ref_axis',(1.,0.,0.));
#13077=DIRECTION('center_axis',(0.,1.,0.));
#13078=DIRECTION('ref_axis',(1.,0.,0.));
#13079=DIRECTION('center_axis',(0.,1.,0.));
#13080=DIRECTION('ref_axis',(1.,0.,0.));
#13081=DIRECTION('',(0.,1.,0.));
#13082=DIRECTION('center_axis',(0.,-1.,0.));
#13083=DIRECTION('ref_axis',(1.,0.,0.));
#13084=DIRECTION('center_axis',(0.,1.,0.));
#13085=DIRECTION('ref_axis',(1.,0.,0.));
#13086=DIRECTION('center_axis',(0.,1.,0.));
#13087=DIRECTION('ref_axis',(1.,0.,0.));
#13088=DIRECTION('',(0.,1.,0.));
#13089=DIRECTION('center_axis',(0.,1.,0.));
#13090=DIRECTION('ref_axis',(1.,0.,0.));
#13091=DIRECTION('center_axis',(0.,1.,0.));
#13092=DIRECTION('ref_axis',(1.,0.,0.));
#13093=DIRECTION('center_axis',(0.,-1.,0.));
#13094=DIRECTION('ref_axis',(1.,0.,0.));
#13095=DIRECTION('center_axis',(0.,1.,0.));
#13096=DIRECTION('ref_axis',(1.,0.,0.));
#13097=DIRECTION('center_axis',(0.,1.,0.));
#13098=DIRECTION('ref_axis',(1.,0.,0.));
#13099=DIRECTION('',(0.,1.,0.));
#13100=DIRECTION('center_axis',(0.,1.,0.));
#13101=DIRECTION('ref_axis',(1.,0.,0.));
#13102=DIRECTION('center_axis',(0.,1.,0.));
#13103=DIRECTION('ref_axis',(1.,0.,0.));
#13104=DIRECTION('center_axis',(0.,-1.,0.));
#13105=DIRECTION('ref_axis',(1.,0.,0.));
#13106=DIRECTION('center_axis',(0.,1.,0.));
#13107=DIRECTION('ref_axis',(1.,0.,0.));
#13108=DIRECTION('center_axis',(0.,1.,0.));
#13109=DIRECTION('ref_axis',(1.,0.,0.));
#13110=DIRECTION('',(0.,1.,0.));
#13111=DIRECTION('center_axis',(0.,1.,0.));
#13112=DIRECTION('ref_axis',(1.,0.,0.));
#13113=DIRECTION('center_axis',(0.,1.,0.));
#13114=DIRECTION('ref_axis',(1.,0.,0.));
#13115=DIRECTION('center_axis',(0.,-1.,0.));
#13116=DIRECTION('ref_axis',(1.,0.,0.));
#13117=DIRECTION('center_axis',(0.,1.,0.));
#13118=DIRECTION('ref_axis',(1.,0.,0.));
#13119=DIRECTION('center_axis',(0.,1.,0.));
#13120=DIRECTION('ref_axis',(1.,0.,0.));
#13121=DIRECTION('',(0.,1.,0.));
#13122=DIRECTION('center_axis',(0.,1.,0.));
#13123=DIRECTION('ref_axis',(1.,0.,0.));
#13124=DIRECTION('center_axis',(0.,1.,0.));
#13125=DIRECTION('ref_axis',(1.,0.,0.));
#13126=DIRECTION('center_axis',(0.,-1.,0.));
#13127=DIRECTION('ref_axis',(1.,0.,0.));
#13128=DIRECTION('center_axis',(0.,1.,0.));
#13129=DIRECTION('ref_axis',(1.,0.,0.));
#13130=DIRECTION('',(0.,1.,0.));
#13131=DIRECTION('center_axis',(0.,-1.,0.));
#13132=DIRECTION('ref_axis',(1.,0.,0.));
#13133=DIRECTION('center_axis',(0.,1.,0.));
#13134=DIRECTION('ref_axis',(1.,0.,0.));
#13135=DIRECTION('',(0.,1.,0.));
#13136=DIRECTION('center_axis',(0.,-1.,0.));
#13137=DIRECTION('ref_axis',(1.,0.,0.));
#13138=DIRECTION('center_axis',(0.,1.,0.));
#13139=DIRECTION('ref_axis',(1.,0.,0.));
#13140=DIRECTION('',(0.,1.,0.));
#13141=DIRECTION('center_axis',(0.,-1.,0.));
#13142=DIRECTION('ref_axis',(1.,0.,0.));
#13143=DIRECTION('center_axis',(0.,1.,0.));
#13144=DIRECTION('ref_axis',(1.,0.,0.));
#13145=DIRECTION('',(0.,1.,0.));
#13146=DIRECTION('center_axis',(0.,-1.,0.));
#13147=DIRECTION('ref_axis',(1.,0.,0.));
#13148=DIRECTION('center_axis',(0.,0.,1.));
#13149=DIRECTION('ref_axis',(1.,0.,0.));
#13150=DIRECTION('center_axis',(0.,0.,1.));
#13151=DIRECTION('ref_axis',(1.,0.,0.));
#13152=DIRECTION('',(0.,0.,1.));
#13153=DIRECTION('center_axis',(0.,0.,1.));
#13154=DIRECTION('ref_axis',(1.,0.,0.));
#13155=DIRECTION('center_axis',(0.,0.,1.));
#13156=DIRECTION('ref_axis',(1.,0.,0.));
#13157=DIRECTION('center_axis',(0.,0.,1.));
#13158=DIRECTION('ref_axis',(1.,0.,0.));
#13159=DIRECTION('center_axis',(0.,0.,1.));
#13160=DIRECTION('ref_axis',(1.,0.,0.));
#13161=DIRECTION('',(0.,0.,1.));
#13162=DIRECTION('center_axis',(0.,0.,1.));
#13163=DIRECTION('ref_axis',(1.,0.,0.));
#13164=DIRECTION('center_axis',(0.,0.,1.));
#13165=DIRECTION('ref_axis',(1.,0.,0.));
#13166=DIRECTION('center_axis',(0.,1.,0.));
#13167=DIRECTION('ref_axis',(1.,0.,0.));
#13168=DIRECTION('center_axis',(0.,1.,0.));
#13169=DIRECTION('ref_axis',(1.,0.,0.));
#13170=DIRECTION('',(0.,1.,0.));
#13171=DIRECTION('center_axis',(0.,1.,0.));
#13172=DIRECTION('ref_axis',(1.,0.,0.));
#13173=DIRECTION('center_axis',(0.,1.,0.));
#13174=DIRECTION('ref_axis',(1.,0.,0.));
#13175=DIRECTION('center_axis',(0.,-1.,0.));
#13176=DIRECTION('ref_axis',(1.,0.,0.));
#13177=DIRECTION('center_axis',(0.,1.,0.));
#13178=DIRECTION('ref_axis',(1.,0.,0.));
#13179=DIRECTION('',(0.,1.,0.));
#13180=DIRECTION('center_axis',(0.,-1.,0.));
#13181=DIRECTION('ref_axis',(1.,0.,0.));
#13182=DIRECTION('center_axis',(0.,1.,0.));
#13183=DIRECTION('ref_axis',(1.,0.,0.));
#13184=DIRECTION('center_axis',(0.,1.,0.));
#13185=DIRECTION('ref_axis',(1.,0.,0.));
#13186=DIRECTION('',(0.,1.,0.));
#13187=DIRECTION('center_axis',(0.,1.,0.));
#13188=DIRECTION('ref_axis',(1.,0.,0.));
#13189=DIRECTION('center_axis',(0.,1.,0.));
#13190=DIRECTION('ref_axis',(1.,0.,0.));
#13191=DIRECTION('center_axis',(0.,-1.,0.));
#13192=DIRECTION('ref_axis',(1.,0.,0.));
#13193=DIRECTION('center_axis',(0.,1.,0.));
#13194=DIRECTION('ref_axis',(1.,0.,0.));
#13195=DIRECTION('',(0.,1.,0.));
#13196=DIRECTION('center_axis',(0.,-1.,0.));
#13197=DIRECTION('ref_axis',(1.,0.,0.));
#13198=DIRECTION('center_axis',(0.,1.,0.));
#13199=DIRECTION('ref_axis',(-1.,0.,0.));
#13200=DIRECTION('',(-1.,0.,0.));
#13201=DIRECTION('',(0.,0.,1.));
#13202=DIRECTION('',(-1.,0.,0.));
#13203=DIRECTION('',(0.,0.,1.));
#13204=DIRECTION('center_axis',(1.,0.,0.));
#13205=DIRECTION('ref_axis',(0.,1.,0.));
#13206=DIRECTION('',(0.,1.,0.));
#13207=DIRECTION('',(0.,1.,0.));
#13208=DIRECTION('',(0.,0.,1.));
#13209=DIRECTION('center_axis',(0.,-1.,0.));
#13210=DIRECTION('ref_axis',(1.,0.,0.));
#13211=DIRECTION('',(1.,0.,0.));
#13212=DIRECTION('',(1.,0.,0.));
#13213=DIRECTION('',(0.,0.,1.));
#13214=DIRECTION('center_axis',(-1.,0.,0.));
#13215=DIRECTION('ref_axis',(0.,-1.,0.));
#13216=DIRECTION('',(0.,-1.,0.));
#13217=DIRECTION('',(0.,-1.,0.));
#13218=DIRECTION('center_axis',(0.,0.,1.));
#13219=DIRECTION('ref_axis',(1.,0.,0.));
#13220=DIRECTION('center_axis',(0.,0.,1.));
#13221=DIRECTION('ref_axis',(1.,0.,0.));
#13222=DIRECTION('axis',(0.,0.,1.));
#13223=DIRECTION('refdir',(1.,0.,0.));
#13224=DIRECTION('center_axis',(0.,1.,0.));
#13225=DIRECTION('ref_axis',(1.,0.,0.));
#13226=DIRECTION('center_axis',(0.,1.,0.));
#13227=DIRECTION('ref_axis',(1.,0.,0.));
#13228=DIRECTION('',(0.,1.,0.));
#13229=DIRECTION('center_axis',(0.,-1.,0.));
#13230=DIRECTION('ref_axis',(1.,0.,0.));
#13231=DIRECTION('center_axis',(0.,1.,0.));
#13232=DIRECTION('ref_axis',(1.,0.,0.));
#13233=DIRECTION('center_axis',(0.,1.,0.));
#13234=DIRECTION('ref_axis',(1.,0.,0.));
#13235=DIRECTION('',(0.,1.,0.));
#13236=DIRECTION('center_axis',(0.,-1.,0.));
#13237=DIRECTION('ref_axis',(1.,0.,0.));
#13238=DIRECTION('center_axis',(0.,1.,0.));
#13239=DIRECTION('ref_axis',(1.,0.,0.));
#13240=DIRECTION('center_axis',(0.,1.,0.));
#13241=DIRECTION('ref_axis',(1.,0.,0.));
#13242=DIRECTION('',(0.,1.,0.));
#13243=DIRECTION('center_axis',(0.,-1.,0.));
#13244=DIRECTION('ref_axis',(1.,0.,0.));
#13245=DIRECTION('center_axis',(0.,1.,0.));
#13246=DIRECTION('ref_axis',(1.,0.,0.));
#13247=DIRECTION('center_axis',(0.,1.,0.));
#13248=DIRECTION('ref_axis',(1.,0.,0.));
#13249=DIRECTION('',(0.,1.,0.));
#13250=DIRECTION('center_axis',(0.,-1.,0.));
#13251=DIRECTION('ref_axis',(1.,0.,0.));
#13252=DIRECTION('center_axis',(0.,1.,0.));
#13253=DIRECTION('ref_axis',(1.,0.,0.));
#13254=DIRECTION('center_axis',(0.,1.,0.));
#13255=DIRECTION('ref_axis',(1.,0.,0.));
#13256=DIRECTION('',(0.,1.,0.));
#13257=DIRECTION('center_axis',(0.,-1.,0.));
#13258=DIRECTION('ref_axis',(1.,0.,0.));
#13259=DIRECTION('center_axis',(0.,1.,0.));
#13260=DIRECTION('ref_axis',(1.,0.,0.));
#13261=DIRECTION('center_axis',(0.,1.,0.));
#13262=DIRECTION('ref_axis',(1.,0.,0.));
#13263=DIRECTION('',(0.,1.,0.));
#13264=DIRECTION('center_axis',(0.,-1.,0.));
#13265=DIRECTION('ref_axis',(1.,0.,0.));
#13266=DIRECTION('center_axis',(0.,1.,0.));
#13267=DIRECTION('ref_axis',(1.,0.,0.));
#13268=DIRECTION('center_axis',(0.,1.,0.));
#13269=DIRECTION('ref_axis',(1.,0.,0.));
#13270=DIRECTION('',(0.,1.,0.));
#13271=DIRECTION('center_axis',(0.,-1.,0.));
#13272=DIRECTION('ref_axis',(1.,0.,0.));
#13273=DIRECTION('center_axis',(0.,1.,0.));
#13274=DIRECTION('ref_axis',(1.,0.,0.));
#13275=DIRECTION('center_axis',(0.,1.,0.));
#13276=DIRECTION('ref_axis',(1.,0.,0.));
#13277=DIRECTION('center_axis',(0.,1.,0.));
#13278=DIRECTION('ref_axis',(1.,0.,0.));
#13279=DIRECTION('center_axis',(0.,1.,0.));
#13280=DIRECTION('ref_axis',(1.,0.,0.));
#13281=DIRECTION('',(0.,1.,0.));
#13282=DIRECTION('center_axis',(0.,-1.,0.));
#13283=DIRECTION('ref_axis',(1.,0.,0.));
#13284=DIRECTION('center_axis',(0.,1.,0.));
#13285=DIRECTION('ref_axis',(1.,0.,0.));
#13286=DIRECTION('center_axis',(0.,1.,0.));
#13287=DIRECTION('ref_axis',(1.,0.,0.));
#13288=DIRECTION('center_axis',(0.,1.,0.));
#13289=DIRECTION('ref_axis',(1.,0.,0.));
#13290=DIRECTION('center_axis',(0.,1.,0.));
#13291=DIRECTION('ref_axis',(1.,0.,0.));
#13292=DIRECTION('',(0.,1.,0.));
#13293=DIRECTION('center_axis',(0.,-1.,0.));
#13294=DIRECTION('ref_axis',(1.,0.,0.));
#13295=DIRECTION('center_axis',(0.,1.,0.));
#13296=DIRECTION('ref_axis',(1.,0.,0.));
#13297=DIRECTION('center_axis',(0.,1.,0.));
#13298=DIRECTION('ref_axis',(1.,0.,0.));
#13299=DIRECTION('center_axis',(0.,1.,0.));
#13300=DIRECTION('ref_axis',(1.,0.,0.));
#13301=DIRECTION('center_axis',(0.,1.,0.));
#13302=DIRECTION('ref_axis',(1.,0.,0.));
#13303=DIRECTION('',(0.,1.,0.));
#13304=DIRECTION('center_axis',(0.,-1.,0.));
#13305=DIRECTION('ref_axis',(1.,0.,0.));
#13306=DIRECTION('center_axis',(0.,1.,0.));
#13307=DIRECTION('ref_axis',(1.,0.,0.));
#13308=DIRECTION('center_axis',(0.,1.,0.));
#13309=DIRECTION('ref_axis',(1.,0.,0.));
#13310=DIRECTION('center_axis',(0.,1.,0.));
#13311=DIRECTION('ref_axis',(1.,0.,0.));
#13312=DIRECTION('center_axis',(0.,1.,0.));
#13313=DIRECTION('ref_axis',(1.,0.,0.));
#13314=DIRECTION('',(0.,1.,0.));
#13315=DIRECTION('center_axis',(0.,1.,0.));
#13316=DIRECTION('ref_axis',(1.,0.,0.));
#13317=DIRECTION('center_axis',(0.,1.,0.));
#13318=DIRECTION('ref_axis',(1.,0.,0.));
#13319=DIRECTION('',(0.,1.,0.));
#13320=DIRECTION('center_axis',(0.,1.,0.));
#13321=DIRECTION('ref_axis',(1.,0.,0.));
#13322=DIRECTION('center_axis',(0.,1.,0.));
#13323=DIRECTION('ref_axis',(1.,0.,0.));
#13324=DIRECTION('',(0.,1.,0.));
#13325=DIRECTION('center_axis',(0.,1.,0.));
#13326=DIRECTION('ref_axis',(1.,0.,0.));
#13327=DIRECTION('center_axis',(0.,1.,0.));
#13328=DIRECTION('ref_axis',(1.,0.,0.));
#13329=DIRECTION('',(0.,1.,0.));
#13330=DIRECTION('center_axis',(0.,0.,1.));
#13331=DIRECTION('ref_axis',(1.,0.,0.));
#13332=DIRECTION('center_axis',(0.,0.,1.));
#13333=DIRECTION('ref_axis',(1.,0.,0.));
#13334=DIRECTION('',(0.,0.,1.));
#13335=DIRECTION('center_axis',(0.,0.,1.));
#13336=DIRECTION('ref_axis',(1.,0.,0.));
#13337=DIRECTION('center_axis',(0.,0.,1.));
#13338=DIRECTION('ref_axis',(1.,0.,0.));
#13339=DIRECTION('center_axis',(0.,0.,1.));
#13340=DIRECTION('ref_axis',(1.,0.,0.));
#13341=DIRECTION('center_axis',(0.,0.,1.));
#13342=DIRECTION('ref_axis',(1.,0.,0.));
#13343=DIRECTION('',(0.,0.,1.));
#13344=DIRECTION('center_axis',(0.,0.,1.));
#13345=DIRECTION('ref_axis',(1.,0.,0.));
#13346=DIRECTION('center_axis',(0.,0.,1.));
#13347=DIRECTION('ref_axis',(1.,0.,0.));
#13348=DIRECTION('center_axis',(0.,1.,0.));
#13349=DIRECTION('ref_axis',(1.,0.,0.));
#13350=DIRECTION('center_axis',(0.,1.,0.));
#13351=DIRECTION('ref_axis',(1.,0.,0.));
#13352=DIRECTION('',(0.,1.,0.));
#13353=DIRECTION('center_axis',(0.,-1.,0.));
#13354=DIRECTION('ref_axis',(1.,0.,0.));
#13355=DIRECTION('center_axis',(0.,1.,0.));
#13356=DIRECTION('ref_axis',(1.,0.,0.));
#13357=DIRECTION('center_axis',(0.,1.,0.));
#13358=DIRECTION('ref_axis',(1.,0.,0.));
#13359=DIRECTION('center_axis',(0.,1.,0.));
#13360=DIRECTION('ref_axis',(1.,0.,0.));
#13361=DIRECTION('center_axis',(0.,1.,0.));
#13362=DIRECTION('ref_axis',(1.,0.,0.));
#13363=DIRECTION('',(0.,1.,0.));
#13364=DIRECTION('center_axis',(0.,1.,0.));
#13365=DIRECTION('ref_axis',(1.,0.,0.));
#13366=DIRECTION('center_axis',(0.,1.,0.));
#13367=DIRECTION('ref_axis',(1.,0.,0.));
#13368=DIRECTION('',(0.,1.,0.));
#13369=DIRECTION('center_axis',(0.,-1.,0.));
#13370=DIRECTION('ref_axis',(1.,0.,0.));
#13371=DIRECTION('center_axis',(0.,1.,0.));
#13372=DIRECTION('ref_axis',(1.,0.,0.));
#13373=DIRECTION('center_axis',(0.,1.,0.));
#13374=DIRECTION('ref_axis',(1.,0.,0.));
#13375=DIRECTION('center_axis',(0.,1.,0.));
#13376=DIRECTION('ref_axis',(1.,0.,0.));
#13377=DIRECTION('center_axis',(0.,1.,0.));
#13378=DIRECTION('ref_axis',(1.,0.,0.));
#13379=DIRECTION('',(0.,1.,0.));
#13380=DIRECTION('center_axis',(0.,1.,0.));
#13381=DIRECTION('ref_axis',(-1.,0.,0.));
#13382=DIRECTION('',(-1.,0.,0.));
#13383=DIRECTION('',(0.,0.,1.));
#13384=DIRECTION('',(-1.,0.,0.));
#13385=DIRECTION('',(0.,0.,1.));
#13386=DIRECTION('center_axis',(1.,0.,0.));
#13387=DIRECTION('ref_axis',(0.,1.,0.));
#13388=DIRECTION('',(0.,1.,0.));
#13389=DIRECTION('',(0.,1.,0.));
#13390=DIRECTION('',(0.,0.,1.));
#13391=DIRECTION('center_axis',(0.,-1.,0.));
#13392=DIRECTION('ref_axis',(1.,0.,0.));
#13393=DIRECTION('',(1.,0.,0.));
#13394=DIRECTION('',(1.,0.,0.));
#13395=DIRECTION('',(0.,0.,1.));
#13396=DIRECTION('center_axis',(-1.,0.,0.));
#13397=DIRECTION('ref_axis',(0.,-1.,0.));
#13398=DIRECTION('',(0.,-1.,0.));
#13399=DIRECTION('',(0.,-1.,0.));
#13400=DIRECTION('center_axis',(0.,0.,1.));
#13401=DIRECTION('ref_axis',(1.,0.,0.));
#13402=DIRECTION('center_axis',(0.,0.,1.));
#13403=DIRECTION('ref_axis',(1.,0.,0.));
#13404=DIRECTION('axis',(0.,0.,1.));
#13405=DIRECTION('refdir',(1.,0.,0.));
#13406=DIRECTION('center_axis',(0.,1.,0.));
#13407=DIRECTION('ref_axis',(1.,0.,0.));
#13408=DIRECTION('center_axis',(0.,-1.,0.));
#13409=DIRECTION('ref_axis',(1.,0.,0.));
#13410=DIRECTION('',(0.,-1.,0.));
#13411=DIRECTION('center_axis',(0.,-1.,0.));
#13412=DIRECTION('ref_axis',(1.,0.,0.));
#13413=DIRECTION('center_axis',(0.,1.,0.));
#13414=DIRECTION('ref_axis',(1.,0.,0.));
#13415=DIRECTION('center_axis',(0.,1.,0.));
#13416=DIRECTION('ref_axis',(1.,0.,0.));
#13417=DIRECTION('',(0.,-1.,0.));
#13418=DIRECTION('center_axis',(0.,1.,0.));
#13419=DIRECTION('ref_axis',(1.,0.,0.));
#13420=DIRECTION('center_axis',(0.,1.,0.));
#13421=DIRECTION('ref_axis',(1.,0.,0.));
#13422=DIRECTION('center_axis',(0.,1.,0.));
#13423=DIRECTION('ref_axis',(1.,0.,0.));
#13424=DIRECTION('axis',(0.,0.,1.));
#13425=DIRECTION('refdir',(1.,0.,0.));
#13426=DIRECTION('center_axis',(0.,1.,0.));
#13427=DIRECTION('ref_axis',(1.,0.,0.));
#13428=DIRECTION('center_axis',(0.,-1.,0.));
#13429=DIRECTION('ref_axis',(1.,0.,0.));
#13430=DIRECTION('',(0.,-1.,0.));
#13431=DIRECTION('center_axis',(0.,-1.,0.));
#13432=DIRECTION('ref_axis',(1.,0.,0.));
#13433=DIRECTION('center_axis',(0.,1.,0.));
#13434=DIRECTION('ref_axis',(1.,0.,0.));
#13435=DIRECTION('center_axis',(0.,1.,0.));
#13436=DIRECTION('ref_axis',(1.,0.,0.));
#13437=DIRECTION('',(0.,-1.,0.));
#13438=DIRECTION('center_axis',(0.,1.,0.));
#13439=DIRECTION('ref_axis',(1.,0.,0.));
#13440=DIRECTION('center_axis',(0.,1.,0.));
#13441=DIRECTION('ref_axis',(1.,0.,0.));
#13442=DIRECTION('center_axis',(0.,1.,0.));
#13443=DIRECTION('ref_axis',(1.,0.,0.));
#13444=DIRECTION('axis',(0.,0.,1.));
#13445=DIRECTION('refdir',(1.,0.,0.));
#13446=DIRECTION('center_axis',(0.,1.,0.));
#13447=DIRECTION('ref_axis',(1.,0.,0.));
#13448=DIRECTION('center_axis',(0.,-1.,0.));
#13449=DIRECTION('ref_axis',(1.,0.,0.));
#13450=DIRECTION('',(0.,-1.,0.));
#13451=DIRECTION('center_axis',(0.,-1.,0.));
#13452=DIRECTION('ref_axis',(1.,0.,0.));
#13453=DIRECTION('center_axis',(0.,1.,0.));
#13454=DIRECTION('ref_axis',(1.,0.,0.));
#13455=DIRECTION('center_axis',(0.,1.,0.));
#13456=DIRECTION('ref_axis',(1.,0.,0.));
#13457=DIRECTION('',(0.,-1.,0.));
#13458=DIRECTION('center_axis',(0.,1.,0.));
#13459=DIRECTION('ref_axis',(1.,0.,0.));
#13460=DIRECTION('center_axis',(0.,1.,0.));
#13461=DIRECTION('ref_axis',(1.,0.,0.));
#13462=DIRECTION('center_axis',(0.,1.,0.));
#13463=DIRECTION('ref_axis',(1.,0.,0.));
#13464=DIRECTION('axis',(0.,0.,1.));
#13465=DIRECTION('refdir',(1.,0.,0.));
#13466=DIRECTION('center_axis',(0.,1.,0.));
#13467=DIRECTION('ref_axis',(1.,0.,0.));
#13468=DIRECTION('center_axis',(0.,-1.,0.));
#13469=DIRECTION('ref_axis',(1.,0.,0.));
#13470=DIRECTION('',(0.,-1.,0.));
#13471=DIRECTION('center_axis',(0.,-1.,0.));
#13472=DIRECTION('ref_axis',(1.,0.,0.));
#13473=DIRECTION('center_axis',(0.,1.,0.));
#13474=DIRECTION('ref_axis',(1.,0.,0.));
#13475=DIRECTION('center_axis',(0.,1.,0.));
#13476=DIRECTION('ref_axis',(1.,0.,0.));
#13477=DIRECTION('',(0.,-1.,0.));
#13478=DIRECTION('center_axis',(0.,1.,0.));
#13479=DIRECTION('ref_axis',(1.,0.,0.));
#13480=DIRECTION('center_axis',(0.,1.,0.));
#13481=DIRECTION('ref_axis',(1.,0.,0.));
#13482=DIRECTION('center_axis',(0.,1.,0.));
#13483=DIRECTION('ref_axis',(1.,0.,0.));
#13484=DIRECTION('axis',(0.,0.,1.));
#13485=DIRECTION('refdir',(1.,0.,0.));
#13486=DIRECTION('center_axis',(0.,1.,0.));
#13487=DIRECTION('ref_axis',(1.,0.,0.));
#13488=DIRECTION('center_axis',(0.,1.,0.));
#13489=DIRECTION('ref_axis',(1.,0.,0.));
#13490=DIRECTION('',(0.,1.,0.));
#13491=DIRECTION('center_axis',(0.,-1.,0.));
#13492=DIRECTION('ref_axis',(1.,0.,0.));
#13493=DIRECTION('center_axis',(0.,1.,0.));
#13494=DIRECTION('ref_axis',(1.,0.,0.));
#13495=DIRECTION('center_axis',(0.,1.,0.));
#13496=DIRECTION('ref_axis',(1.,0.,0.));
#13497=DIRECTION('',(0.,1.,0.));
#13498=DIRECTION('center_axis',(0.,-1.,0.));
#13499=DIRECTION('ref_axis',(1.,0.,0.));
#13500=DIRECTION('center_axis',(0.,1.,0.));
#13501=DIRECTION('ref_axis',(1.,0.,0.));
#13502=DIRECTION('center_axis',(0.,1.,0.));
#13503=DIRECTION('ref_axis',(1.,0.,0.));
#13504=DIRECTION('',(0.,1.,0.));
#13505=DIRECTION('center_axis',(0.,-1.,0.));
#13506=DIRECTION('ref_axis',(1.,0.,0.));
#13507=DIRECTION('center_axis',(0.,1.,0.));
#13508=DIRECTION('ref_axis',(1.,0.,0.));
#13509=DIRECTION('center_axis',(0.,1.,0.));
#13510=DIRECTION('ref_axis',(1.,0.,0.));
#13511=DIRECTION('',(0.,-1.,0.));
#13512=DIRECTION('center_axis',(0.,-1.,0.));
#13513=DIRECTION('ref_axis',(1.,0.,0.));
#13514=DIRECTION('center_axis',(0.,1.,0.));
#13515=DIRECTION('ref_axis',(1.,0.,0.));
#13516=DIRECTION('center_axis',(0.,-1.,0.));
#13517=DIRECTION('ref_axis',(1.,0.,0.));
#13518=DIRECTION('center_axis',(0.,1.,0.));
#13519=DIRECTION('ref_axis',(1.,0.,0.));
#13520=DIRECTION('',(0.,-1.,0.));
#13521=DIRECTION('center_axis',(0.,-1.,0.));
#13522=DIRECTION('ref_axis',(1.,0.,0.));
#13523=DIRECTION('center_axis',(0.,1.,0.));
#13524=DIRECTION('ref_axis',(1.,0.,0.));
#13525=DIRECTION('center_axis',(0.,1.,0.));
#13526=DIRECTION('ref_axis',(1.,0.,0.));
#13527=DIRECTION('',(0.,-1.,0.));
#13528=DIRECTION('center_axis',(0.,1.,0.));
#13529=DIRECTION('ref_axis',(1.,0.,0.));
#13530=DIRECTION('center_axis',(0.,1.,0.));
#13531=DIRECTION('ref_axis',(1.,0.,0.));
#13532=DIRECTION('center_axis',(0.,1.,0.));
#13533=DIRECTION('ref_axis',(1.,0.,0.));
#13534=DIRECTION('axis',(0.,0.,1.));
#13535=DIRECTION('refdir',(1.,0.,0.));
#13536=DIRECTION('center_axis',(0.,1.,0.));
#13537=DIRECTION('ref_axis',(1.,0.,0.));
#13538=DIRECTION('center_axis',(0.,1.,0.));
#13539=DIRECTION('ref_axis',(1.,0.,0.));
#13540=DIRECTION('',(0.,1.,0.));
#13541=DIRECTION('center_axis',(0.,-1.,0.));
#13542=DIRECTION('ref_axis',(1.,0.,0.));
#13543=DIRECTION('center_axis',(0.,1.,0.));
#13544=DIRECTION('ref_axis',(1.,0.,0.));
#13545=DIRECTION('center_axis',(0.,1.,0.));
#13546=DIRECTION('ref_axis',(1.,0.,0.));
#13547=DIRECTION('',(0.,1.,0.));
#13548=DIRECTION('center_axis',(0.,-1.,0.));
#13549=DIRECTION('ref_axis',(1.,0.,0.));
#13550=DIRECTION('center_axis',(0.,1.,0.));
#13551=DIRECTION('ref_axis',(1.,0.,0.));
#13552=DIRECTION('center_axis',(0.,1.,0.));
#13553=DIRECTION('ref_axis',(1.,0.,0.));
#13554=DIRECTION('',(0.,1.,0.));
#13555=DIRECTION('center_axis',(0.,-1.,0.));
#13556=DIRECTION('ref_axis',(1.,0.,0.));
#13557=DIRECTION('center_axis',(0.,1.,0.));
#13558=DIRECTION('ref_axis',(1.,0.,0.));
#13559=DIRECTION('center_axis',(0.,1.,0.));
#13560=DIRECTION('ref_axis',(1.,0.,0.));
#13561=DIRECTION('',(0.,-1.,0.));
#13562=DIRECTION('center_axis',(0.,-1.,0.));
#13563=DIRECTION('ref_axis',(1.,0.,0.));
#13564=DIRECTION('center_axis',(0.,1.,0.));
#13565=DIRECTION('ref_axis',(1.,0.,0.));
#13566=DIRECTION('center_axis',(0.,-1.,0.));
#13567=DIRECTION('ref_axis',(1.,0.,0.));
#13568=DIRECTION('center_axis',(0.,1.,0.));
#13569=DIRECTION('ref_axis',(1.,0.,0.));
#13570=DIRECTION('',(0.,-1.,0.));
#13571=DIRECTION('center_axis',(0.,-1.,0.));
#13572=DIRECTION('ref_axis',(1.,0.,0.));
#13573=DIRECTION('center_axis',(0.,1.,0.));
#13574=DIRECTION('ref_axis',(1.,0.,0.));
#13575=DIRECTION('center_axis',(0.,1.,0.));
#13576=DIRECTION('ref_axis',(1.,0.,0.));
#13577=DIRECTION('',(0.,-1.,0.));
#13578=DIRECTION('center_axis',(0.,1.,0.));
#13579=DIRECTION('ref_axis',(1.,0.,0.));
#13580=DIRECTION('center_axis',(0.,1.,0.));
#13581=DIRECTION('ref_axis',(1.,0.,0.));
#13582=DIRECTION('center_axis',(0.,1.,0.));
#13583=DIRECTION('ref_axis',(1.,0.,0.));
#13584=DIRECTION('axis',(0.,0.,1.));
#13585=DIRECTION('refdir',(1.,0.,0.));
#13586=DIRECTION('center_axis',(0.,1.,0.));
#13587=DIRECTION('ref_axis',(1.,0.,0.));
#13588=DIRECTION('center_axis',(0.,1.,0.));
#13589=DIRECTION('ref_axis',(1.,0.,0.));
#13590=DIRECTION('',(0.,1.,0.));
#13591=DIRECTION('center_axis',(0.,-1.,0.));
#13592=DIRECTION('ref_axis',(1.,0.,0.));
#13593=DIRECTION('center_axis',(0.,1.,0.));
#13594=DIRECTION('ref_axis',(1.,0.,0.));
#13595=DIRECTION('center_axis',(0.,1.,0.));
#13596=DIRECTION('ref_axis',(1.,0.,0.));
#13597=DIRECTION('',(0.,1.,0.));
#13598=DIRECTION('center_axis',(0.,-1.,0.));
#13599=DIRECTION('ref_axis',(1.,0.,0.));
#13600=DIRECTION('center_axis',(0.,1.,0.));
#13601=DIRECTION('ref_axis',(1.,0.,0.));
#13602=DIRECTION('center_axis',(0.,1.,0.));
#13603=DIRECTION('ref_axis',(1.,0.,0.));
#13604=DIRECTION('',(0.,1.,0.));
#13605=DIRECTION('center_axis',(0.,-1.,0.));
#13606=DIRECTION('ref_axis',(1.,0.,0.));
#13607=DIRECTION('center_axis',(0.,1.,0.));
#13608=DIRECTION('ref_axis',(1.,0.,0.));
#13609=DIRECTION('center_axis',(0.,1.,0.));
#13610=DIRECTION('ref_axis',(1.,0.,0.));
#13611=DIRECTION('',(0.,-1.,0.));
#13612=DIRECTION('center_axis',(0.,1.,0.));
#13613=DIRECTION('ref_axis',(1.,0.,0.));
#13614=DIRECTION('center_axis',(0.,1.,0.));
#13615=DIRECTION('ref_axis',(1.,0.,0.));
#13616=DIRECTION('center_axis',(0.,-1.,0.));
#13617=DIRECTION('ref_axis',(1.,0.,0.));
#13618=DIRECTION('center_axis',(0.,1.,0.));
#13619=DIRECTION('ref_axis',(1.,0.,0.));
#13620=DIRECTION('center_axis',(0.,-1.,0.));
#13621=DIRECTION('ref_axis',(1.,0.,0.));
#13622=DIRECTION('',(0.,-1.,0.));
#13623=DIRECTION('center_axis',(0.,1.,0.));
#13624=DIRECTION('ref_axis',(1.,0.,0.));
#13625=DIRECTION('center_axis',(0.,1.,0.));
#13626=DIRECTION('ref_axis',(1.,0.,0.));
#13627=DIRECTION('',(0.,-1.,0.));
#13628=DIRECTION('center_axis',(0.,1.,0.));
#13629=DIRECTION('ref_axis',(1.,0.,0.));
#13630=DIRECTION('center_axis',(0.,1.,0.));
#13631=DIRECTION('ref_axis',(1.,0.,0.));
#13632=DIRECTION('center_axis',(0.,1.,0.));
#13633=DIRECTION('ref_axis',(1.,0.,0.));
#13634=DIRECTION('axis',(0.,0.,1.));
#13635=DIRECTION('refdir',(1.,0.,0.));
#13636=DIRECTION('center_axis',(0.,1.,0.));
#13637=DIRECTION('ref_axis',(1.,0.,0.));
#13638=DIRECTION('center_axis',(0.,1.,0.));
#13639=DIRECTION('ref_axis',(1.,0.,0.));
#13640=DIRECTION('',(0.,1.,0.));
#13641=DIRECTION('center_axis',(0.,-1.,0.));
#13642=DIRECTION('ref_axis',(1.,0.,0.));
#13643=DIRECTION('center_axis',(0.,1.,0.));
#13644=DIRECTION('ref_axis',(1.,0.,0.));
#13645=DIRECTION('center_axis',(0.,1.,0.));
#13646=DIRECTION('ref_axis',(1.,0.,0.));
#13647=DIRECTION('',(0.,1.,0.));
#13648=DIRECTION('center_axis',(0.,-1.,0.));
#13649=DIRECTION('ref_axis',(1.,0.,0.));
#13650=DIRECTION('center_axis',(0.,1.,0.));
#13651=DIRECTION('ref_axis',(1.,0.,0.));
#13652=DIRECTION('center_axis',(0.,1.,0.));
#13653=DIRECTION('ref_axis',(1.,0.,0.));
#13654=DIRECTION('',(0.,1.,0.));
#13655=DIRECTION('center_axis',(0.,-1.,0.));
#13656=DIRECTION('ref_axis',(1.,0.,0.));
#13657=DIRECTION('center_axis',(0.,1.,0.));
#13658=DIRECTION('ref_axis',(1.,0.,0.));
#13659=DIRECTION('center_axis',(0.,1.,0.));
#13660=DIRECTION('ref_axis',(1.,0.,0.));
#13661=DIRECTION('',(0.,-1.,0.));
#13662=DIRECTION('center_axis',(0.,1.,0.));
#13663=DIRECTION('ref_axis',(1.,0.,0.));
#13664=DIRECTION('center_axis',(0.,1.,0.));
#13665=DIRECTION('ref_axis',(1.,0.,0.));
#13666=DIRECTION('center_axis',(0.,-1.,0.));
#13667=DIRECTION('ref_axis',(1.,0.,0.));
#13668=DIRECTION('center_axis',(0.,1.,0.));
#13669=DIRECTION('ref_axis',(1.,0.,0.));
#13670=DIRECTION('center_axis',(0.,-1.,0.));
#13671=DIRECTION('ref_axis',(1.,0.,0.));
#13672=DIRECTION('',(0.,-1.,0.));
#13673=DIRECTION('center_axis',(0.,1.,0.));
#13674=DIRECTION('ref_axis',(1.,0.,0.));
#13675=DIRECTION('center_axis',(0.,1.,0.));
#13676=DIRECTION('ref_axis',(1.,0.,0.));
#13677=DIRECTION('',(0.,-1.,0.));
#13678=DIRECTION('center_axis',(0.,1.,0.));
#13679=DIRECTION('ref_axis',(1.,0.,0.));
#13680=DIRECTION('center_axis',(0.,1.,0.));
#13681=DIRECTION('ref_axis',(1.,0.,0.));
#13682=DIRECTION('center_axis',(0.,1.,0.));
#13683=DIRECTION('ref_axis',(1.,0.,0.));
#13684=DIRECTION('axis',(0.,0.,1.));
#13685=DIRECTION('refdir',(1.,0.,0.));
#13686=DIRECTION('center_axis',(0.,1.,0.));
#13687=DIRECTION('ref_axis',(0.,0.,1.));
#13688=DIRECTION('center_axis',(0.,-1.,0.));
#13689=DIRECTION('ref_axis',(1.,0.,0.));
#13690=DIRECTION('center_axis',(0.,-1.,0.));
#13691=DIRECTION('ref_axis',(1.,0.,0.));
#13692=DIRECTION('center_axis',(0.,-1.,0.));
#13693=DIRECTION('ref_axis',(1.,0.,0.));
#13694=DIRECTION('',(0.707106781186548,0.707106781186547,8.65956056235493E-17));
#13695=DIRECTION('center_axis',(0.,-1.,0.));
#13696=DIRECTION('ref_axis',(1.,0.,0.));
#13697=DIRECTION('center_axis',(0.,-1.,0.));
#13698=DIRECTION('ref_axis',(1.,0.,0.));
#13699=DIRECTION('',(0.,1.,0.));
#13700=DIRECTION('center_axis',(0.,1.,0.));
#13701=DIRECTION('ref_axis',(1.,0.,0.));
#13702=DIRECTION('center_axis',(0.,-1.,0.));
#13703=DIRECTION('ref_axis',(1.,0.,0.));
#13704=DIRECTION('',(-0.707106781186547,0.707106781186548,-8.65956056235493E-17));
#13705=DIRECTION('center_axis',(0.,-1.,0.));
#13706=DIRECTION('ref_axis',(0.,0.,-1.));
#13707=DIRECTION('center_axis',(0.,-1.,0.));
#13708=DIRECTION('ref_axis',(1.,0.,0.));
#13709=DIRECTION('center_axis',(0.,1.,0.));
#13710=DIRECTION('ref_axis',(1.,0.,0.));
#13711=DIRECTION('center_axis',(0.,1.,0.));
#13712=DIRECTION('ref_axis',(1.,0.,0.));
#13713=DIRECTION('',(-0.447213595499958,0.894427190999916,-5.47678698264203E-17));
#13714=DIRECTION('center_axis',(0.,-1.,0.));
#13715=DIRECTION('ref_axis',(1.,0.,0.));
#13716=DIRECTION('center_axis',(0.,1.,0.));
#13717=DIRECTION('ref_axis',(1.,0.,0.));
#13718=DIRECTION('',(0.,1.,0.));
#13719=DIRECTION('center_axis',(0.,1.,0.));
#13720=DIRECTION('ref_axis',(1.,0.,0.));
#13721=DIRECTION('center_axis',(0.,-1.,0.));
#13722=DIRECTION('ref_axis',(1.,0.,0.));
#13723=DIRECTION('',(-0.707106781186547,0.707106781186548,-8.65956056235493E-17));
#13724=DIRECTION('center_axis',(0.,-1.,0.));
#13725=DIRECTION('ref_axis',(0.,0.,-1.));
#13726=DIRECTION('center_axis',(0.866025403784439,0.,-0.5));
#13727=DIRECTION('ref_axis',(0.5,0.,0.866025403784439));
#13728=DIRECTION('',(-0.5,0.,-0.866025403784439));
#13729=DIRECTION('',(0.,-1.,0.));
#13730=DIRECTION('',(0.5,0.,0.866025403784439));
#13731=DIRECTION('',(0.,-1.,0.));
#13732=DIRECTION('center_axis',(1.20185167898973E-16,0.,-1.));
#13733=DIRECTION('ref_axis',(1.,0.,1.20185167898973E-16));
#13734=DIRECTION('',(-1.,0.,-1.20185167898973E-16));
#13735=DIRECTION('',(0.,-1.,0.));
#13736=DIRECTION('',(1.,0.,1.20185167898973E-16));
#13737=DIRECTION('center_axis',(-0.866025403784439,0.,-0.5));
#13738=DIRECTION('ref_axis',(0.5,0.,-0.866025403784439));
#13739=DIRECTION('',(-0.5,0.,0.866025403784439));
#13740=DIRECTION('',(0.,-1.,0.));
#13741=DIRECTION('',(0.5,0.,-0.866025403784439));
#13742=DIRECTION('center_axis',(-0.866025403784439,0.,0.5));
#13743=DIRECTION('ref_axis',(-0.5,0.,-0.866025403784439));
#13744=DIRECTION('',(0.5,0.,0.866025403784439));
#13745=DIRECTION('',(0.,-1.,0.));
#13746=DIRECTION('',(-0.5,0.,-0.866025403784439));
#13747=DIRECTION('center_axis',(-2.40370335797945E-16,0.,1.));
#13748=DIRECTION('ref_axis',(-1.,0.,-2.40370335797945E-16));
#13749=DIRECTION('',(1.,0.,2.40370335797945E-16));
#13750=DIRECTION('',(0.,-1.,0.));
#13751=DIRECTION('',(-1.,0.,-2.40370335797945E-16));
#13752=DIRECTION('center_axis',(0.866025403784439,0.,0.5));
#13753=DIRECTION('ref_axis',(-0.5,0.,0.866025403784439));
#13754=DIRECTION('',(0.5,0.,-0.866025403784439));
#13755=DIRECTION('',(-0.5,0.,0.866025403784439));
#13756=DIRECTION('center_axis',(0.,1.,0.));
#13757=DIRECTION('ref_axis',(1.,0.,0.));
#13758=DIRECTION('center_axis',(0.,-1.,0.));
#13759=DIRECTION('ref_axis',(0.,0.,-1.));
#13760=DIRECTION('axis',(0.,0.,1.));
#13761=DIRECTION('refdir',(1.,0.,0.));
#13762=DIRECTION('center_axis',(0.,1.,0.));
#13763=DIRECTION('ref_axis',(0.,0.,1.));
#13764=DIRECTION('center_axis',(0.,-1.,0.));
#13765=DIRECTION('ref_axis',(1.,0.,0.));
#13766=DIRECTION('center_axis',(0.,-1.,0.));
#13767=DIRECTION('ref_axis',(1.,0.,0.));
#13768=DIRECTION('center_axis',(0.,-1.,0.));
#13769=DIRECTION('ref_axis',(1.,0.,0.));
#13770=DIRECTION('',(0.707106781186548,0.707106781186547,8.65956056235494E-17));
#13771=DIRECTION('center_axis',(0.,-1.,0.));
#13772=DIRECTION('ref_axis',(1.,0.,0.));
#13773=DIRECTION('center_axis',(0.,-1.,0.));
#13774=DIRECTION('ref_axis',(1.,0.,0.));
#13775=DIRECTION('',(0.,1.,0.));
#13776=DIRECTION('center_axis',(0.,1.,0.));
#13777=DIRECTION('ref_axis',(1.,0.,0.));
#13778=DIRECTION('center_axis',(0.,-1.,0.));
#13779=DIRECTION('ref_axis',(1.,0.,0.));
#13780=DIRECTION('',(-0.707106781186547,0.707106781186548,-8.65956056235493E-17));
#13781=DIRECTION('center_axis',(0.,-1.,0.));
#13782=DIRECTION('ref_axis',(0.,0.,-1.));
#13783=DIRECTION('center_axis',(0.,-1.,0.));
#13784=DIRECTION('ref_axis',(1.,0.,0.));
#13785=DIRECTION('center_axis',(0.,1.,0.));
#13786=DIRECTION('ref_axis',(1.,0.,0.));
#13787=DIRECTION('center_axis',(0.,1.,0.));
#13788=DIRECTION('ref_axis',(1.,0.,0.));
#13789=DIRECTION('',(-0.447213595499958,0.894427190999916,-5.47678698264203E-17));
#13790=DIRECTION('center_axis',(0.,-1.,0.));
#13791=DIRECTION('ref_axis',(1.,0.,0.));
#13792=DIRECTION('center_axis',(0.,1.,0.));
#13793=DIRECTION('ref_axis',(1.,0.,0.));
#13794=DIRECTION('',(0.,1.,0.));
#13795=DIRECTION('center_axis',(0.,1.,0.));
#13796=DIRECTION('ref_axis',(1.,0.,0.));
#13797=DIRECTION('center_axis',(0.,-1.,0.));
#13798=DIRECTION('ref_axis',(1.,0.,0.));
#13799=DIRECTION('',(-0.707106781186547,0.707106781186548,-8.65956056235493E-17));
#13800=DIRECTION('center_axis',(0.,-1.,0.));
#13801=DIRECTION('ref_axis',(0.,0.,-1.));
#13802=DIRECTION('center_axis',(0.866025403784439,0.,-0.5));
#13803=DIRECTION('ref_axis',(0.5,0.,0.866025403784439));
#13804=DIRECTION('',(-0.5,0.,-0.866025403784439));
#13805=DIRECTION('',(0.,-1.,0.));
#13806=DIRECTION('',(0.5,0.,0.866025403784439));
#13807=DIRECTION('',(0.,-1.,0.));
#13808=DIRECTION('center_axis',(1.92296268638356E-16,0.,-1.));
#13809=DIRECTION('ref_axis',(1.,0.,1.92296268638356E-16));
#13810=DIRECTION('',(-1.,0.,-1.92296268638356E-16));
#13811=DIRECTION('',(0.,-1.,0.));
#13812=DIRECTION('',(1.,0.,1.92296268638356E-16));
#13813=DIRECTION('center_axis',(-0.866025403784439,0.,-0.5));
#13814=DIRECTION('ref_axis',(0.5,0.,-0.866025403784439));
#13815=DIRECTION('',(-0.5,0.,0.866025403784438));
#13816=DIRECTION('',(0.,-1.,0.));
#13817=DIRECTION('',(0.5,0.,-0.866025403784438));
#13818=DIRECTION('center_axis',(-0.866025403784439,0.,0.5));
#13819=DIRECTION('ref_axis',(-0.5,0.,-0.866025403784439));
#13820=DIRECTION('',(0.5,0.,0.866025403784439));
#13821=DIRECTION('',(0.,-1.,0.));
#13822=DIRECTION('',(-0.5,0.,-0.866025403784439));
#13823=DIRECTION('center_axis',(-1.92296268638356E-16,0.,1.));
#13824=DIRECTION('ref_axis',(-1.,0.,-1.92296268638356E-16));
#13825=DIRECTION('',(1.,0.,1.92296268638356E-16));
#13826=DIRECTION('',(0.,-1.,0.));
#13827=DIRECTION('',(-1.,0.,-1.92296268638356E-16));
#13828=DIRECTION('center_axis',(0.866025403784439,0.,0.5));
#13829=DIRECTION('ref_axis',(-0.5,0.,0.866025403784439));
#13830=DIRECTION('',(0.5,0.,-0.866025403784439));
#13831=DIRECTION('',(-0.5,0.,0.866025403784439));
#13832=DIRECTION('center_axis',(0.,1.,0.));
#13833=DIRECTION('ref_axis',(1.,0.,0.));
#13834=DIRECTION('center_axis',(0.,-1.,0.));
#13835=DIRECTION('ref_axis',(0.,0.,-1.));
#13836=DIRECTION('axis',(0.,0.,1.));
#13837=DIRECTION('refdir',(1.,0.,0.));
#13838=DIRECTION('axis',(0.,0.,1.));
#13839=DIRECTION('refdir',(1.,0.,0.));
#13840=DIRECTION('center_axis',(0.,-1.,0.));
#13841=DIRECTION('ref_axis',(0.,0.,-1.));
#13842=DIRECTION('center_axis',(0.,-1.,0.));
#13843=DIRECTION('ref_axis',(1.,0.,0.));
#13844=DIRECTION('center_axis',(0.,-1.,0.));
#13845=DIRECTION('ref_axis',(1.,0.,0.));
#13846=DIRECTION('center_axis',(1.,0.,1.22464679914735E-16));
#13847=DIRECTION('ref_axis',(-1.22464679914735E-16,0.,1.));
#13848=DIRECTION('center_axis',(0.,1.,0.));
#13849=DIRECTION('ref_axis',(1.,0.,0.));
#13850=DIRECTION('center_axis',(0.,1.,0.));
#13851=DIRECTION('ref_axis',(1.,0.,0.));
#13852=DIRECTION('center_axis',(0.,-1.,0.));
#13853=DIRECTION('ref_axis',(1.,0.,0.));
#13854=DIRECTION('',(0.,1.,0.));
#13855=DIRECTION('center_axis',(0.,-1.,0.));
#13856=DIRECTION('ref_axis',(1.,0.,0.));
#13857=DIRECTION('center_axis',(0.,-1.,0.));
#13858=DIRECTION('ref_axis',(1.,0.,0.));
#13859=DIRECTION('center_axis',(0.,-1.,0.));
#13860=DIRECTION('ref_axis',(1.,0.,0.));
#13861=DIRECTION('',(0.,1.,0.));
#13862=DIRECTION('center_axis',(0.,-1.,0.));
#13863=DIRECTION('ref_axis',(1.,0.,0.));
#13864=DIRECTION('center_axis',(0.,1.,0.));
#13865=DIRECTION('ref_axis',(1.,0.,0.));
#13866=DIRECTION('',(-0.707106781186548,0.707106781186547,-8.65956056235493E-17));
#13867=DIRECTION('center_axis',(0.,-1.,0.));
#13868=DIRECTION('ref_axis',(1.,0.,0.));
#13869=DIRECTION('center_axis',(0.,1.,0.));
#13870=DIRECTION('ref_axis',(0.,0.,1.));
#13871=DIRECTION('center_axis',(0.,-1.,0.));
#13872=DIRECTION('ref_axis',(1.,0.,0.));
#13873=DIRECTION('center_axis',(0.,-1.,0.));
#13874=DIRECTION('ref_axis',(1.,0.,0.));
#13875=DIRECTION('',(0.,1.,0.));
#13876=DIRECTION('center_axis',(0.,-1.,0.));
#13877=DIRECTION('ref_axis',(0.,0.,-1.));
#13878=DIRECTION('center_axis',(0.,-1.,0.));
#13879=DIRECTION('ref_axis',(1.,0.,0.));
#13880=DIRECTION('center_axis',(0.,-1.,0.));
#13881=DIRECTION('ref_axis',(1.,0.,0.));
#13882=DIRECTION('',(0.707106781186548,0.707106781186547,8.65956056235493E-17));
#13883=DIRECTION('axis',(0.,0.,1.));
#13884=DIRECTION('refdir',(1.,0.,0.));
#13885=DIRECTION('center_axis',(0.,-1.,0.));
#13886=DIRECTION('ref_axis',(0.,0.,-1.));
#13887=DIRECTION('center_axis',(0.,-1.,0.));
#13888=DIRECTION('ref_axis',(1.,0.,0.));
#13889=DIRECTION('center_axis',(0.,-1.,0.));
#13890=DIRECTION('ref_axis',(1.,0.,0.));
#13891=DIRECTION('center_axis',(1.,0.,1.22464679914735E-16));
#13892=DIRECTION('ref_axis',(-1.22464679914735E-16,0.,1.));
#13893=DIRECTION('center_axis',(0.,1.,0.));
#13894=DIRECTION('ref_axis',(1.,0.,0.));
#13895=DIRECTION('center_axis',(0.,1.,0.));
#13896=DIRECTION('ref_axis',(1.,0.,0.));
#13897=DIRECTION('center_axis',(0.,-1.,0.));
#13898=DIRECTION('ref_axis',(1.,0.,0.));
#13899=DIRECTION('center_axis',(0.,-1.,0.));
#13900=DIRECTION('ref_axis',(1.,0.,0.));
#13901=DIRECTION('',(0.,1.,0.));
#13902=DIRECTION('center_axis',(0.,1.,0.));
#13903=DIRECTION('ref_axis',(0.,0.,1.));
#13904=DIRECTION('center_axis',(0.,-1.,0.));
#13905=DIRECTION('ref_axis',(1.,0.,0.));
#13906=DIRECTION('center_axis',(0.,-1.,0.));
#13907=DIRECTION('ref_axis',(1.,0.,0.));
#13908=DIRECTION('center_axis',(0.,-1.,0.));
#13909=DIRECTION('ref_axis',(1.,0.,0.));
#13910=DIRECTION('center_axis',(0.,-1.,0.));
#13911=DIRECTION('ref_axis',(1.,0.,0.));
#13912=DIRECTION('',(0.707106781186548,0.707106781186547,8.65956056235494E-17));
#13913=DIRECTION('center_axis',(0.,-1.,0.));
#13914=DIRECTION('ref_axis',(1.,0.,0.));
#13915=DIRECTION('center_axis',(0.,-1.,0.));
#13916=DIRECTION('ref_axis',(1.,0.,0.));
#13917=DIRECTION('',(0.,1.,0.));
#13918=DIRECTION('center_axis',(0.,1.,0.));
#13919=DIRECTION('ref_axis',(1.,0.,0.));
#13920=DIRECTION('center_axis',(0.,-1.,0.));
#13921=DIRECTION('ref_axis',(1.,0.,0.));
#13922=DIRECTION('',(-0.707106781186548,0.707106781186547,-8.65956056235494E-17));
#13923=DIRECTION('center_axis',(0.,-1.,0.));
#13924=DIRECTION('ref_axis',(0.,0.,-1.));
#13925=DIRECTION('center_axis',(0.,-1.,0.));
#13926=DIRECTION('ref_axis',(1.,0.,0.));
#13927=DIRECTION('',(0.,1.,0.));
#13928=DIRECTION('axis',(0.,0.,1.));
#13929=DIRECTION('refdir',(1.,0.,0.));
#13930=DIRECTION('center_axis',(0.,0.,1.));
#13931=DIRECTION('ref_axis',(1.,0.,0.));
#13932=DIRECTION('center_axis',(1.22464679914735E-16,-1.,0.));
#13933=DIRECTION('ref_axis',(-1.,-1.22464679914735E-16,0.));
#13934=DIRECTION('center_axis',(0.78183148246803,0.,0.623489801858733));
#13935=DIRECTION('ref_axis',(0.623489801858734,0.,-0.78183148246803));
#13936=DIRECTION('center_axis',(7.63554790147315E-17,-1.,-9.57467422477103E-17));
#13937=DIRECTION('ref_axis',(-0.623489801858734,-1.22464679914735E-16,0.78183148246803));
#13938=DIRECTION('center_axis',(0.974927912181824,0.,-0.222520933956314));
#13939=DIRECTION('ref_axis',(-0.222520933956314,0.,-0.974927912181824));
#13940=DIRECTION('center_axis',(-2.7250954951288E-17,-1.,-1.19394234705288E-16));
#13941=DIRECTION('ref_axis',(0.222520933956314,-1.22464679914735E-16,0.974927912181824));
#13942=DIRECTION('center_axis',(0.433883739117558,0.,-0.900968867902419));
#13943=DIRECTION('ref_axis',(-0.900968867902419,0.,-0.433883739117558));
#13944=DIRECTION('center_axis',(-1.10336864020811E-16,-1.,-5.31354332312403E-17));
#13945=DIRECTION('ref_axis',(0.900968867902419,-1.22464679914735E-16,0.433883739117558));
#13946=DIRECTION('center_axis',(-0.433883739117558,0.,-0.900968867902419));
#13947=DIRECTION('ref_axis',(-0.900968867902419,0.,0.433883739117558));
#13948=DIRECTION('center_axis',(-1.10336864020811E-16,-1.,5.31354332312403E-17));
#13949=DIRECTION('ref_axis',(0.900968867902419,-1.22464679914735E-16,-0.433883739117558));
#13950=DIRECTION('center_axis',(-0.974927912181824,0.,-0.222520933956314));
#13951=DIRECTION('ref_axis',(-0.222520933956315,0.,0.974927912181824));
#13952=DIRECTION('center_axis',(-2.7250954951288E-17,-1.,1.19394234705288E-16));
#13953=DIRECTION('ref_axis',(0.222520933956315,-1.22464679914735E-16,-0.974927912181824));
#13954=DIRECTION('center_axis',(-0.78183148246803,0.,0.623489801858734));
#13955=DIRECTION('ref_axis',(0.623489801858733,0.,0.78183148246803));
#13956=DIRECTION('center_axis',(7.63554790147315E-17,-1.,9.57467422477103E-17));
#13957=DIRECTION('ref_axis',(-0.623489801858733,-1.22464679914735E-16,-0.78183148246803));
#13958=DIRECTION('axis',(0.,0.,1.));
#13959=DIRECTION('refdir',(1.,0.,0.));
#13960=DIRECTION('center_axis',(0.,0.,1.));
#13961=DIRECTION('ref_axis',(1.,0.,0.));
#13962=DIRECTION('center_axis',(0.,-1.,0.));
#13963=DIRECTION('ref_axis',(0.,0.,-1.));
#13964=DIRECTION('center_axis',(0.,-1.,0.));
#13965=DIRECTION('ref_axis',(0.,0.,-1.));
#13966=DIRECTION('center_axis',(0.,1.,0.));
#13967=DIRECTION('ref_axis',(1.,0.,0.));
#13968=DIRECTION('center_axis',(0.,1.,0.));
#13969=DIRECTION('ref_axis',(1.,0.,0.));
#13970=DIRECTION('center_axis',(0.,1.,0.));
#13971=DIRECTION('ref_axis',(1.,0.,0.));
#13972=DIRECTION('center_axis',(0.,1.,0.));
#13973=DIRECTION('ref_axis',(1.,0.,0.));
#13974=DIRECTION('',(0.,-1.,0.));
#13975=DIRECTION('center_axis',(0.,-1.,0.));
#13976=DIRECTION('ref_axis',(1.,0.,0.));
#13977=DIRECTION('center_axis',(0.,1.,0.));
#13978=DIRECTION('ref_axis',(1.,0.,0.));
#13979=DIRECTION('center_axis',(0.,1.,0.));
#13980=DIRECTION('ref_axis',(1.,0.,0.));
#13981=DIRECTION('center_axis',(0.,1.,0.));
#13982=DIRECTION('ref_axis',(1.,0.,0.));
#13983=DIRECTION('center_axis',(0.,1.,0.));
#13984=DIRECTION('ref_axis',(1.,0.,0.));
#13985=DIRECTION('center_axis',(0.,1.,0.));
#13986=DIRECTION('ref_axis',(1.,0.,0.));
#13987=DIRECTION('center_axis',(0.,1.,0.));
#13988=DIRECTION('ref_axis',(1.,0.,0.));
#13989=DIRECTION('center_axis',(0.,-1.,0.));
#13990=DIRECTION('ref_axis',(1.,0.,0.));
#13991=DIRECTION('center_axis',(0.,-1.,0.));
#13992=DIRECTION('ref_axis',(0.,0.,-1.));
#13993=DIRECTION('center_axis',(8.96625347776458E-17,0.,1.));
#13994=DIRECTION('ref_axis',(1.,0.,0.));
#13995=DIRECTION('center_axis',(0.,-1.,0.));
#13996=DIRECTION('ref_axis',(0.,0.,-1.));
#13997=DIRECTION('center_axis',(0.,1.,0.));
#13998=DIRECTION('ref_axis',(1.,0.,0.));
#13999=DIRECTION('center_axis',(0.,-1.,0.));
#14000=DIRECTION('ref_axis',(1.,0.,0.));
#14001=DIRECTION('center_axis',(0.,-1.,0.));
#14002=DIRECTION('ref_axis',(0.,0.,-1.));
#14003=DIRECTION('center_axis',(0.,0.,1.));
#14004=DIRECTION('ref_axis',(1.,0.,0.));
#14005=DIRECTION('center_axis',(0.,-1.,0.));
#14006=DIRECTION('ref_axis',(0.,0.,-1.));
#14007=DIRECTION('center_axis',(0.,1.,0.));
#14008=DIRECTION('ref_axis',(1.,0.,0.));
#14009=DIRECTION('center_axis',(0.,-1.,0.));
#14010=DIRECTION('ref_axis',(1.,0.,0.));
#14011=DIRECTION('center_axis',(0.,-1.,0.));
#14012=DIRECTION('ref_axis',(1.,0.,0.));
#14013=DIRECTION('center_axis',(0.,-1.,0.));
#14014=DIRECTION('ref_axis',(0.,0.,-1.));
#14015=DIRECTION('center_axis',(0.,0.,1.));
#14016=DIRECTION('ref_axis',(1.,0.,0.));
#14017=DIRECTION('center_axis',(0.,-1.,0.));
#14018=DIRECTION('ref_axis',(0.,0.,-1.));
#14019=DIRECTION('center_axis',(0.,1.,0.));
#14020=DIRECTION('ref_axis',(1.,0.,0.));
#14021=DIRECTION('center_axis',(0.,-1.,0.));
#14022=DIRECTION('ref_axis',(1.,0.,0.));
#14023=DIRECTION('center_axis',(0.,-1.,0.));
#14024=DIRECTION('ref_axis',(0.,0.,-1.));
#14025=DIRECTION('center_axis',(8.96625347776458E-17,0.,1.));
#14026=DIRECTION('ref_axis',(1.,0.,0.));
#14027=DIRECTION('center_axis',(0.,-1.,0.));
#14028=DIRECTION('ref_axis',(0.,0.,-1.));
#14029=DIRECTION('center_axis',(0.,1.,0.));
#14030=DIRECTION('ref_axis',(1.,0.,0.));
#14031=DIRECTION('center_axis',(0.,-1.,0.));
#14032=DIRECTION('ref_axis',(1.,0.,0.));
#14033=DIRECTION('center_axis',(0.,-1.,0.));
#14034=DIRECTION('ref_axis',(0.,0.,-1.));
#14035=DIRECTION('center_axis',(0.,0.,1.));
#14036=DIRECTION('ref_axis',(1.,0.,0.));
#14037=DIRECTION('center_axis',(0.,-1.,0.));
#14038=DIRECTION('ref_axis',(0.,0.,-1.));
#14039=DIRECTION('center_axis',(0.,1.,0.));
#14040=DIRECTION('ref_axis',(1.,0.,0.));
#14041=DIRECTION('center_axis',(0.,1.,0.));
#14042=DIRECTION('ref_axis',(1.,0.,0.));
#14043=DIRECTION('',(0.,1.,0.));
#14044=DIRECTION('center_axis',(0.,-1.,0.));
#14045=DIRECTION('ref_axis',(1.,0.,0.));
#14046=DIRECTION('center_axis',(0.,-1.,0.));
#14047=DIRECTION('ref_axis',(1.,0.,0.));
#14048=DIRECTION('center_axis',(0.,1.,0.));
#14049=DIRECTION('ref_axis',(1.,0.,0.));
#14050=DIRECTION('center_axis',(0.,-1.,0.));
#14051=DIRECTION('ref_axis',(0.,0.,-1.));
#14052=DIRECTION('center_axis',(0.,0.,1.));
#14053=DIRECTION('ref_axis',(1.,0.,0.));
#14054=DIRECTION('center_axis',(0.,-1.,0.));
#14055=DIRECTION('ref_axis',(0.,0.,-1.));
#14056=DIRECTION('center_axis',(0.,-1.,0.));
#14057=DIRECTION('ref_axis',(-1.,0.,0.));
#14058=DIRECTION('center_axis',(0.,1.,0.));
#14059=DIRECTION('ref_axis',(1.,0.,0.));
#14060=DIRECTION('axis',(0.,0.,1.));
#14061=DIRECTION('refdir',(1.,0.,0.));
#14062=DIRECTION('center_axis',(0.,1.,0.));
#14063=DIRECTION('ref_axis',(0.,0.,1.));
#14064=DIRECTION('center_axis',(0.,-1.,0.));
#14065=DIRECTION('ref_axis',(1.,0.,0.));
#14066=DIRECTION('center_axis',(0.,-1.,0.));
#14067=DIRECTION('ref_axis',(1.,0.,0.));
#14068=DIRECTION('center_axis',(0.,-1.,0.));
#14069=DIRECTION('ref_axis',(1.,0.,0.));
#14070=DIRECTION('center_axis',(0.,-1.,0.));
#14071=DIRECTION('ref_axis',(1.,0.,0.));
#14072=DIRECTION('',(0.,1.,0.));
#14073=DIRECTION('center_axis',(0.,-1.,0.));
#14074=DIRECTION('ref_axis',(0.,0.,-1.));
#14075=DIRECTION('center_axis',(0.,-1.,0.));
#14076=DIRECTION('ref_axis',(1.,0.,0.));
#14077=DIRECTION('center_axis',(0.,-1.,0.));
#14078=DIRECTION('ref_axis',(1.,0.,0.));
#14079=DIRECTION('',(0.,1.,0.));
#14080=DIRECTION('center_axis',(0.,1.,0.));
#14081=DIRECTION('ref_axis',(0.,0.,1.));
#14082=DIRECTION('center_axis',(0.,-1.,0.));
#14083=DIRECTION('ref_axis',(1.,0.,0.));
#14084=DIRECTION('center_axis',(0.,-1.,0.));
#14085=DIRECTION('ref_axis',(1.,0.,0.));
#14086=DIRECTION('center_axis',(0.,-1.,0.));
#14087=DIRECTION('ref_axis',(1.,0.,0.));
#14088=DIRECTION('center_axis',(0.,-1.,0.));
#14089=DIRECTION('ref_axis',(1.,0.,0.));
#14090=DIRECTION('',(0.,1.,0.));
#14091=DIRECTION('center_axis',(0.,-1.,0.));
#14092=DIRECTION('ref_axis',(0.,0.,-1.));
#14093=DIRECTION('center_axis',(0.,-1.,0.));
#14094=DIRECTION('ref_axis',(1.,0.,0.));
#14095=DIRECTION('center_axis',(0.,-1.,0.));
#14096=DIRECTION('ref_axis',(1.,0.,0.));
#14097=DIRECTION('',(0.,1.,0.));
#14098=DIRECTION('',(0.,0.,1.));
#14099=DIRECTION('',(1.,0.,0.));
#14100=DIRECTION('',(0.,0.,1.));
#14101=DIRECTION('',(1.,0.,0.));
#14102=DIRECTION('',(0.,0.,1.));
#14103=DIRECTION('',(1.,0.,0.));
#14104=DIRECTION('',(0.,0.,1.));
#14105=DIRECTION('',(1.,0.,0.));
#14106=DIRECTION('',(0.,0.,1.));
#14107=DIRECTION('',(1.,0.,0.));
#14108=DIRECTION('axis',(0.,0.,1.));
#14109=DIRECTION('refdir',(1.,0.,0.));
#14110=DIRECTION('axis',(0.,0.,1.));
#14111=DIRECTION('refdir',(1.,0.,0.));
#14112=DIRECTION('center_axis',(0.,-1.,0.));
#14113=DIRECTION('ref_axis',(0.,0.,-1.));
#14114=DIRECTION('center_axis',(0.,-1.,0.));
#14115=DIRECTION('ref_axis',(1.,0.,0.));
#14116=DIRECTION('center_axis',(0.,-1.,0.));
#14117=DIRECTION('ref_axis',(1.,0.,0.));
#14118=DIRECTION('center_axis',(1.,0.,1.22464679914735E-16));
#14119=DIRECTION('ref_axis',(-1.22464679914735E-16,0.,1.));
#14120=DIRECTION('center_axis',(0.,1.,0.));
#14121=DIRECTION('ref_axis',(1.,0.,0.));
#14122=DIRECTION('center_axis',(0.,1.,0.));
#14123=DIRECTION('ref_axis',(1.,0.,0.));
#14124=DIRECTION('center_axis',(0.,-1.,0.));
#14125=DIRECTION('ref_axis',(1.,0.,0.));
#14126=DIRECTION('',(0.,1.,0.));
#14127=DIRECTION('center_axis',(0.,-1.,0.));
#14128=DIRECTION('ref_axis',(1.,0.,0.));
#14129=DIRECTION('center_axis',(0.,-1.,0.));
#14130=DIRECTION('ref_axis',(1.,0.,0.));
#14131=DIRECTION('center_axis',(0.,-1.,0.));
#14132=DIRECTION('ref_axis',(1.,0.,0.));
#14133=DIRECTION('',(0.,1.,0.));
#14134=DIRECTION('center_axis',(0.,-1.,0.));
#14135=DIRECTION('ref_axis',(1.,0.,0.));
#14136=DIRECTION('center_axis',(0.,1.,0.));
#14137=DIRECTION('ref_axis',(1.,0.,0.));
#14138=DIRECTION('',(-0.707106781186548,0.707106781186547,-8.65956056235494E-17));
#14139=DIRECTION('center_axis',(0.,-1.,0.));
#14140=DIRECTION('ref_axis',(1.,0.,0.));
#14141=DIRECTION('center_axis',(0.,1.,0.));
#14142=DIRECTION('ref_axis',(0.,0.,1.));
#14143=DIRECTION('center_axis',(0.,-1.,0.));
#14144=DIRECTION('ref_axis',(1.,0.,0.));
#14145=DIRECTION('center_axis',(0.,-1.,0.));
#14146=DIRECTION('ref_axis',(1.,0.,0.));
#14147=DIRECTION('',(0.,1.,0.));
#14148=DIRECTION('center_axis',(0.,-1.,0.));
#14149=DIRECTION('ref_axis',(0.,0.,-1.));
#14150=DIRECTION('center_axis',(0.,-1.,0.));
#14151=DIRECTION('ref_axis',(1.,0.,0.));
#14152=DIRECTION('center_axis',(0.,-1.,0.));
#14153=DIRECTION('ref_axis',(1.,0.,0.));
#14154=DIRECTION('',(0.707106781186548,0.707106781186547,8.65956056235494E-17));
#14155=DIRECTION('axis',(0.,0.,1.));
#14156=DIRECTION('refdir',(1.,0.,0.));
#14157=DIRECTION('center_axis',(0.,-1.,0.));
#14158=DIRECTION('ref_axis',(0.,0.,-1.));
#14159=DIRECTION('center_axis',(0.,-1.,0.));
#14160=DIRECTION('ref_axis',(1.,0.,0.));
#14161=DIRECTION('center_axis',(0.,-1.,0.));
#14162=DIRECTION('ref_axis',(1.,0.,0.));
#14163=DIRECTION('center_axis',(1.,0.,1.22464679914735E-16));
#14164=DIRECTION('ref_axis',(-1.22464679914735E-16,0.,1.));
#14165=DIRECTION('center_axis',(0.,1.,0.));
#14166=DIRECTION('ref_axis',(1.,0.,0.));
#14167=DIRECTION('center_axis',(0.,1.,0.));
#14168=DIRECTION('ref_axis',(1.,0.,0.));
#14169=DIRECTION('center_axis',(0.,-1.,0.));
#14170=DIRECTION('ref_axis',(1.,0.,0.));
#14171=DIRECTION('center_axis',(0.,-1.,0.));
#14172=DIRECTION('ref_axis',(1.,0.,0.));
#14173=DIRECTION('',(0.,1.,0.));
#14174=DIRECTION('center_axis',(0.,1.,0.));
#14175=DIRECTION('ref_axis',(0.,0.,1.));
#14176=DIRECTION('center_axis',(0.,-1.,0.));
#14177=DIRECTION('ref_axis',(1.,0.,0.));
#14178=DIRECTION('center_axis',(0.,-1.,0.));
#14179=DIRECTION('ref_axis',(1.,0.,0.));
#14180=DIRECTION('center_axis',(0.,-1.,0.));
#14181=DIRECTION('ref_axis',(1.,0.,0.));
#14182=DIRECTION('center_axis',(0.,-1.,0.));
#14183=DIRECTION('ref_axis',(1.,0.,0.));
#14184=DIRECTION('',(0.707106781186548,0.707106781186547,8.65956056235494E-17));
#14185=DIRECTION('center_axis',(0.,-1.,0.));
#14186=DIRECTION('ref_axis',(1.,0.,0.));
#14187=DIRECTION('center_axis',(0.,-1.,0.));
#14188=DIRECTION('ref_axis',(1.,0.,0.));
#14189=DIRECTION('',(0.,1.,0.));
#14190=DIRECTION('center_axis',(0.,1.,0.));
#14191=DIRECTION('ref_axis',(1.,0.,0.));
#14192=DIRECTION('center_axis',(0.,-1.,0.));
#14193=DIRECTION('ref_axis',(1.,0.,0.));
#14194=DIRECTION('',(-0.707106781186548,0.707106781186547,-8.65956056235494E-17));
#14195=DIRECTION('center_axis',(0.,-1.,0.));
#14196=DIRECTION('ref_axis',(0.,0.,-1.));
#14197=DIRECTION('center_axis',(0.,-1.,0.));
#14198=DIRECTION('ref_axis',(1.,0.,0.));
#14199=DIRECTION('',(0.,1.,0.));
#14200=DIRECTION('axis',(0.,0.,1.));
#14201=DIRECTION('refdir',(1.,0.,0.));
#14202=DIRECTION('center_axis',(0.,0.,1.));
#14203=DIRECTION('ref_axis',(1.,0.,0.));
#14204=DIRECTION('center_axis',(1.22464679914735E-16,-1.,0.));
#14205=DIRECTION('ref_axis',(-1.,-1.22464679914735E-16,0.));
#14206=DIRECTION('center_axis',(0.707106781186548,0.,0.707106781186548));
#14207=DIRECTION('ref_axis',(0.707106781186548,0.,-0.707106781186548));
#14208=DIRECTION('center_axis',(8.65956056235493E-17,-1.,-8.65956056235493E-17));
#14209=DIRECTION('ref_axis',(-0.707106781186548,-1.22464679914735E-16,0.707106781186548));
#14210=DIRECTION('center_axis',(1.,0.,0.));
#14211=DIRECTION('ref_axis',(6.12323399573677E-17,0.,-1.));
#14212=DIRECTION('center_axis',(7.49879891330929E-33,-1.,-1.22464679914735E-16));
#14213=DIRECTION('ref_axis',(-6.12323399573677E-17,-1.22464679914735E-16,
1.));
#14214=DIRECTION('center_axis',(0.707106781186548,0.,-0.707106781186548));
#14215=DIRECTION('ref_axis',(-0.707106781186548,0.,-0.707106781186548));
#14216=DIRECTION('center_axis',(-8.65956056235493E-17,-1.,-8.65956056235493E-17));
#14217=DIRECTION('ref_axis',(0.707106781186548,-1.22464679914735E-16,0.707106781186548));
#14218=DIRECTION('center_axis',(0.,0.,-1.));
#14219=DIRECTION('ref_axis',(-1.,0.,-1.22464679914735E-16));
#14220=DIRECTION('center_axis',(-1.22464679914735E-16,-1.,-1.49975978266186E-32));
#14221=DIRECTION('ref_axis',(1.,-1.22464679914735E-16,1.22464679914735E-16));
#14222=DIRECTION('center_axis',(-0.707106781186548,0.,-0.707106781186548));
#14223=DIRECTION('ref_axis',(-0.707106781186548,0.,0.707106781186548));
#14224=DIRECTION('center_axis',(-8.65956056235493E-17,-1.,8.65956056235493E-17));
#14225=DIRECTION('ref_axis',(0.707106781186548,-1.22464679914735E-16,-0.707106781186548));
#14226=DIRECTION('center_axis',(-1.,0.,0.));
#14227=DIRECTION('ref_axis',(-1.83697019872103E-16,0.,1.));
#14228=DIRECTION('center_axis',(-2.24963967399279E-32,-1.,1.22464679914735E-16));
#14229=DIRECTION('ref_axis',(1.83697019872103E-16,-1.22464679914735E-16,
-1.));
#14230=DIRECTION('center_axis',(-0.707106781186548,0.,0.707106781186548));
#14231=DIRECTION('ref_axis',(0.707106781186548,0.,0.707106781186548));
#14232=DIRECTION('center_axis',(8.65956056235493E-17,-1.,8.65956056235494E-17));
#14233=DIRECTION('ref_axis',(-0.707106781186548,-1.22464679914735E-16,-0.707106781186548));
#14234=DIRECTION('axis',(0.,0.,1.));
#14235=DIRECTION('refdir',(1.,0.,0.));
#14236=DIRECTION('center_axis',(0.,0.,1.));
#14237=DIRECTION('ref_axis',(1.,0.,0.));
#14238=DIRECTION('center_axis',(0.,-1.,0.));
#14239=DIRECTION('ref_axis',(0.,0.,-1.));
#14240=DIRECTION('center_axis',(0.,-1.,0.));
#14241=DIRECTION('ref_axis',(0.,0.,-1.));
#14242=DIRECTION('center_axis',(0.,1.,0.));
#14243=DIRECTION('ref_axis',(1.,0.,0.));
#14244=DIRECTION('center_axis',(0.,1.,0.));
#14245=DIRECTION('ref_axis',(1.,0.,0.));
#14246=DIRECTION('center_axis',(0.,1.,0.));
#14247=DIRECTION('ref_axis',(1.,0.,0.));
#14248=DIRECTION('center_axis',(0.,1.,0.));
#14249=DIRECTION('ref_axis',(1.,0.,0.));
#14250=DIRECTION('',(0.,-1.,0.));
#14251=DIRECTION('center_axis',(0.,-1.,0.));
#14252=DIRECTION('ref_axis',(1.,0.,0.));
#14253=DIRECTION('center_axis',(0.,1.,0.));
#14254=DIRECTION('ref_axis',(1.,0.,0.));
#14255=DIRECTION('center_axis',(0.,1.,0.));
#14256=DIRECTION('ref_axis',(1.,0.,0.));
#14257=DIRECTION('center_axis',(0.,1.,0.));
#14258=DIRECTION('ref_axis',(1.,0.,0.));
#14259=DIRECTION('center_axis',(0.,1.,0.));
#14260=DIRECTION('ref_axis',(1.,0.,0.));
#14261=DIRECTION('center_axis',(0.,1.,0.));
#14262=DIRECTION('ref_axis',(1.,0.,0.));
#14263=DIRECTION('center_axis',(0.,1.,0.));
#14264=DIRECTION('ref_axis',(1.,0.,0.));
#14265=DIRECTION('center_axis',(0.,-1.,0.));
#14266=DIRECTION('ref_axis',(1.,0.,0.));
#14267=DIRECTION('center_axis',(0.,-1.,0.));
#14268=DIRECTION('ref_axis',(0.,0.,-1.));
#14269=DIRECTION('center_axis',(6.12323399573677E-17,0.,1.));
#14270=DIRECTION('ref_axis',(1.,0.,0.));
#14271=DIRECTION('center_axis',(0.,-1.,0.));
#14272=DIRECTION('ref_axis',(0.,0.,-1.));
#14273=DIRECTION('center_axis',(0.,1.,0.));
#14274=DIRECTION('ref_axis',(1.,0.,0.));
#14275=DIRECTION('center_axis',(0.,-1.,0.));
#14276=DIRECTION('ref_axis',(1.,0.,0.));
#14277=DIRECTION('center_axis',(0.,-1.,0.));
#14278=DIRECTION('ref_axis',(0.,0.,-1.));
#14279=DIRECTION('center_axis',(0.,0.,1.));
#14280=DIRECTION('ref_axis',(1.,0.,0.));
#14281=DIRECTION('center_axis',(0.,-1.,0.));
#14282=DIRECTION('ref_axis',(0.,0.,-1.));
#14283=DIRECTION('center_axis',(0.,1.,0.));
#14284=DIRECTION('ref_axis',(1.,0.,0.));
#14285=DIRECTION('center_axis',(0.,-1.,0.));
#14286=DIRECTION('ref_axis',(1.,0.,0.));
#14287=DIRECTION('center_axis',(0.,-1.,0.));
#14288=DIRECTION('ref_axis',(0.,0.,-1.));
#14289=DIRECTION('center_axis',(0.,0.,1.));
#14290=DIRECTION('ref_axis',(1.,0.,0.));
#14291=DIRECTION('center_axis',(0.,-1.,0.));
#14292=DIRECTION('ref_axis',(0.,0.,-1.));
#14293=DIRECTION('center_axis',(0.,1.,0.));
#14294=DIRECTION('ref_axis',(1.,0.,0.));
#14295=DIRECTION('center_axis',(0.,-1.,0.));
#14296=DIRECTION('ref_axis',(1.,0.,0.));
#14297=DIRECTION('center_axis',(0.,-1.,0.));
#14298=DIRECTION('ref_axis',(0.,0.,-1.));
#14299=DIRECTION('center_axis',(0.,0.,1.));
#14300=DIRECTION('ref_axis',(1.,0.,0.));
#14301=DIRECTION('center_axis',(0.,-1.,0.));
#14302=DIRECTION('ref_axis',(0.,0.,-1.));
#14303=DIRECTION('center_axis',(0.,1.,0.));
#14304=DIRECTION('ref_axis',(1.,0.,0.));
#14305=DIRECTION('center_axis',(0.,-1.,0.));
#14306=DIRECTION('ref_axis',(1.,0.,0.));
#14307=DIRECTION('center_axis',(0.,-1.,0.));
#14308=DIRECTION('ref_axis',(0.,0.,-1.));
#14309=DIRECTION('center_axis',(6.12323399573676E-17,0.,1.));
#14310=DIRECTION('ref_axis',(1.,0.,0.));
#14311=DIRECTION('center_axis',(0.,-1.,0.));
#14312=DIRECTION('ref_axis',(0.,0.,-1.));
#14313=DIRECTION('center_axis',(0.,1.,0.));
#14314=DIRECTION('ref_axis',(1.,0.,0.));
#14315=DIRECTION('center_axis',(0.,-1.,0.));
#14316=DIRECTION('ref_axis',(1.,0.,0.));
#14317=DIRECTION('center_axis',(0.,-1.,0.));
#14318=DIRECTION('ref_axis',(0.,0.,-1.));
#14319=DIRECTION('center_axis',(0.,0.,1.));
#14320=DIRECTION('ref_axis',(1.,0.,0.));
#14321=DIRECTION('center_axis',(0.,-1.,0.));
#14322=DIRECTION('ref_axis',(0.,0.,-1.));
#14323=DIRECTION('center_axis',(0.,1.,0.));
#14324=DIRECTION('ref_axis',(1.,0.,0.));
#14325=DIRECTION('center_axis',(0.,1.,0.));
#14326=DIRECTION('ref_axis',(1.,0.,0.));
#14327=DIRECTION('',(0.,1.,0.));
#14328=DIRECTION('center_axis',(0.,-1.,0.));
#14329=DIRECTION('ref_axis',(1.,0.,0.));
#14330=DIRECTION('center_axis',(0.,-1.,0.));
#14331=DIRECTION('ref_axis',(1.,0.,0.));
#14332=DIRECTION('center_axis',(0.,1.,0.));
#14333=DIRECTION('ref_axis',(1.,0.,0.));
#14334=DIRECTION('center_axis',(0.,-1.,0.));
#14335=DIRECTION('ref_axis',(0.,0.,-1.));
#14336=DIRECTION('center_axis',(0.,0.,1.));
#14337=DIRECTION('ref_axis',(1.,0.,0.));
#14338=DIRECTION('center_axis',(0.,-1.,0.));
#14339=DIRECTION('ref_axis',(0.,0.,-1.));
#14340=DIRECTION('center_axis',(0.,-1.,0.));
#14341=DIRECTION('ref_axis',(-1.,0.,0.));
#14342=DIRECTION('center_axis',(0.,1.,0.));
#14343=DIRECTION('ref_axis',(1.,0.,0.));
#14344=DIRECTION('axis',(0.,0.,1.));
#14345=DIRECTION('refdir',(1.,0.,0.));
#14346=DIRECTION('center_axis',(0.,1.,0.));
#14347=DIRECTION('ref_axis',(0.,0.,1.));
#14348=DIRECTION('center_axis',(0.,-1.,0.));
#14349=DIRECTION('ref_axis',(1.,0.,0.));
#14350=DIRECTION('center_axis',(0.,-1.,0.));
#14351=DIRECTION('ref_axis',(1.,0.,0.));
#14352=DIRECTION('center_axis',(0.,-1.,0.));
#14353=DIRECTION('ref_axis',(1.,0.,0.));
#14354=DIRECTION('center_axis',(0.,-1.,0.));
#14355=DIRECTION('ref_axis',(1.,0.,0.));
#14356=DIRECTION('',(0.,1.,0.));
#14357=DIRECTION('center_axis',(0.,-1.,0.));
#14358=DIRECTION('ref_axis',(0.,0.,-1.));
#14359=DIRECTION('center_axis',(0.,-1.,0.));
#14360=DIRECTION('ref_axis',(1.,0.,0.));
#14361=DIRECTION('center_axis',(0.,-1.,0.));
#14362=DIRECTION('ref_axis',(1.,0.,0.));
#14363=DIRECTION('',(0.,1.,0.));
#14364=DIRECTION('center_axis',(0.,1.,0.));
#14365=DIRECTION('ref_axis',(0.,0.,1.));
#14366=DIRECTION('center_axis',(0.,-1.,0.));
#14367=DIRECTION('ref_axis',(1.,0.,0.));
#14368=DIRECTION('center_axis',(0.,-1.,0.));
#14369=DIRECTION('ref_axis',(1.,0.,0.));
#14370=DIRECTION('center_axis',(0.,-1.,0.));
#14371=DIRECTION('ref_axis',(1.,0.,0.));
#14372=DIRECTION('center_axis',(0.,-1.,0.));
#14373=DIRECTION('ref_axis',(1.,0.,0.));
#14374=DIRECTION('',(0.,1.,0.));
#14375=DIRECTION('center_axis',(0.,-1.,0.));
#14376=DIRECTION('ref_axis',(0.,0.,-1.));
#14377=DIRECTION('center_axis',(0.,-1.,0.));
#14378=DIRECTION('ref_axis',(1.,0.,0.));
#14379=DIRECTION('center_axis',(0.,-1.,0.));
#14380=DIRECTION('ref_axis',(1.,0.,0.));
#14381=DIRECTION('',(0.,1.,0.));
#14382=DIRECTION('',(0.,0.,1.));
#14383=DIRECTION('',(1.,0.,0.));
#14384=DIRECTION('',(0.,0.,1.));
#14385=DIRECTION('',(1.,0.,0.));
#14386=DIRECTION('',(0.,0.,1.));
#14387=DIRECTION('',(1.,0.,0.));
#14388=DIRECTION('',(0.,0.,1.));
#14389=DIRECTION('',(1.,0.,0.));
#14390=DIRECTION('',(0.,0.,1.));
#14391=DIRECTION('',(1.,0.,0.));
#14392=DIRECTION('axis',(0.,0.,1.));
#14393=DIRECTION('refdir',(1.,0.,0.));
#14394=DIRECTION('center_axis',(0.,1.,0.));
#14395=DIRECTION('ref_axis',(0.,0.,1.));
#14396=DIRECTION('center_axis',(0.,-1.,0.));
#14397=DIRECTION('ref_axis',(1.,0.,0.));
#14398=DIRECTION('center_axis',(0.,-1.,0.));
#14399=DIRECTION('ref_axis',(1.,0.,0.));
#14400=DIRECTION('center_axis',(0.,-1.,0.));
#14401=DIRECTION('ref_axis',(1.,0.,0.));
#14402=DIRECTION('',(0.707106781186547,0.707106781186548,8.65956056235493E-17));
#14403=DIRECTION('center_axis',(0.,-1.,0.));
#14404=DIRECTION('ref_axis',(1.,0.,0.));
#14405=DIRECTION('center_axis',(0.,-1.,0.));
#14406=DIRECTION('ref_axis',(1.,0.,0.));
#14407=DIRECTION('',(0.,1.,0.));
#14408=DIRECTION('center_axis',(0.,1.,0.));
#14409=DIRECTION('ref_axis',(1.,0.,0.));
#14410=DIRECTION('center_axis',(0.,-1.,0.));
#14411=DIRECTION('ref_axis',(1.,0.,0.));
#14412=DIRECTION('',(-0.707106781186547,0.707106781186548,-8.65956056235493E-17));
#14413=DIRECTION('center_axis',(0.,-1.,0.));
#14414=DIRECTION('ref_axis',(0.,0.,-1.));
#14415=DIRECTION('center_axis',(0.,-1.,0.));
#14416=DIRECTION('ref_axis',(1.,0.,0.));
#14417=DIRECTION('center_axis',(0.,1.,0.));
#14418=DIRECTION('ref_axis',(1.,0.,0.));
#14419=DIRECTION('center_axis',(0.,1.,0.));
#14420=DIRECTION('ref_axis',(1.,0.,0.));
#14421=DIRECTION('',(-0.447213595499958,0.894427190999916,-5.47678698264203E-17));
#14422=DIRECTION('center_axis',(0.,-1.,0.));
#14423=DIRECTION('ref_axis',(1.,0.,0.));
#14424=DIRECTION('center_axis',(0.,1.,0.));
#14425=DIRECTION('ref_axis',(1.,0.,0.));
#14426=DIRECTION('',(0.,1.,0.));
#14427=DIRECTION('center_axis',(0.,1.,0.));
#14428=DIRECTION('ref_axis',(1.,0.,0.));
#14429=DIRECTION('center_axis',(0.,-1.,0.));
#14430=DIRECTION('ref_axis',(1.,0.,0.));
#14431=DIRECTION('',(-0.707106781186547,0.707106781186548,-8.65956056235493E-17));
#14432=DIRECTION('center_axis',(0.,-1.,0.));
#14433=DIRECTION('ref_axis',(0.,0.,-1.));
#14434=DIRECTION('center_axis',(0.866025403784439,0.,-0.5));
#14435=DIRECTION('ref_axis',(0.5,0.,0.866025403784439));
#14436=DIRECTION('',(-0.5,0.,-0.866025403784439));
#14437=DIRECTION('',(0.,-1.,0.));
#14438=DIRECTION('',(0.5,0.,0.866025403784439));
#14439=DIRECTION('',(0.,-1.,0.));
#14440=DIRECTION('center_axis',(1.60246890531964E-16,0.,-1.));
#14441=DIRECTION('ref_axis',(1.,0.,1.60246890531964E-16));
#14442=DIRECTION('',(-1.,0.,-1.60246890531964E-16));
#14443=DIRECTION('',(0.,-1.,0.));
#14444=DIRECTION('',(1.,0.,1.60246890531964E-16));
#14445=DIRECTION('center_axis',(-0.866025403784439,0.,-0.5));
#14446=DIRECTION('ref_axis',(0.5,0.,-0.866025403784439));
#14447=DIRECTION('',(-0.5,0.,0.866025403784439));
#14448=DIRECTION('',(0.,-1.,0.));
#14449=DIRECTION('',(0.5,0.,-0.866025403784439));
#14450=DIRECTION('center_axis',(-0.866025403784439,0.,0.5));
#14451=DIRECTION('ref_axis',(-0.5,0.,-0.866025403784439));
#14452=DIRECTION('',(0.5,0.,0.866025403784439));
#14453=DIRECTION('',(0.,-1.,0.));
#14454=DIRECTION('',(-0.5,0.,-0.866025403784439));
#14455=DIRECTION('center_axis',(-1.60246890531964E-16,0.,1.));
#14456=DIRECTION('ref_axis',(-1.,0.,-1.60246890531964E-16));
#14457=DIRECTION('',(1.,0.,1.60246890531964E-16));
#14458=DIRECTION('',(0.,-1.,0.));
#14459=DIRECTION('',(-1.,0.,-1.60246890531964E-16));
#14460=DIRECTION('center_axis',(0.866025403784439,0.,0.5));
#14461=DIRECTION('ref_axis',(-0.5,0.,0.866025403784439));
#14462=DIRECTION('',(0.5,0.,-0.866025403784439));
#14463=DIRECTION('',(-0.5,0.,0.866025403784439));
#14464=DIRECTION('center_axis',(0.,1.,0.));
#14465=DIRECTION('ref_axis',(1.,0.,0.));
#14466=DIRECTION('center_axis',(0.,-1.,0.));
#14467=DIRECTION('ref_axis',(0.,0.,-1.));
#14468=DIRECTION('',(0.,0.,1.));
#14469=DIRECTION('',(1.,0.,0.));
#14470=DIRECTION('',(0.,0.,1.));
#14471=DIRECTION('',(1.,0.,0.));
#14472=DIRECTION('',(0.,0.,1.));
#14473=DIRECTION('',(1.,0.,0.));
#14474=DIRECTION('',(0.,0.,1.));
#14475=DIRECTION('',(1.,0.,0.));
#14476=DIRECTION('',(0.,0.,1.));
#14477=DIRECTION('',(1.,0.,0.));
#14478=DIRECTION('',(0.,0.,1.));
#14479=DIRECTION('',(1.,0.,0.));
#14480=DIRECTION('',(0.,0.,1.));
#14481=DIRECTION('',(1.,0.,0.));
#14482=DIRECTION('',(0.,0.,1.));
#14483=DIRECTION('',(1.,0.,0.));
#14484=DIRECTION('',(0.,0.,1.));
#14485=DIRECTION('',(1.,0.,0.));
#14486=DIRECTION('',(0.,0.,1.));
#14487=DIRECTION('',(1.,0.,0.));
#14488=DIRECTION('',(0.,0.,1.));
#14489=DIRECTION('',(1.,0.,0.));
#14490=DIRECTION('',(0.,0.,1.));
#14491=DIRECTION('',(-1.,1.22464679914735E-16,0.));
#14492=DIRECTION('',(0.,0.,1.));
#14493=DIRECTION('',(1.,0.,0.));
#14494=DIRECTION('',(0.,0.,1.));
#14495=DIRECTION('',(-1.,1.22464679914735E-16,0.));
#14496=DIRECTION('',(0.,0.,1.));
#14497=DIRECTION('',(1.,0.,0.));
#14498=DIRECTION('',(0.,0.,1.));
#14499=DIRECTION('',(-1.,1.22464679914735E-16,0.));
#14500=DIRECTION('',(0.,0.,1.));
#14501=DIRECTION('',(1.,0.,0.));
#14502=DIRECTION('',(0.,0.,1.));
#14503=DIRECTION('',(-1.,1.22464679914735E-16,0.));
#14504=DIRECTION('',(0.,0.,1.));
#14505=DIRECTION('',(1.,0.,0.));
#14506=DIRECTION('',(0.,1.,2.22044604925031E-16));
#14507=DIRECTION('',(1.,0.,0.));
#14508=DIRECTION('',(0.,1.,2.22044604925031E-16));
#14509=DIRECTION('',(1.,0.,0.));
#14510=DIRECTION('',(0.,1.,2.22044604925031E-16));
#14511=DIRECTION('',(1.,0.,0.));
#14512=DIRECTION('',(0.,1.,2.22044604925031E-16));
#14513=DIRECTION('',(1.,0.,0.));
#14514=DIRECTION('',(0.,0.,1.));
#14515=DIRECTION('',(1.,0.,0.));
#14516=DIRECTION('',(0.,0.,1.));
#14517=DIRECTION('',(-1.,1.22464679914735E-16,0.));
#14518=DIRECTION('',(0.,0.,1.));
#14519=DIRECTION('',(-1.,1.22464679914735E-16,0.));
#14520=DIRECTION('',(0.,0.,1.));
#14521=DIRECTION('',(-1.,1.22464679914735E-16,0.));
#14522=DIRECTION('',(0.,0.,1.));
#14523=DIRECTION('',(1.,0.,0.));
#14524=DIRECTION('',(0.,0.,1.));
#14525=DIRECTION('',(-1.,1.22464679914735E-16,0.));
#14526=DIRECTION('',(0.,0.,1.));
#14527=DIRECTION('',(-1.,1.22464679914735E-16,0.));
#14528=DIRECTION('',(0.,0.,1.));
#14529=DIRECTION('',(-1.,1.22464679914735E-16,0.));
#14530=DIRECTION('',(0.,0.,1.));
#14531=DIRECTION('',(1.,0.,0.));
#14532=DIRECTION('',(0.,0.,1.));
#14533=DIRECTION('',(1.,0.,0.));
#14534=DIRECTION('',(0.,0.,1.));
#14535=DIRECTION('',(1.,0.,0.));
#14536=DIRECTION('',(0.,0.,1.));
#14537=DIRECTION('',(1.,0.,0.));
#14538=DIRECTION('',(0.,0.,1.));
#14539=DIRECTION('',(1.,0.,0.));
#14540=DIRECTION('',(0.,0.,1.));
#14541=DIRECTION('',(1.,0.,0.));
#14542=DIRECTION('',(0.,0.,1.));
#14543=DIRECTION('',(1.,0.,0.));
#14544=DIRECTION('',(0.,0.,1.));
#14545=DIRECTION('',(1.,0.,0.));
#14546=DIRECTION('axis',(0.,0.,1.));
#14547=DIRECTION('refdir',(1.,0.,0.));
#14548=DIRECTION('axis',(0.,0.,1.));
#14549=DIRECTION('refdir',(1.,0.,0.));
#14550=DIRECTION('center_axis',(-1.,0.,0.));
#14551=DIRECTION('ref_axis',(0.,0.,1.));
#14552=DIRECTION('',(0.,-1.,0.));
#14553=DIRECTION('',(0.,0.,1.));
#14554=DIRECTION('',(0.,1.,0.));
#14555=DIRECTION('',(0.,0.,-1.));
#14556=DIRECTION('center_axis',(0.,1.,0.));
#14557=DIRECTION('ref_axis',(1.,0.,0.));
#14558=DIRECTION('center_axis',(0.,-1.,0.));
#14559=DIRECTION('ref_axis',(1.,0.,0.));
#14560=DIRECTION('',(-1.,0.,0.));
#14561=DIRECTION('',(0.,0.,1.));
#14562=DIRECTION('center_axis',(1.,0.,0.));
#14563=DIRECTION('ref_axis',(0.,0.,-1.));
#14564=DIRECTION('',(0.,1.,0.));
#14565=DIRECTION('',(0.,1.,0.));
#14566=DIRECTION('',(0.,0.,-1.));
#14567=DIRECTION('center_axis',(0.,0.,1.));
#14568=DIRECTION('ref_axis',(1.,0.,0.));
#14569=DIRECTION('',(1.,0.,0.));
#14570=DIRECTION('center_axis',(0.,1.,0.));
#14571=DIRECTION('ref_axis',(0.,0.,1.));
#14572=DIRECTION('center_axis',(0.,1.,0.));
#14573=DIRECTION('ref_axis',(1.,0.,0.));
#14574=DIRECTION('center_axis',(0.,1.,0.));
#14575=DIRECTION('ref_axis',(1.,0.,0.));
#14576=DIRECTION('center_axis',(0.,1.,0.));
#14577=DIRECTION('ref_axis',(1.,0.,0.));
#14578=DIRECTION('',(0.,-1.,0.));
#14579=DIRECTION('center_axis',(0.,1.,0.));
#14580=DIRECTION('ref_axis',(1.,0.,0.));
#14581=DIRECTION('center_axis',(0.,1.,0.));
#14582=DIRECTION('ref_axis',(1.,0.,0.));
#14583=DIRECTION('center_axis',(0.,1.,0.));
#14584=DIRECTION('ref_axis',(1.,0.,0.));
#14585=DIRECTION('axis',(0.,0.,1.));
#14586=DIRECTION('refdir',(1.,0.,0.));
#14587=DIRECTION('center_axis',(0.,1.,0.));
#14588=DIRECTION('ref_axis',(1.,0.,0.));
#14589=DIRECTION('center_axis',(0.,-1.,0.));
#14590=DIRECTION('ref_axis',(1.,0.,0.));
#14591=DIRECTION('',(0.,-1.,0.));
#14592=DIRECTION('center_axis',(0.,-1.,0.));
#14593=DIRECTION('ref_axis',(1.,0.,0.));
#14594=DIRECTION('center_axis',(0.,1.,0.));
#14595=DIRECTION('ref_axis',(1.,0.,0.));
#14596=DIRECTION('center_axis',(0.,1.,0.));
#14597=DIRECTION('ref_axis',(1.,0.,0.));
#14598=DIRECTION('',(0.,-1.,0.));
#14599=DIRECTION('center_axis',(0.,1.,0.));
#14600=DIRECTION('ref_axis',(1.,0.,0.));
#14601=DIRECTION('center_axis',(0.,1.,0.));
#14602=DIRECTION('ref_axis',(1.,0.,0.));
#14603=DIRECTION('center_axis',(0.,1.,0.));
#14604=DIRECTION('ref_axis',(1.,0.,0.));
#14605=DIRECTION('axis',(0.,0.,1.));
#14606=DIRECTION('refdir',(1.,0.,0.));
#14607=DIRECTION('center_axis',(0.,1.,0.));
#14608=DIRECTION('ref_axis',(1.,0.,0.));
#14609=DIRECTION('center_axis',(0.,-1.,0.));
#14610=DIRECTION('ref_axis',(1.,0.,0.));
#14611=DIRECTION('',(0.,-1.,0.));
#14612=DIRECTION('center_axis',(0.,-1.,0.));
#14613=DIRECTION('ref_axis',(1.,0.,0.));
#14614=DIRECTION('center_axis',(0.,1.,0.));
#14615=DIRECTION('ref_axis',(1.,0.,0.));
#14616=DIRECTION('center_axis',(0.,1.,0.));
#14617=DIRECTION('ref_axis',(1.,0.,0.));
#14618=DIRECTION('',(0.,-1.,0.));
#14619=DIRECTION('center_axis',(0.,1.,0.));
#14620=DIRECTION('ref_axis',(1.,0.,0.));
#14621=DIRECTION('center_axis',(0.,1.,0.));
#14622=DIRECTION('ref_axis',(1.,0.,0.));
#14623=DIRECTION('center_axis',(0.,1.,0.));
#14624=DIRECTION('ref_axis',(1.,0.,0.));
#14625=DIRECTION('axis',(0.,0.,1.));
#14626=DIRECTION('refdir',(1.,0.,0.));
#14627=DIRECTION('center_axis',(0.,0.,1.));
#14628=DIRECTION('ref_axis',(1.,0.,0.));
#14629=DIRECTION('',(0.,1.,0.));
#14630=DIRECTION('center_axis',(0.,0.,1.));
#14631=DIRECTION('ref_axis',(1.,0.,0.));
#14632=DIRECTION('center_axis',(0.,0.,1.));
#14633=DIRECTION('ref_axis',(1.,0.,0.));
#14634=DIRECTION('center_axis',(0.,0.,1.));
#14635=DIRECTION('ref_axis',(1.,0.,0.));
#14636=DIRECTION('',(0.,0.,1.));
#14637=DIRECTION('center_axis',(0.,0.,1.));
#14638=DIRECTION('ref_axis',(1.,0.,0.));
#14639=DIRECTION('center_axis',(0.,0.,1.));
#14640=DIRECTION('ref_axis',(1.,0.,0.));
#14641=DIRECTION('',(0.,-1.,0.));
#14642=DIRECTION('center_axis',(0.,1.,0.));
#14643=DIRECTION('ref_axis',(1.,0.,0.));
#14644=DIRECTION('center_axis',(0.,-1.,0.));
#14645=DIRECTION('ref_axis',(1.,0.,0.));
#14646=DIRECTION('',(0.,-1.,0.));
#14647=DIRECTION('center_axis',(0.,-1.,0.));
#14648=DIRECTION('ref_axis',(1.,0.,0.));
#14649=DIRECTION('center_axis',(0.,1.,0.));
#14650=DIRECTION('ref_axis',(1.,0.,0.));
#14651=DIRECTION('center_axis',(0.,1.,0.));
#14652=DIRECTION('ref_axis',(1.,0.,0.));
#14653=DIRECTION('',(0.,-1.,0.));
#14654=DIRECTION('center_axis',(0.,1.,0.));
#14655=DIRECTION('ref_axis',(1.,0.,0.));
#14656=DIRECTION('center_axis',(0.,1.,0.));
#14657=DIRECTION('ref_axis',(1.,0.,0.));
#14658=DIRECTION('center_axis',(0.,1.,0.));
#14659=DIRECTION('ref_axis',(1.,0.,0.));
#14660=DIRECTION('axis',(0.,0.,1.));
#14661=DIRECTION('refdir',(1.,0.,0.));
#14662=DIRECTION('center_axis',(0.,1.,0.));
#14663=DIRECTION('ref_axis',(1.,0.,0.));
#14664=DIRECTION('center_axis',(0.,-1.,0.));
#14665=DIRECTION('ref_axis',(1.,0.,0.));
#14666=DIRECTION('',(0.,-1.,0.));
#14667=DIRECTION('center_axis',(0.,-1.,0.));
#14668=DIRECTION('ref_axis',(1.,0.,0.));
#14669=DIRECTION('center_axis',(0.,1.,0.));
#14670=DIRECTION('ref_axis',(1.,0.,0.));
#14671=DIRECTION('center_axis',(0.,1.,0.));
#14672=DIRECTION('ref_axis',(1.,0.,0.));
#14673=DIRECTION('',(0.,-1.,0.));
#14674=DIRECTION('center_axis',(0.,1.,0.));
#14675=DIRECTION('ref_axis',(1.,0.,0.));
#14676=DIRECTION('center_axis',(0.,1.,0.));
#14677=DIRECTION('ref_axis',(1.,0.,0.));
#14678=DIRECTION('center_axis',(0.,1.,0.));
#14679=DIRECTION('ref_axis',(1.,0.,0.));
#14680=DIRECTION('axis',(0.,0.,1.));
#14681=DIRECTION('refdir',(1.,0.,0.));
#14682=DIRECTION('center_axis',(0.,0.,1.));
#14683=DIRECTION('ref_axis',(1.,0.,0.));
#14684=DIRECTION('',(0.,1.,0.));
#14685=DIRECTION('center_axis',(0.,0.,1.));
#14686=DIRECTION('ref_axis',(1.,0.,0.));
#14687=DIRECTION('center_axis',(0.,0.,1.));
#14688=DIRECTION('ref_axis',(1.,0.,0.));
#14689=DIRECTION('center_axis',(0.,0.,1.));
#14690=DIRECTION('ref_axis',(1.,0.,0.));
#14691=DIRECTION('',(0.,0.,1.));
#14692=DIRECTION('center_axis',(0.,0.,1.));
#14693=DIRECTION('ref_axis',(1.,0.,0.));
#14694=DIRECTION('center_axis',(0.,0.,1.));
#14695=DIRECTION('ref_axis',(1.,0.,0.));
#14696=DIRECTION('',(0.,-1.,0.));
#14697=DIRECTION('center_axis',(0.,1.,0.));
#14698=DIRECTION('ref_axis',(1.,0.,0.));
#14699=DIRECTION('center_axis',(0.,-1.,0.));
#14700=DIRECTION('ref_axis',(1.,0.,0.));
#14701=DIRECTION('',(0.,-1.,0.));
#14702=DIRECTION('center_axis',(0.,-1.,0.));
#14703=DIRECTION('ref_axis',(1.,0.,0.));
#14704=DIRECTION('center_axis',(0.,1.,0.));
#14705=DIRECTION('ref_axis',(1.,0.,0.));
#14706=DIRECTION('center_axis',(0.,1.,0.));
#14707=DIRECTION('ref_axis',(1.,0.,0.));
#14708=DIRECTION('',(0.,-1.,0.));
#14709=DIRECTION('center_axis',(0.,1.,0.));
#14710=DIRECTION('ref_axis',(1.,0.,0.));
#14711=DIRECTION('center_axis',(0.,1.,0.));
#14712=DIRECTION('ref_axis',(1.,0.,0.));
#14713=DIRECTION('center_axis',(0.,1.,0.));
#14714=DIRECTION('ref_axis',(1.,0.,0.));
#14715=DIRECTION('axis',(0.,0.,1.));
#14716=DIRECTION('refdir',(1.,0.,0.));
#14717=DIRECTION('center_axis',(0.,1.,0.));
#14718=DIRECTION('ref_axis',(1.,0.,0.));
#14719=DIRECTION('center_axis',(0.,-1.,0.));
#14720=DIRECTION('ref_axis',(1.,0.,0.));
#14721=DIRECTION('',(0.,-1.,0.));
#14722=DIRECTION('center_axis',(0.,-1.,0.));
#14723=DIRECTION('ref_axis',(1.,0.,0.));
#14724=DIRECTION('center_axis',(0.,1.,0.));
#14725=DIRECTION('ref_axis',(1.,0.,0.));
#14726=DIRECTION('center_axis',(0.,1.,0.));
#14727=DIRECTION('ref_axis',(1.,0.,0.));
#14728=DIRECTION('',(0.,-1.,0.));
#14729=DIRECTION('center_axis',(0.,1.,0.));
#14730=DIRECTION('ref_axis',(1.,0.,0.));
#14731=DIRECTION('center_axis',(0.,1.,0.));
#14732=DIRECTION('ref_axis',(1.,0.,0.));
#14733=DIRECTION('center_axis',(0.,1.,0.));
#14734=DIRECTION('ref_axis',(1.,0.,0.));
#14735=DIRECTION('axis',(0.,0.,1.));
#14736=DIRECTION('refdir',(1.,0.,0.));
#14737=DIRECTION('center_axis',(1.,0.,0.));
#14738=DIRECTION('ref_axis',(0.,0.,-1.));
#14739=DIRECTION('',(0.,0.,1.));
#14740=DIRECTION('',(0.,1.,0.));
#14741=DIRECTION('',(0.,0.,-1.));
#14742=DIRECTION('',(0.,-1.,0.));
#14743=DIRECTION('center_axis',(0.,0.,-1.));
#14744=DIRECTION('ref_axis',(-1.,0.,0.));
#14745=DIRECTION('',(1.,0.,0.));
#14746=DIRECTION('',(0.,-1.,0.));
#14747=DIRECTION('',(-1.,0.,0.));
#14748=DIRECTION('center_axis',(-1.,0.,0.));
#14749=DIRECTION('ref_axis',(0.,0.,1.));
#14750=DIRECTION('',(0.,0.,-1.));
#14751=DIRECTION('',(0.,1.,0.));
#14752=DIRECTION('',(0.,0.,1.));
#14753=DIRECTION('center_axis',(0.,1.,0.));
#14754=DIRECTION('ref_axis',(1.,0.,0.));
#14755=DIRECTION('center_axis',(0.,-1.,0.));
#14756=DIRECTION('ref_axis',(1.,0.,0.));
#14757=DIRECTION('',(-0.587785252292473,0.,0.809016994374947));
#14758=DIRECTION('center_axis',(0.,-1.,0.));
#14759=DIRECTION('ref_axis',(1.,0.,0.));
#14760=DIRECTION('',(-0.809016994374948,0.,0.587785252292473));
#14761=DIRECTION('center_axis',(0.,-1.,0.));
#14762=DIRECTION('ref_axis',(1.,0.,0.));
#14763=DIRECTION('',(-0.951056516295154,0.,0.309016994374947));
#14764=DIRECTION('center_axis',(0.,-1.,0.));
#14765=DIRECTION('ref_axis',(1.,0.,0.));
#14766=DIRECTION('',(-1.,0.,-1.83697019872103E-16));
#14767=DIRECTION('center_axis',(0.,-1.,0.));
#14768=DIRECTION('ref_axis',(1.,0.,0.));
#14769=DIRECTION('',(-0.951056516295154,0.,-0.309016994374948));
#14770=DIRECTION('center_axis',(0.,-1.,0.));
#14771=DIRECTION('ref_axis',(1.,0.,0.));
#14772=DIRECTION('',(-0.809016994374947,0.,-0.587785252292473));
#14773=DIRECTION('center_axis',(0.,-1.,0.));
#14774=DIRECTION('ref_axis',(1.,0.,0.));
#14775=DIRECTION('',(-0.587785252292473,0.,-0.809016994374948));
#14776=DIRECTION('center_axis',(0.,-1.,0.));
#14777=DIRECTION('ref_axis',(1.,0.,0.));
#14778=DIRECTION('',(-0.309016994374947,0.,-0.951056516295154));
#14779=DIRECTION('center_axis',(0.,-1.,0.));
#14780=DIRECTION('ref_axis',(1.,0.,0.));
#14781=DIRECTION('',(1.22464679914735E-16,0.,-1.));
#14782=DIRECTION('center_axis',(0.,-1.,0.));
#14783=DIRECTION('ref_axis',(1.,0.,0.));
#14784=DIRECTION('',(0.309016994374948,0.,-0.951056516295154));
#14785=DIRECTION('center_axis',(0.,-1.,0.));
#14786=DIRECTION('ref_axis',(1.,0.,0.));
#14787=DIRECTION('',(0.587785252292473,0.,-0.809016994374947));
#14788=DIRECTION('center_axis',(0.,-1.,0.));
#14789=DIRECTION('ref_axis',(1.,0.,0.));
#14790=DIRECTION('',(0.809016994374948,0.,-0.587785252292473));
#14791=DIRECTION('center_axis',(0.,-1.,0.));
#14792=DIRECTION('ref_axis',(1.,0.,0.));
#14793=DIRECTION('',(0.951056516295154,0.,-0.309016994374947));
#14794=DIRECTION('center_axis',(0.,-1.,0.));
#14795=DIRECTION('ref_axis',(1.,0.,0.));
#14796=DIRECTION('',(1.,0.,6.12323399573677E-17));
#14797=DIRECTION('center_axis',(0.,-1.,0.));
#14798=DIRECTION('ref_axis',(1.,0.,0.));
#14799=DIRECTION('',(0.951056516295154,0.,0.309016994374948));
#14800=DIRECTION('center_axis',(0.,-1.,0.));
#14801=DIRECTION('ref_axis',(1.,0.,0.));
#14802=DIRECTION('',(0.809016994374947,0.,0.587785252292473));
#14803=DIRECTION('center_axis',(0.,-1.,0.));
#14804=DIRECTION('ref_axis',(1.,0.,0.));
#14805=DIRECTION('',(0.587785252292473,0.,0.809016994374947));
#14806=DIRECTION('center_axis',(0.,-1.,0.));
#14807=DIRECTION('ref_axis',(1.,0.,0.));
#14808=DIRECTION('',(0.309016994374947,0.,0.951056516295154));
#14809=DIRECTION('center_axis',(0.,-1.,0.));
#14810=DIRECTION('ref_axis',(1.,0.,0.));
#14811=DIRECTION('',(0.,0.,1.));
#14812=DIRECTION('center_axis',(0.,-1.,0.));
#14813=DIRECTION('ref_axis',(1.,0.,0.));
#14814=DIRECTION('',(-0.309016994374948,0.,0.951056516295154));
#14815=DIRECTION('center_axis',(0.,1.,0.));
#14816=DIRECTION('ref_axis',(1.,0.,0.));
#14817=DIRECTION('center_axis',(0.,1.,0.));
#14818=DIRECTION('ref_axis',(6.12323399573677E-17,0.,1.));
#14819=DIRECTION('center_axis',(0.,-1.,0.));
#14820=DIRECTION('ref_axis',(1.,0.,0.));
#14821=DIRECTION('center_axis',(0.,1.,0.));
#14822=DIRECTION('ref_axis',(1.,0.,0.));
#14823=DIRECTION('center_axis',(0.,1.,0.));
#14824=DIRECTION('ref_axis',(1.,0.,0.));
#14825=DIRECTION('',(0.,-1.,0.));
#14826=DIRECTION('center_axis',(0.,-1.,0.));
#14827=DIRECTION('ref_axis',(1.,0.,0.));
#14828=DIRECTION('center_axis',(0.,1.,0.));
#14829=DIRECTION('ref_axis',(1.,0.,0.));
#14830=DIRECTION('',(0.,-1.,0.));
#14831=DIRECTION('',(0.,1.,0.));
#14832=DIRECTION('center_axis',(0.951056516295154,0.,0.309016994374948));
#14833=DIRECTION('ref_axis',(0.309016994374948,0.,-0.951056516295154));
#14834=DIRECTION('',(0.309016994374948,0.,-0.951056516295154));
#14835=DIRECTION('',(0.,1.,0.));
#14836=DIRECTION('',(0.,1.,0.));
#14837=DIRECTION('center_axis',(0.,1.,0.));
#14838=DIRECTION('ref_axis',(1.,0.,0.));
#14839=DIRECTION('center_axis',(0.,1.,0.));
#14840=DIRECTION('ref_axis',(1.,0.,0.));
#14841=DIRECTION('',(0.,-1.,0.));
#14842=DIRECTION('',(0.,1.,0.));
#14843=DIRECTION('center_axis',(0.809016994374947,0.,0.587785252292473));
#14844=DIRECTION('ref_axis',(0.587785252292473,0.,-0.809016994374947));
#14845=DIRECTION('',(0.587785252292473,0.,-0.809016994374947));
#14846=DIRECTION('',(0.,1.,0.));
#14847=DIRECTION('',(0.,1.,0.));
#14848=DIRECTION('center_axis',(0.,1.,0.));
#14849=DIRECTION('ref_axis',(1.,0.,0.));
#14850=DIRECTION('center_axis',(0.,1.,0.));
#14851=DIRECTION('ref_axis',(1.,0.,0.));
#14852=DIRECTION('',(0.,-1.,0.));
#14853=DIRECTION('',(0.,1.,0.));
#14854=DIRECTION('center_axis',(0.587785252292473,0.,0.809016994374948));
#14855=DIRECTION('ref_axis',(0.809016994374948,0.,-0.587785252292473));
#14856=DIRECTION('',(0.809016994374948,0.,-0.587785252292473));
#14857=DIRECTION('',(0.,1.,0.));
#14858=DIRECTION('',(0.,1.,0.));
#14859=DIRECTION('center_axis',(0.,1.,0.));
#14860=DIRECTION('ref_axis',(1.,0.,0.));
#14861=DIRECTION('center_axis',(0.,1.,0.));
#14862=DIRECTION('ref_axis',(1.,0.,0.));
#14863=DIRECTION('',(0.,-1.,0.));
#14864=DIRECTION('',(0.,1.,0.));
#14865=DIRECTION('center_axis',(0.309016994374947,0.,0.951056516295154));
#14866=DIRECTION('ref_axis',(0.951056516295154,0.,-0.309016994374947));
#14867=DIRECTION('',(0.951056516295154,0.,-0.309016994374947));
#14868=DIRECTION('',(0.,1.,0.));
#14869=DIRECTION('',(0.,1.,0.));
#14870=DIRECTION('center_axis',(0.,1.,0.));
#14871=DIRECTION('ref_axis',(1.,0.,0.));
#14872=DIRECTION('center_axis',(0.,1.,0.));
#14873=DIRECTION('ref_axis',(1.,0.,0.));
#14874=DIRECTION('',(0.,-1.,0.));
#14875=DIRECTION('',(0.,1.,0.));
#14876=DIRECTION('center_axis',(-1.83697019872103E-16,0.,1.));
#14877=DIRECTION('ref_axis',(1.,0.,1.83697019872103E-16));
#14878=DIRECTION('',(1.,0.,1.83697019872103E-16));
#14879=DIRECTION('',(0.,1.,0.));
#14880=DIRECTION('',(0.,1.,0.));
#14881=DIRECTION('center_axis',(0.,1.,0.));
#14882=DIRECTION('ref_axis',(1.,0.,0.));
#14883=DIRECTION('center_axis',(0.,1.,0.));
#14884=DIRECTION('ref_axis',(1.,0.,0.));
#14885=DIRECTION('',(0.,-1.,0.));
#14886=DIRECTION('',(0.,1.,0.));
#14887=DIRECTION('center_axis',(-0.309016994374948,0.,0.951056516295154));
#14888=DIRECTION('ref_axis',(0.951056516295154,0.,0.309016994374948));
#14889=DIRECTION('',(0.951056516295154,0.,0.309016994374948));
#14890=DIRECTION('',(0.,1.,0.));
#14891=DIRECTION('',(0.,1.,0.));
#14892=DIRECTION('center_axis',(0.,1.,0.));
#14893=DIRECTION('ref_axis',(1.,0.,0.));
#14894=DIRECTION('center_axis',(0.,1.,0.));
#14895=DIRECTION('ref_axis',(1.,0.,0.));
#14896=DIRECTION('',(0.,-1.,0.));
#14897=DIRECTION('',(0.,1.,0.));
#14898=DIRECTION('center_axis',(-0.587785252292473,0.,0.809016994374947));
#14899=DIRECTION('ref_axis',(0.809016994374947,0.,0.587785252292473));
#14900=DIRECTION('',(0.809016994374947,0.,0.587785252292473));
#14901=DIRECTION('',(0.,1.,0.));
#14902=DIRECTION('',(0.,1.,0.));
#14903=DIRECTION('center_axis',(0.,1.,0.));
#14904=DIRECTION('ref_axis',(1.,0.,0.));
#14905=DIRECTION('center_axis',(0.,1.,0.));
#14906=DIRECTION('ref_axis',(1.,0.,0.));
#14907=DIRECTION('',(0.,-1.,0.));
#14908=DIRECTION('',(0.,1.,0.));
#14909=DIRECTION('center_axis',(-0.809016994374948,0.,0.587785252292473));
#14910=DIRECTION('ref_axis',(0.587785252292473,0.,0.809016994374948));
#14911=DIRECTION('',(0.587785252292473,0.,0.809016994374948));
#14912=DIRECTION('',(0.,1.,0.));
#14913=DIRECTION('',(0.,1.,0.));
#14914=DIRECTION('center_axis',(0.,1.,0.));
#14915=DIRECTION('ref_axis',(1.,0.,0.));
#14916=DIRECTION('center_axis',(0.,1.,0.));
#14917=DIRECTION('ref_axis',(1.,0.,0.));
#14918=DIRECTION('',(0.,-1.,0.));
#14919=DIRECTION('',(0.,1.,0.));
#14920=DIRECTION('center_axis',(-0.951056516295154,0.,0.309016994374947));
#14921=DIRECTION('ref_axis',(0.309016994374947,0.,0.951056516295154));
#14922=DIRECTION('',(0.309016994374947,0.,0.951056516295154));
#14923=DIRECTION('',(0.,1.,0.));
#14924=DIRECTION('',(0.,1.,0.));
#14925=DIRECTION('center_axis',(0.,1.,0.));
#14926=DIRECTION('ref_axis',(1.,0.,0.));
#14927=DIRECTION('center_axis',(0.,1.,0.));
#14928=DIRECTION('ref_axis',(1.,0.,0.));
#14929=DIRECTION('',(0.,-1.,0.));
#14930=DIRECTION('',(0.,1.,0.));
#14931=DIRECTION('center_axis',(-1.,0.,-1.22464679914735E-16));
#14932=DIRECTION('ref_axis',(-1.22464679914735E-16,0.,1.));
#14933=DIRECTION('',(-1.22464679914735E-16,0.,1.));
#14934=DIRECTION('',(0.,1.,0.));
#14935=DIRECTION('',(0.,1.,0.));
#14936=DIRECTION('center_axis',(0.,1.,0.));
#14937=DIRECTION('ref_axis',(1.,0.,0.));
#14938=DIRECTION('center_axis',(0.,1.,0.));
#14939=DIRECTION('ref_axis',(1.,0.,0.));
#14940=DIRECTION('',(0.,-1.,0.));
#14941=DIRECTION('',(0.,1.,0.));
#14942=DIRECTION('center_axis',(-0.951056516295154,0.,-0.309016994374948));
#14943=DIRECTION('ref_axis',(-0.309016994374948,0.,0.951056516295154));
#14944=DIRECTION('',(-0.309016994374948,0.,0.951056516295154));
#14945=DIRECTION('',(0.,1.,0.));
#14946=DIRECTION('',(0.,1.,0.));
#14947=DIRECTION('center_axis',(0.,1.,0.));
#14948=DIRECTION('ref_axis',(1.,0.,0.));
#14949=DIRECTION('center_axis',(0.,1.,0.));
#14950=DIRECTION('ref_axis',(1.,0.,0.));
#14951=DIRECTION('',(0.,-1.,0.));
#14952=DIRECTION('',(0.,1.,0.));
#14953=DIRECTION('center_axis',(-0.809016994374947,0.,-0.587785252292473));
#14954=DIRECTION('ref_axis',(-0.587785252292473,0.,0.809016994374947));
#14955=DIRECTION('',(-0.587785252292473,0.,0.809016994374947));
#14956=DIRECTION('',(0.,1.,0.));
#14957=DIRECTION('',(0.,1.,0.));
#14958=DIRECTION('center_axis',(0.,1.,0.));
#14959=DIRECTION('ref_axis',(1.,0.,0.));
#14960=DIRECTION('center_axis',(0.,1.,0.));
#14961=DIRECTION('ref_axis',(1.,0.,0.));
#14962=DIRECTION('',(0.,-1.,0.));
#14963=DIRECTION('',(0.,1.,0.));
#14964=DIRECTION('center_axis',(-0.587785252292473,0.,-0.809016994374948));
#14965=DIRECTION('ref_axis',(-0.809016994374948,0.,0.587785252292473));
#14966=DIRECTION('',(-0.809016994374948,0.,0.587785252292473));
#14967=DIRECTION('',(0.,1.,0.));
#14968=DIRECTION('',(0.,1.,0.));
#14969=DIRECTION('center_axis',(0.,1.,0.));
#14970=DIRECTION('ref_axis',(1.,0.,0.));
#14971=DIRECTION('center_axis',(0.,1.,0.));
#14972=DIRECTION('ref_axis',(1.,0.,0.));
#14973=DIRECTION('',(0.,-1.,0.));
#14974=DIRECTION('',(0.,1.,0.));
#14975=DIRECTION('center_axis',(-0.309016994374947,0.,-0.951056516295154));
#14976=DIRECTION('ref_axis',(-0.951056516295154,0.,0.309016994374947));
#14977=DIRECTION('',(-0.951056516295154,0.,0.309016994374947));
#14978=DIRECTION('',(0.,1.,0.));
#14979=DIRECTION('',(0.,1.,0.));
#14980=DIRECTION('center_axis',(0.,1.,0.));
#14981=DIRECTION('ref_axis',(1.,0.,0.));
#14982=DIRECTION('center_axis',(0.,1.,0.));
#14983=DIRECTION('ref_axis',(1.,0.,0.));
#14984=DIRECTION('',(0.,-1.,0.));
#14985=DIRECTION('',(0.,1.,0.));
#14986=DIRECTION('center_axis',(6.12323399573677E-17,0.,-1.));
#14987=DIRECTION('ref_axis',(-1.,0.,-6.12323399573677E-17));
#14988=DIRECTION('',(-1.,0.,-6.12323399573677E-17));
#14989=DIRECTION('',(0.,1.,0.));
#14990=DIRECTION('',(0.,1.,0.));
#14991=DIRECTION('center_axis',(0.,1.,0.));
#14992=DIRECTION('ref_axis',(1.,0.,0.));
#14993=DIRECTION('center_axis',(0.,1.,0.));
#14994=DIRECTION('ref_axis',(1.,0.,0.));
#14995=DIRECTION('',(0.,-1.,0.));
#14996=DIRECTION('',(0.,1.,0.));
#14997=DIRECTION('center_axis',(0.309016994374948,0.,-0.951056516295154));
#14998=DIRECTION('ref_axis',(-0.951056516295154,0.,-0.309016994374948));
#14999=DIRECTION('',(-0.951056516295154,0.,-0.309016994374948));
#15000=DIRECTION('',(0.,1.,0.));
#15001=DIRECTION('',(0.,1.,0.));
#15002=DIRECTION('center_axis',(0.,1.,0.));
#15003=DIRECTION('ref_axis',(1.,0.,0.));
#15004=DIRECTION('center_axis',(0.,1.,0.));
#15005=DIRECTION('ref_axis',(1.,0.,0.));
#15006=DIRECTION('',(0.,-1.,0.));
#15007=DIRECTION('',(0.,1.,0.));
#15008=DIRECTION('center_axis',(0.587785252292473,0.,-0.809016994374947));
#15009=DIRECTION('ref_axis',(-0.809016994374947,0.,-0.587785252292473));
#15010=DIRECTION('',(-0.809016994374947,0.,-0.587785252292473));
#15011=DIRECTION('',(0.,1.,0.));
#15012=DIRECTION('',(0.,1.,0.));
#15013=DIRECTION('center_axis',(0.,1.,0.));
#15014=DIRECTION('ref_axis',(1.,0.,0.));
#15015=DIRECTION('center_axis',(0.,1.,0.));
#15016=DIRECTION('ref_axis',(1.,0.,0.));
#15017=DIRECTION('',(0.,-1.,0.));
#15018=DIRECTION('',(0.,1.,0.));
#15019=DIRECTION('center_axis',(0.809016994374947,0.,-0.587785252292473));
#15020=DIRECTION('ref_axis',(-0.587785252292473,0.,-0.809016994374947));
#15021=DIRECTION('',(-0.587785252292473,0.,-0.809016994374947));
#15022=DIRECTION('',(0.,1.,0.));
#15023=DIRECTION('',(0.,1.,0.));
#15024=DIRECTION('center_axis',(0.,1.,0.));
#15025=DIRECTION('ref_axis',(1.,0.,0.));
#15026=DIRECTION('center_axis',(0.,1.,0.));
#15027=DIRECTION('ref_axis',(1.,0.,0.));
#15028=DIRECTION('',(0.,-1.,0.));
#15029=DIRECTION('',(0.,1.,0.));
#15030=DIRECTION('center_axis',(0.951056516295154,0.,-0.309016994374947));
#15031=DIRECTION('ref_axis',(-0.309016994374947,0.,-0.951056516295154));
#15032=DIRECTION('',(-0.309016994374947,0.,-0.951056516295154));
#15033=DIRECTION('',(0.,1.,0.));
#15034=DIRECTION('',(0.,1.,0.));
#15035=DIRECTION('center_axis',(0.,1.,0.));
#15036=DIRECTION('ref_axis',(1.,0.,0.));
#15037=DIRECTION('center_axis',(0.,1.,0.));
#15038=DIRECTION('ref_axis',(1.,0.,0.));
#15039=DIRECTION('',(0.,-1.,0.));
#15040=DIRECTION('',(0.,1.,0.));
#15041=DIRECTION('center_axis',(1.,0.,0.));
#15042=DIRECTION('ref_axis',(0.,0.,-1.));
#15043=DIRECTION('',(0.,0.,-1.));
#15044=DIRECTION('',(0.,1.,0.));
#15045=DIRECTION('',(0.,1.,0.));
#15046=DIRECTION('center_axis',(0.,1.,0.));
#15047=DIRECTION('ref_axis',(1.,0.,0.));
#15048=DIRECTION('center_axis',(0.,1.,0.));
#15049=DIRECTION('ref_axis',(1.,0.,0.));
#15050=DIRECTION('center_axis',(0.,1.,0.));
#15051=DIRECTION('ref_axis',(1.,0.,0.));
#15052=DIRECTION('axis',(0.,0.,1.));
#15053=DIRECTION('refdir',(1.,0.,0.));
#15054=DIRECTION('center_axis',(0.,0.707106781186548,0.707106781186547));
#15055=DIRECTION('ref_axis',(1.,0.,0.));
#15056=DIRECTION('',(-3.92523114670944E-15,-0.707106781186547,0.707106781186548));
#15057=DIRECTION('',(1.,0.,0.));
#15058=DIRECTION('',(0.,0.707106781186547,-0.707106781186548));
#15059=DIRECTION('',(-1.,0.,0.));
#15060=DIRECTION('center_axis',(0.,0.,-1.));
#15061=DIRECTION('ref_axis',(0.,1.,0.));
#15062=DIRECTION('',(0.,0.707106781186548,0.707106781186548));
#15063=DIRECTION('center_axis',(0.,0.,-1.));
#15064=DIRECTION('ref_axis',(0.,1.,0.));
#15065=DIRECTION('center_axis',(0.,0.,1.));
#15066=DIRECTION('ref_axis',(0.,1.,0.));
#15067=DIRECTION('center_axis',(0.,-0.707106781186548,0.707106781186547));
#15068=DIRECTION('ref_axis',(1.,0.,0.));
#15069=DIRECTION('',(3.92523114670944E-15,0.707106781186547,0.707106781186548));
#15070=DIRECTION('',(-1.,0.,0.));
#15071=DIRECTION('',(1.,0.,0.));
#15072=DIRECTION('center_axis',(0.,0.,-1.));
#15073=DIRECTION('ref_axis',(0.,-1.,0.));
#15074=DIRECTION('center_axis',(0.,0.,-1.));
#15075=DIRECTION('ref_axis',(0.,-1.,0.));
#15076=DIRECTION('center_axis',(0.,0.,1.));
#15077=DIRECTION('ref_axis',(0.,-1.,0.));
#15078=DIRECTION('center_axis',(0.,0.,1.));
#15079=DIRECTION('ref_axis',(0.,1.,0.));
#15080=DIRECTION('',(0.,0.,1.));
#15081=DIRECTION('center_axis',(0.,0.,-1.));
#15082=DIRECTION('ref_axis',(0.,1.,0.));
#15083=DIRECTION('',(0.,0.,1.));
#15084=DIRECTION('center_axis',(0.,1.,0.));
#15085=DIRECTION('ref_axis',(-1.,0.,0.));
#15086=DIRECTION('',(0.,0.,1.));
#15087=DIRECTION('',(1.,0.,0.));
#15088=DIRECTION('center_axis',(0.,0.,1.));
#15089=DIRECTION('ref_axis',(1.,0.,0.));
#15090=DIRECTION('center_axis',(0.,0.707106781186548,-0.707106781186548));
#15091=DIRECTION('ref_axis',(-1.,0.,0.));
#15092=DIRECTION('',(3.92523114670944E-15,0.707106781186548,0.707106781186548));
#15093=DIRECTION('',(0.,-0.707106781186548,-0.707106781186548));
#15094=DIRECTION('',(-1.,0.,0.));
#15095=DIRECTION('center_axis',(0.,0.,1.));
#15096=DIRECTION('ref_axis',(0.,1.,0.));
#15097=DIRECTION('',(0.,-0.707106781186548,0.707106781186547));
#15098=DIRECTION('center_axis',(0.,0.,1.));
#15099=DIRECTION('ref_axis',(0.,1.,0.));
#15100=DIRECTION('center_axis',(0.,-0.707106781186548,-0.707106781186548));
#15101=DIRECTION('ref_axis',(-1.,0.,0.));
#15102=DIRECTION('',(-3.92523114670944E-15,-0.707106781186548,0.707106781186548));
#15103=DIRECTION('',(-1.,0.,0.));
#15104=DIRECTION('',(1.,0.,0.));
#15105=DIRECTION('center_axis',(0.,0.,1.));
#15106=DIRECTION('ref_axis',(0.,-1.,0.));
#15107=DIRECTION('center_axis',(0.,0.,-1.));
#15108=DIRECTION('ref_axis',(0.,-1.,0.));
#15109=DIRECTION('center_axis',(0.,0.,1.));
#15110=DIRECTION('ref_axis',(0.,-1.,0.));
#15111=DIRECTION('center_axis',(0.,0.,1.));
#15112=DIRECTION('ref_axis',(0.,-1.,0.));
#15113=DIRECTION('',(0.,0.,1.));
#15114=DIRECTION('center_axis',(0.,0.,1.));
#15115=DIRECTION('ref_axis',(1.,0.,0.));
#15116=DIRECTION('center_axis',(0.,-1.,0.));
#15117=DIRECTION('ref_axis',(1.,0.,0.));
#15118=DIRECTION('axis',(0.,0.,1.));
#15119=DIRECTION('refdir',(1.,0.,0.));
#15120=DIRECTION('axis',(0.,0.,1.));
#15121=DIRECTION('refdir',(1.,0.,0.));
#15122=DIRECTION('center_axis',(-1.,0.,0.));
#15123=DIRECTION('ref_axis',(0.,0.,1.));
#15124=DIRECTION('',(0.,-1.,0.));
#15125=DIRECTION('',(0.,0.,1.));
#15126=DIRECTION('',(0.,1.,0.));
#15127=DIRECTION('',(0.,0.,-1.));
#15128=DIRECTION('center_axis',(0.,1.,0.));
#15129=DIRECTION('ref_axis',(1.,0.,0.));
#15130=DIRECTION('center_axis',(0.,-1.,0.));
#15131=DIRECTION('ref_axis',(1.,0.,0.));
#15132=DIRECTION('',(-1.,0.,0.));
#15133=DIRECTION('',(0.,0.,1.));
#15134=DIRECTION('center_axis',(1.,0.,0.));
#15135=DIRECTION('ref_axis',(0.,0.,-1.));
#15136=DIRECTION('',(0.,1.,0.));
#15137=DIRECTION('',(0.,1.,0.));
#15138=DIRECTION('',(0.,0.,-1.));
#15139=DIRECTION('center_axis',(0.,0.,1.));
#15140=DIRECTION('ref_axis',(1.,0.,0.));
#15141=DIRECTION('',(1.,0.,0.));
#15142=DIRECTION('center_axis',(0.,1.,0.));
#15143=DIRECTION('ref_axis',(0.,0.,1.));
#15144=DIRECTION('center_axis',(0.,1.,0.));
#15145=DIRECTION('ref_axis',(1.,0.,0.));
#15146=DIRECTION('center_axis',(0.,1.,0.));
#15147=DIRECTION('ref_axis',(1.,0.,0.));
#15148=DIRECTION('center_axis',(0.,1.,0.));
#15149=DIRECTION('ref_axis',(1.,0.,0.));
#15150=DIRECTION('',(0.,-1.,0.));
#15151=DIRECTION('center_axis',(0.,1.,0.));
#15152=DIRECTION('ref_axis',(1.,0.,0.));
#15153=DIRECTION('center_axis',(0.,1.,0.));
#15154=DIRECTION('ref_axis',(1.,0.,0.));
#15155=DIRECTION('center_axis',(0.,1.,0.));
#15156=DIRECTION('ref_axis',(1.,0.,0.));
#15157=DIRECTION('axis',(0.,0.,1.));
#15158=DIRECTION('refdir',(1.,0.,0.));
#15159=DIRECTION('center_axis',(0.,1.,0.));
#15160=DIRECTION('ref_axis',(1.,0.,0.));
#15161=DIRECTION('center_axis',(0.,-1.,0.));
#15162=DIRECTION('ref_axis',(1.,0.,0.));
#15163=DIRECTION('',(0.,-1.,0.));
#15164=DIRECTION('center_axis',(0.,-1.,0.));
#15165=DIRECTION('ref_axis',(1.,0.,0.));
#15166=DIRECTION('center_axis',(0.,1.,0.));
#15167=DIRECTION('ref_axis',(1.,0.,0.));
#15168=DIRECTION('center_axis',(0.,1.,0.));
#15169=DIRECTION('ref_axis',(1.,0.,0.));
#15170=DIRECTION('',(0.,-1.,0.));
#15171=DIRECTION('center_axis',(0.,1.,0.));
#15172=DIRECTION('ref_axis',(1.,0.,0.));
#15173=DIRECTION('center_axis',(0.,1.,0.));
#15174=DIRECTION('ref_axis',(1.,0.,0.));
#15175=DIRECTION('center_axis',(0.,1.,0.));
#15176=DIRECTION('ref_axis',(1.,0.,0.));
#15177=DIRECTION('axis',(0.,0.,1.));
#15178=DIRECTION('refdir',(1.,0.,0.));
#15179=DIRECTION('center_axis',(0.,1.,0.));
#15180=DIRECTION('ref_axis',(1.,0.,0.));
#15181=DIRECTION('center_axis',(0.,-1.,0.));
#15182=DIRECTION('ref_axis',(1.,0.,0.));
#15183=DIRECTION('',(0.,-1.,0.));
#15184=DIRECTION('center_axis',(0.,-1.,0.));
#15185=DIRECTION('ref_axis',(1.,0.,0.));
#15186=DIRECTION('center_axis',(0.,1.,0.));
#15187=DIRECTION('ref_axis',(1.,0.,0.));
#15188=DIRECTION('center_axis',(0.,1.,0.));
#15189=DIRECTION('ref_axis',(1.,0.,0.));
#15190=DIRECTION('',(0.,-1.,0.));
#15191=DIRECTION('center_axis',(0.,1.,0.));
#15192=DIRECTION('ref_axis',(1.,0.,0.));
#15193=DIRECTION('center_axis',(0.,1.,0.));
#15194=DIRECTION('ref_axis',(1.,0.,0.));
#15195=DIRECTION('center_axis',(0.,1.,0.));
#15196=DIRECTION('ref_axis',(1.,0.,0.));
#15197=DIRECTION('axis',(0.,0.,1.));
#15198=DIRECTION('refdir',(1.,0.,0.));
#15199=DIRECTION('center_axis',(0.,0.,1.));
#15200=DIRECTION('ref_axis',(1.,0.,0.));
#15201=DIRECTION('',(0.,1.,0.));
#15202=DIRECTION('center_axis',(0.,0.,1.));
#15203=DIRECTION('ref_axis',(1.,0.,0.));
#15204=DIRECTION('center_axis',(0.,0.,1.));
#15205=DIRECTION('ref_axis',(1.,0.,0.));
#15206=DIRECTION('center_axis',(0.,0.,1.));
#15207=DIRECTION('ref_axis',(1.,0.,0.));
#15208=DIRECTION('',(0.,0.,1.));
#15209=DIRECTION('center_axis',(0.,0.,1.));
#15210=DIRECTION('ref_axis',(1.,0.,0.));
#15211=DIRECTION('center_axis',(0.,0.,1.));
#15212=DIRECTION('ref_axis',(1.,0.,0.));
#15213=DIRECTION('',(0.,-1.,0.));
#15214=DIRECTION('center_axis',(0.,1.,0.));
#15215=DIRECTION('ref_axis',(1.,0.,0.));
#15216=DIRECTION('center_axis',(0.,-1.,0.));
#15217=DIRECTION('ref_axis',(1.,0.,0.));
#15218=DIRECTION('',(0.,-1.,0.));
#15219=DIRECTION('center_axis',(0.,-1.,0.));
#15220=DIRECTION('ref_axis',(1.,0.,0.));
#15221=DIRECTION('center_axis',(0.,1.,0.));
#15222=DIRECTION('ref_axis',(1.,0.,0.));
#15223=DIRECTION('center_axis',(0.,1.,0.));
#15224=DIRECTION('ref_axis',(1.,0.,0.));
#15225=DIRECTION('',(0.,-1.,0.));
#15226=DIRECTION('center_axis',(0.,1.,0.));
#15227=DIRECTION('ref_axis',(1.,0.,0.));
#15228=DIRECTION('center_axis',(0.,1.,0.));
#15229=DIRECTION('ref_axis',(1.,0.,0.));
#15230=DIRECTION('center_axis',(0.,1.,0.));
#15231=DIRECTION('ref_axis',(1.,0.,0.));
#15232=DIRECTION('axis',(0.,0.,1.));
#15233=DIRECTION('refdir',(1.,0.,0.));
#15234=DIRECTION('center_axis',(0.,1.,0.));
#15235=DIRECTION('ref_axis',(1.,0.,0.));
#15236=DIRECTION('center_axis',(0.,-1.,0.));
#15237=DIRECTION('ref_axis',(1.,0.,0.));
#15238=DIRECTION('',(0.,-1.,0.));
#15239=DIRECTION('center_axis',(0.,-1.,0.));
#15240=DIRECTION('ref_axis',(1.,0.,0.));
#15241=DIRECTION('center_axis',(0.,1.,0.));
#15242=DIRECTION('ref_axis',(1.,0.,0.));
#15243=DIRECTION('center_axis',(0.,1.,0.));
#15244=DIRECTION('ref_axis',(1.,0.,0.));
#15245=DIRECTION('',(0.,-1.,0.));
#15246=DIRECTION('center_axis',(0.,1.,0.));
#15247=DIRECTION('ref_axis',(1.,0.,0.));
#15248=DIRECTION('center_axis',(0.,1.,0.));
#15249=DIRECTION('ref_axis',(1.,0.,0.));
#15250=DIRECTION('center_axis',(0.,1.,0.));
#15251=DIRECTION('ref_axis',(1.,0.,0.));
#15252=DIRECTION('axis',(0.,0.,1.));
#15253=DIRECTION('refdir',(1.,0.,0.));
#15254=DIRECTION('center_axis',(0.,0.,1.));
#15255=DIRECTION('ref_axis',(1.,0.,0.));
#15256=DIRECTION('',(0.,1.,0.));
#15257=DIRECTION('center_axis',(0.,0.,1.));
#15258=DIRECTION('ref_axis',(1.,0.,0.));
#15259=DIRECTION('center_axis',(0.,0.,1.));
#15260=DIRECTION('ref_axis',(1.,0.,0.));
#15261=DIRECTION('center_axis',(0.,0.,1.));
#15262=DIRECTION('ref_axis',(1.,0.,0.));
#15263=DIRECTION('',(0.,0.,1.));
#15264=DIRECTION('center_axis',(0.,0.,1.));
#15265=DIRECTION('ref_axis',(1.,0.,0.));
#15266=DIRECTION('center_axis',(0.,0.,1.));
#15267=DIRECTION('ref_axis',(1.,0.,0.));
#15268=DIRECTION('',(0.,-1.,0.));
#15269=DIRECTION('center_axis',(0.,1.,0.));
#15270=DIRECTION('ref_axis',(1.,0.,0.));
#15271=DIRECTION('center_axis',(0.,-1.,0.));
#15272=DIRECTION('ref_axis',(1.,0.,0.));
#15273=DIRECTION('',(0.,-1.,0.));
#15274=DIRECTION('center_axis',(0.,-1.,0.));
#15275=DIRECTION('ref_axis',(1.,0.,0.));
#15276=DIRECTION('center_axis',(0.,1.,0.));
#15277=DIRECTION('ref_axis',(1.,0.,0.));
#15278=DIRECTION('center_axis',(0.,1.,0.));
#15279=DIRECTION('ref_axis',(1.,0.,0.));
#15280=DIRECTION('',(0.,-1.,0.));
#15281=DIRECTION('center_axis',(0.,1.,0.));
#15282=DIRECTION('ref_axis',(1.,0.,0.));
#15283=DIRECTION('center_axis',(0.,1.,0.));
#15284=DIRECTION('ref_axis',(1.,0.,0.));
#15285=DIRECTION('center_axis',(0.,1.,0.));
#15286=DIRECTION('ref_axis',(1.,0.,0.));
#15287=DIRECTION('axis',(0.,0.,1.));
#15288=DIRECTION('refdir',(1.,0.,0.));
#15289=DIRECTION('center_axis',(0.,1.,0.));
#15290=DIRECTION('ref_axis',(1.,0.,0.));
#15291=DIRECTION('center_axis',(0.,-1.,0.));
#15292=DIRECTION('ref_axis',(1.,0.,0.));
#15293=DIRECTION('',(0.,-1.,0.));
#15294=DIRECTION('center_axis',(0.,-1.,0.));
#15295=DIRECTION('ref_axis',(1.,0.,0.));
#15296=DIRECTION('center_axis',(0.,1.,0.));
#15297=DIRECTION('ref_axis',(1.,0.,0.));
#15298=DIRECTION('center_axis',(0.,1.,0.));
#15299=DIRECTION('ref_axis',(1.,0.,0.));
#15300=DIRECTION('',(0.,-1.,0.));
#15301=DIRECTION('center_axis',(0.,1.,0.));
#15302=DIRECTION('ref_axis',(1.,0.,0.));
#15303=DIRECTION('center_axis',(0.,1.,0.));
#15304=DIRECTION('ref_axis',(1.,0.,0.));
#15305=DIRECTION('center_axis',(0.,1.,0.));
#15306=DIRECTION('ref_axis',(1.,0.,0.));
#15307=DIRECTION('axis',(0.,0.,1.));
#15308=DIRECTION('refdir',(1.,0.,0.));
#15309=DIRECTION('center_axis',(1.,0.,0.));
#15310=DIRECTION('ref_axis',(0.,0.,-1.));
#15311=DIRECTION('',(0.,0.,1.));
#15312=DIRECTION('',(0.,1.,0.));
#15313=DIRECTION('',(0.,0.,-1.));
#15314=DIRECTION('',(0.,-1.,0.));
#15315=DIRECTION('center_axis',(0.,0.,-1.));
#15316=DIRECTION('ref_axis',(-1.,0.,0.));
#15317=DIRECTION('',(1.,0.,0.));
#15318=DIRECTION('',(0.,-1.,0.));
#15319=DIRECTION('',(-1.,0.,0.));
#15320=DIRECTION('center_axis',(-1.,0.,0.));
#15321=DIRECTION('ref_axis',(0.,0.,1.));
#15322=DIRECTION('',(0.,0.,-1.));
#15323=DIRECTION('',(0.,1.,0.));
#15324=DIRECTION('',(0.,0.,1.));
#15325=DIRECTION('center_axis',(0.,1.,0.));
#15326=DIRECTION('ref_axis',(1.,0.,0.));
#15327=DIRECTION('center_axis',(0.,-1.,0.));
#15328=DIRECTION('ref_axis',(1.,0.,0.));
#15329=DIRECTION('',(-0.309016994374948,0.,0.951056516295154));
#15330=DIRECTION('center_axis',(0.,-1.,0.));
#15331=DIRECTION('ref_axis',(1.,0.,0.));
#15332=DIRECTION('',(-0.453990499739547,0.,0.891006524188368));
#15333=DIRECTION('center_axis',(0.,-1.,0.));
#15334=DIRECTION('ref_axis',(1.,0.,0.));
#15335=DIRECTION('',(-0.587785252292473,0.,0.809016994374947));
#15336=DIRECTION('center_axis',(0.,-1.,0.));
#15337=DIRECTION('ref_axis',(1.,0.,0.));
#15338=DIRECTION('',(-0.707106781186548,0.,0.707106781186547));
#15339=DIRECTION('center_axis',(0.,-1.,0.));
#15340=DIRECTION('ref_axis',(1.,0.,0.));
#15341=DIRECTION('',(-0.809016994374948,0.,0.587785252292473));
#15342=DIRECTION('center_axis',(0.,-1.,0.));
#15343=DIRECTION('ref_axis',(1.,0.,0.));
#15344=DIRECTION('',(-0.891006524188368,0.,0.453990499739547));
#15345=DIRECTION('center_axis',(0.,-1.,0.));
#15346=DIRECTION('ref_axis',(1.,0.,0.));
#15347=DIRECTION('',(-0.951056516295154,0.,0.309016994374947));
#15348=DIRECTION('center_axis',(0.,-1.,0.));
#15349=DIRECTION('ref_axis',(1.,0.,0.));
#15350=DIRECTION('',(-0.987688340595138,0.,0.156434465040231));
#15351=DIRECTION('center_axis',(0.,-1.,0.));
#15352=DIRECTION('ref_axis',(1.,0.,0.));
#15353=DIRECTION('',(-1.,0.,-1.83697019872103E-16));
#15354=DIRECTION('center_axis',(0.,-1.,0.));
#15355=DIRECTION('ref_axis',(1.,0.,0.));
#15356=DIRECTION('',(-0.987688340595138,0.,-0.156434465040231));
#15357=DIRECTION('center_axis',(0.,-1.,0.));
#15358=DIRECTION('ref_axis',(1.,0.,0.));
#15359=DIRECTION('',(-0.951056516295154,0.,-0.309016994374948));
#15360=DIRECTION('center_axis',(0.,-1.,0.));
#15361=DIRECTION('ref_axis',(1.,0.,0.));
#15362=DIRECTION('',(-0.891006524188368,0.,-0.453990499739547));
#15363=DIRECTION('center_axis',(0.,-1.,0.));
#15364=DIRECTION('ref_axis',(1.,0.,0.));
#15365=DIRECTION('',(-0.809016994374947,0.,-0.587785252292473));
#15366=DIRECTION('center_axis',(0.,-1.,0.));
#15367=DIRECTION('ref_axis',(1.,0.,0.));
#15368=DIRECTION('',(-0.707106781186547,0.,-0.707106781186548));
#15369=DIRECTION('center_axis',(0.,-1.,0.));
#15370=DIRECTION('ref_axis',(1.,0.,0.));
#15371=DIRECTION('',(-0.587785252292473,0.,-0.809016994374948));
#15372=DIRECTION('center_axis',(0.,-1.,0.));
#15373=DIRECTION('ref_axis',(1.,0.,0.));
#15374=DIRECTION('',(-0.453990499739547,0.,-0.891006524188368));
#15375=DIRECTION('center_axis',(0.,-1.,0.));
#15376=DIRECTION('ref_axis',(1.,0.,0.));
#15377=DIRECTION('',(-0.309016994374947,0.,-0.951056516295154));
#15378=DIRECTION('center_axis',(0.,-1.,0.));
#15379=DIRECTION('ref_axis',(1.,0.,0.));
#15380=DIRECTION('',(-0.156434465040231,0.,-0.987688340595138));
#15381=DIRECTION('center_axis',(0.,-1.,0.));
#15382=DIRECTION('ref_axis',(1.,0.,0.));
#15383=DIRECTION('',(1.22464679914735E-16,0.,-1.));
#15384=DIRECTION('center_axis',(0.,-1.,0.));
#15385=DIRECTION('ref_axis',(1.,0.,0.));
#15386=DIRECTION('',(0.156434465040231,0.,-0.987688340595138));
#15387=DIRECTION('center_axis',(0.,-1.,0.));
#15388=DIRECTION('ref_axis',(1.,0.,0.));
#15389=DIRECTION('',(0.309016994374948,0.,-0.951056516295154));
#15390=DIRECTION('center_axis',(0.,-1.,0.));
#15391=DIRECTION('ref_axis',(1.,0.,0.));
#15392=DIRECTION('',(0.453990499739547,0.,-0.891006524188368));
#15393=DIRECTION('center_axis',(0.,-1.,0.));
#15394=DIRECTION('ref_axis',(1.,0.,0.));
#15395=DIRECTION('',(0.587785252292473,0.,-0.809016994374947));
#15396=DIRECTION('center_axis',(0.,-1.,0.));
#15397=DIRECTION('ref_axis',(1.,0.,0.));
#15398=DIRECTION('',(0.707106781186548,0.,-0.707106781186547));
#15399=DIRECTION('center_axis',(0.,-1.,0.));
#15400=DIRECTION('ref_axis',(1.,0.,0.));
#15401=DIRECTION('',(0.809016994374948,0.,-0.587785252292473));
#15402=DIRECTION('center_axis',(0.,-1.,0.));
#15403=DIRECTION('ref_axis',(1.,0.,0.));
#15404=DIRECTION('',(0.891006524188368,0.,-0.453990499739547));
#15405=DIRECTION('center_axis',(0.,-1.,0.));
#15406=DIRECTION('ref_axis',(1.,0.,0.));
#15407=DIRECTION('',(0.951056516295154,0.,-0.309016994374947));
#15408=DIRECTION('center_axis',(0.,-1.,0.));
#15409=DIRECTION('ref_axis',(1.,0.,0.));
#15410=DIRECTION('',(0.987688340595138,0.,-0.156434465040231));
#15411=DIRECTION('center_axis',(0.,-1.,0.));
#15412=DIRECTION('ref_axis',(1.,0.,0.));
#15413=DIRECTION('',(1.,0.,6.12323399573677E-17));
#15414=DIRECTION('center_axis',(0.,-1.,0.));
#15415=DIRECTION('ref_axis',(1.,0.,0.));
#15416=DIRECTION('',(0.987688340595138,0.,0.156434465040231));
#15417=DIRECTION('center_axis',(0.,-1.,0.));
#15418=DIRECTION('ref_axis',(1.,0.,0.));
#15419=DIRECTION('',(0.951056516295154,0.,0.309016994374948));
#15420=DIRECTION('center_axis',(0.,-1.,0.));
#15421=DIRECTION('ref_axis',(1.,0.,0.));
#15422=DIRECTION('',(0.891006524188368,0.,0.453990499739547));
#15423=DIRECTION('center_axis',(0.,-1.,0.));
#15424=DIRECTION('ref_axis',(1.,0.,0.));
#15425=DIRECTION('',(0.809016994374947,0.,0.587785252292473));
#15426=DIRECTION('center_axis',(0.,-1.,0.));
#15427=DIRECTION('ref_axis',(1.,0.,0.));
#15428=DIRECTION('',(0.707106781186547,0.,0.707106781186548));
#15429=DIRECTION('center_axis',(0.,-1.,0.));
#15430=DIRECTION('ref_axis',(1.,0.,0.));
#15431=DIRECTION('',(0.587785252292473,0.,0.809016994374947));
#15432=DIRECTION('center_axis',(0.,-1.,0.));
#15433=DIRECTION('ref_axis',(1.,0.,0.));
#15434=DIRECTION('',(0.453990499739547,0.,0.891006524188368));
#15435=DIRECTION('center_axis',(0.,-1.,0.));
#15436=DIRECTION('ref_axis',(1.,0.,0.));
#15437=DIRECTION('',(0.309016994374947,0.,0.951056516295154));
#15438=DIRECTION('center_axis',(0.,-1.,0.));
#15439=DIRECTION('ref_axis',(1.,0.,0.));
#15440=DIRECTION('',(0.156434465040231,0.,0.987688340595138));
#15441=DIRECTION('center_axis',(0.,-1.,0.));
#15442=DIRECTION('ref_axis',(1.,0.,0.));
#15443=DIRECTION('',(0.,0.,1.));
#15444=DIRECTION('center_axis',(0.,-1.,0.));
#15445=DIRECTION('ref_axis',(1.,0.,0.));
#15446=DIRECTION('',(-0.156434465040231,0.,0.987688340595138));
#15447=DIRECTION('center_axis',(0.,1.,0.));
#15448=DIRECTION('ref_axis',(1.,0.,0.));
#15449=DIRECTION('center_axis',(0.,1.,0.));
#15450=DIRECTION('ref_axis',(6.12323399573677E-17,0.,1.));
#15451=DIRECTION('center_axis',(0.,-1.,0.));
#15452=DIRECTION('ref_axis',(1.,0.,0.));
#15453=DIRECTION('center_axis',(0.,1.,0.));
#15454=DIRECTION('ref_axis',(1.,0.,0.));
#15455=DIRECTION('center_axis',(0.,1.,0.));
#15456=DIRECTION('ref_axis',(1.,0.,0.));
#15457=DIRECTION('',(0.,-1.,0.));
#15458=DIRECTION('center_axis',(0.,-1.,0.));
#15459=DIRECTION('ref_axis',(1.,0.,0.));
#15460=DIRECTION('center_axis',(0.,1.,0.));
#15461=DIRECTION('ref_axis',(1.,0.,0.));
#15462=DIRECTION('',(0.,1.,0.));
#15463=DIRECTION('',(0.,1.,0.));
#15464=DIRECTION('center_axis',(0.987688340595138,0.,0.156434465040231));
#15465=DIRECTION('ref_axis',(0.156434465040231,0.,-0.987688340595138));
#15466=DIRECTION('',(0.156434465040231,0.,-0.987688340595138));
#15467=DIRECTION('center_axis',(0.,1.,0.));
#15468=DIRECTION('ref_axis',(1.,0.,0.));
#15469=DIRECTION('center_axis',(0.,1.,0.));
#15470=DIRECTION('ref_axis',(1.,0.,0.));
#15471=DIRECTION('',(0.,1.,0.));
#15472=DIRECTION('',(0.,1.,0.));
#15473=DIRECTION('center_axis',(0.951056516295154,0.,0.309016994374948));
#15474=DIRECTION('ref_axis',(0.309016994374948,0.,-0.951056516295154));
#15475=DIRECTION('',(0.309016994374948,0.,-0.951056516295154));
#15476=DIRECTION('center_axis',(0.,1.,0.));
#15477=DIRECTION('ref_axis',(1.,0.,0.));
#15478=DIRECTION('center_axis',(0.,1.,0.));
#15479=DIRECTION('ref_axis',(1.,0.,0.));
#15480=DIRECTION('',(0.,1.,0.));
#15481=DIRECTION('',(0.,1.,0.));
#15482=DIRECTION('center_axis',(0.891006524188368,0.,0.453990499739547));
#15483=DIRECTION('ref_axis',(0.453990499739547,0.,-0.891006524188368));
#15484=DIRECTION('',(0.453990499739547,0.,-0.891006524188368));
#15485=DIRECTION('center_axis',(0.,1.,0.));
#15486=DIRECTION('ref_axis',(1.,0.,0.));
#15487=DIRECTION('center_axis',(0.,1.,0.));
#15488=DIRECTION('ref_axis',(1.,0.,0.));
#15489=DIRECTION('',(0.,1.,0.));
#15490=DIRECTION('',(0.,1.,0.));
#15491=DIRECTION('center_axis',(0.809016994374947,0.,0.587785252292473));
#15492=DIRECTION('ref_axis',(0.587785252292473,0.,-0.809016994374947));
#15493=DIRECTION('',(0.587785252292473,0.,-0.809016994374947));
#15494=DIRECTION('center_axis',(0.,1.,0.));
#15495=DIRECTION('ref_axis',(1.,0.,0.));
#15496=DIRECTION('center_axis',(0.,1.,0.));
#15497=DIRECTION('ref_axis',(1.,0.,0.));
#15498=DIRECTION('',(0.,1.,0.));
#15499=DIRECTION('',(0.,1.,0.));
#15500=DIRECTION('center_axis',(0.707106781186547,0.,0.707106781186548));
#15501=DIRECTION('ref_axis',(0.707106781186548,0.,-0.707106781186547));
#15502=DIRECTION('',(0.707106781186548,0.,-0.707106781186547));
#15503=DIRECTION('center_axis',(0.,1.,0.));
#15504=DIRECTION('ref_axis',(1.,0.,0.));
#15505=DIRECTION('center_axis',(0.,1.,0.));
#15506=DIRECTION('ref_axis',(1.,0.,0.));
#15507=DIRECTION('',(0.,1.,0.));
#15508=DIRECTION('',(0.,1.,0.));
#15509=DIRECTION('center_axis',(0.587785252292473,0.,0.809016994374948));
#15510=DIRECTION('ref_axis',(0.809016994374948,0.,-0.587785252292473));
#15511=DIRECTION('',(0.809016994374948,0.,-0.587785252292473));
#15512=DIRECTION('center_axis',(0.,1.,0.));
#15513=DIRECTION('ref_axis',(1.,0.,0.));
#15514=DIRECTION('center_axis',(0.,1.,0.));
#15515=DIRECTION('ref_axis',(1.,0.,0.));
#15516=DIRECTION('',(0.,1.,0.));
#15517=DIRECTION('',(0.,1.,0.));
#15518=DIRECTION('center_axis',(0.453990499739547,0.,0.891006524188368));
#15519=DIRECTION('ref_axis',(0.891006524188368,0.,-0.453990499739547));
#15520=DIRECTION('',(0.891006524188368,0.,-0.453990499739547));
#15521=DIRECTION('center_axis',(0.,1.,0.));
#15522=DIRECTION('ref_axis',(1.,0.,0.));
#15523=DIRECTION('center_axis',(0.,1.,0.));
#15524=DIRECTION('ref_axis',(1.,0.,0.));
#15525=DIRECTION('',(0.,1.,0.));
#15526=DIRECTION('',(0.,1.,0.));
#15527=DIRECTION('center_axis',(0.309016994374947,0.,0.951056516295154));
#15528=DIRECTION('ref_axis',(0.951056516295154,0.,-0.309016994374947));
#15529=DIRECTION('',(0.951056516295154,0.,-0.309016994374947));
#15530=DIRECTION('center_axis',(0.,1.,0.));
#15531=DIRECTION('ref_axis',(1.,0.,0.));
#15532=DIRECTION('center_axis',(0.,1.,0.));
#15533=DIRECTION('ref_axis',(1.,0.,0.));
#15534=DIRECTION('',(0.,1.,0.));
#15535=DIRECTION('',(0.,1.,0.));
#15536=DIRECTION('center_axis',(0.156434465040231,0.,0.987688340595138));
#15537=DIRECTION('ref_axis',(0.987688340595138,0.,-0.156434465040231));
#15538=DIRECTION('',(0.987688340595138,0.,-0.156434465040231));
#15539=DIRECTION('center_axis',(0.,1.,0.));
#15540=DIRECTION('ref_axis',(1.,0.,0.));
#15541=DIRECTION('center_axis',(0.,1.,0.));
#15542=DIRECTION('ref_axis',(1.,0.,0.));
#15543=DIRECTION('',(0.,1.,0.));
#15544=DIRECTION('',(0.,1.,0.));
#15545=DIRECTION('center_axis',(-1.83697019872103E-16,0.,1.));
#15546=DIRECTION('ref_axis',(1.,0.,1.83697019872103E-16));
#15547=DIRECTION('',(1.,0.,1.83697019872103E-16));
#15548=DIRECTION('center_axis',(0.,1.,0.));
#15549=DIRECTION('ref_axis',(1.,0.,0.));
#15550=DIRECTION('center_axis',(0.,1.,0.));
#15551=DIRECTION('ref_axis',(1.,0.,0.));
#15552=DIRECTION('',(0.,1.,0.));
#15553=DIRECTION('',(0.,1.,0.));
#15554=DIRECTION('center_axis',(-0.156434465040231,0.,0.987688340595138));
#15555=DIRECTION('ref_axis',(0.987688340595138,0.,0.156434465040231));
#15556=DIRECTION('',(0.987688340595138,0.,0.156434465040231));
#15557=DIRECTION('center_axis',(0.,1.,0.));
#15558=DIRECTION('ref_axis',(1.,0.,0.));
#15559=DIRECTION('center_axis',(0.,1.,0.));
#15560=DIRECTION('ref_axis',(1.,0.,0.));
#15561=DIRECTION('',(0.,1.,0.));
#15562=DIRECTION('',(0.,1.,0.));
#15563=DIRECTION('center_axis',(-0.309016994374948,0.,0.951056516295154));
#15564=DIRECTION('ref_axis',(0.951056516295154,0.,0.309016994374948));
#15565=DIRECTION('',(0.951056516295154,0.,0.309016994374948));
#15566=DIRECTION('center_axis',(0.,1.,0.));
#15567=DIRECTION('ref_axis',(1.,0.,0.));
#15568=DIRECTION('center_axis',(0.,1.,0.));
#15569=DIRECTION('ref_axis',(1.,0.,0.));
#15570=DIRECTION('',(0.,1.,0.));
#15571=DIRECTION('',(0.,1.,0.));
#15572=DIRECTION('center_axis',(-0.453990499739547,0.,0.891006524188368));
#15573=DIRECTION('ref_axis',(0.891006524188368,0.,0.453990499739547));
#15574=DIRECTION('',(0.891006524188368,0.,0.453990499739547));
#15575=DIRECTION('center_axis',(0.,1.,0.));
#15576=DIRECTION('ref_axis',(1.,0.,0.));
#15577=DIRECTION('center_axis',(0.,1.,0.));
#15578=DIRECTION('ref_axis',(1.,0.,0.));
#15579=DIRECTION('',(0.,1.,0.));
#15580=DIRECTION('',(0.,1.,0.));
#15581=DIRECTION('center_axis',(-0.587785252292473,0.,0.809016994374947));
#15582=DIRECTION('ref_axis',(0.809016994374947,0.,0.587785252292473));
#15583=DIRECTION('',(0.809016994374947,0.,0.587785252292473));
#15584=DIRECTION('center_axis',(0.,1.,0.));
#15585=DIRECTION('ref_axis',(1.,0.,0.));
#15586=DIRECTION('center_axis',(0.,1.,0.));
#15587=DIRECTION('ref_axis',(1.,0.,0.));
#15588=DIRECTION('',(0.,1.,0.));
#15589=DIRECTION('',(0.,1.,0.));
#15590=DIRECTION('center_axis',(-0.707106781186548,0.,0.707106781186547));
#15591=DIRECTION('ref_axis',(0.707106781186547,0.,0.707106781186548));
#15592=DIRECTION('',(0.707106781186547,0.,0.707106781186548));
#15593=DIRECTION('center_axis',(0.,1.,0.));
#15594=DIRECTION('ref_axis',(1.,0.,0.));
#15595=DIRECTION('center_axis',(0.,1.,0.));
#15596=DIRECTION('ref_axis',(1.,0.,0.));
#15597=DIRECTION('',(0.,1.,0.));
#15598=DIRECTION('',(0.,1.,0.));
#15599=DIRECTION('center_axis',(-0.809016994374948,0.,0.587785252292473));
#15600=DIRECTION('ref_axis',(0.587785252292473,0.,0.809016994374948));
#15601=DIRECTION('',(0.587785252292473,0.,0.809016994374948));
#15602=DIRECTION('center_axis',(0.,1.,0.));
#15603=DIRECTION('ref_axis',(1.,0.,0.));
#15604=DIRECTION('center_axis',(0.,1.,0.));
#15605=DIRECTION('ref_axis',(1.,0.,0.));
#15606=DIRECTION('',(0.,1.,0.));
#15607=DIRECTION('',(0.,1.,0.));
#15608=DIRECTION('center_axis',(-0.891006524188368,0.,0.453990499739547));
#15609=DIRECTION('ref_axis',(0.453990499739547,0.,0.891006524188368));
#15610=DIRECTION('',(0.453990499739547,0.,0.891006524188368));
#15611=DIRECTION('center_axis',(0.,1.,0.));
#15612=DIRECTION('ref_axis',(1.,0.,0.));
#15613=DIRECTION('center_axis',(0.,1.,0.));
#15614=DIRECTION('ref_axis',(1.,0.,0.));
#15615=DIRECTION('',(0.,1.,0.));
#15616=DIRECTION('',(0.,1.,0.));
#15617=DIRECTION('center_axis',(-0.951056516295154,0.,0.309016994374947));
#15618=DIRECTION('ref_axis',(0.309016994374947,0.,0.951056516295154));
#15619=DIRECTION('',(0.309016994374947,0.,0.951056516295154));
#15620=DIRECTION('center_axis',(0.,1.,0.));
#15621=DIRECTION('ref_axis',(1.,0.,0.));
#15622=DIRECTION('center_axis',(0.,1.,0.));
#15623=DIRECTION('ref_axis',(1.,0.,0.));
#15624=DIRECTION('',(0.,1.,0.));
#15625=DIRECTION('',(0.,1.,0.));
#15626=DIRECTION('center_axis',(-0.987688340595138,0.,0.156434465040231));
#15627=DIRECTION('ref_axis',(0.156434465040231,0.,0.987688340595138));
#15628=DIRECTION('',(0.156434465040231,0.,0.987688340595138));
#15629=DIRECTION('center_axis',(0.,1.,0.));
#15630=DIRECTION('ref_axis',(1.,0.,0.));
#15631=DIRECTION('center_axis',(0.,1.,0.));
#15632=DIRECTION('ref_axis',(1.,0.,0.));
#15633=DIRECTION('',(0.,1.,0.));
#15634=DIRECTION('',(0.,1.,0.));
#15635=DIRECTION('center_axis',(-1.,0.,-1.22464679914735E-16));
#15636=DIRECTION('ref_axis',(-1.22464679914735E-16,0.,1.));
#15637=DIRECTION('',(-1.22464679914735E-16,0.,1.));
#15638=DIRECTION('center_axis',(0.,1.,0.));
#15639=DIRECTION('ref_axis',(1.,0.,0.));
#15640=DIRECTION('center_axis',(0.,1.,0.));
#15641=DIRECTION('ref_axis',(1.,0.,0.));
#15642=DIRECTION('',(0.,1.,0.));
#15643=DIRECTION('',(0.,1.,0.));
#15644=DIRECTION('center_axis',(-0.987688340595138,0.,-0.156434465040231));
#15645=DIRECTION('ref_axis',(-0.156434465040231,0.,0.987688340595138));
#15646=DIRECTION('',(-0.156434465040231,0.,0.987688340595138));
#15647=DIRECTION('center_axis',(0.,1.,0.));
#15648=DIRECTION('ref_axis',(1.,0.,0.));
#15649=DIRECTION('center_axis',(0.,1.,0.));
#15650=DIRECTION('ref_axis',(1.,0.,0.));
#15651=DIRECTION('',(0.,1.,0.));
#15652=DIRECTION('',(0.,1.,0.));
#15653=DIRECTION('center_axis',(-0.951056516295154,0.,-0.309016994374948));
#15654=DIRECTION('ref_axis',(-0.309016994374948,0.,0.951056516295154));
#15655=DIRECTION('',(-0.309016994374948,0.,0.951056516295154));
#15656=DIRECTION('center_axis',(0.,1.,0.));
#15657=DIRECTION('ref_axis',(1.,0.,0.));
#15658=DIRECTION('center_axis',(0.,1.,0.));
#15659=DIRECTION('ref_axis',(1.,0.,0.));
#15660=DIRECTION('',(0.,1.,0.));
#15661=DIRECTION('',(0.,1.,0.));
#15662=DIRECTION('center_axis',(-0.891006524188368,0.,-0.453990499739547));
#15663=DIRECTION('ref_axis',(-0.453990499739547,0.,0.891006524188368));
#15664=DIRECTION('',(-0.453990499739547,0.,0.891006524188368));
#15665=DIRECTION('center_axis',(0.,1.,0.));
#15666=DIRECTION('ref_axis',(1.,0.,0.));
#15667=DIRECTION('center_axis',(0.,1.,0.));
#15668=DIRECTION('ref_axis',(1.,0.,0.));
#15669=DIRECTION('',(0.,1.,0.));
#15670=DIRECTION('',(0.,1.,0.));
#15671=DIRECTION('center_axis',(-0.809016994374947,0.,-0.587785252292473));
#15672=DIRECTION('ref_axis',(-0.587785252292473,0.,0.809016994374947));
#15673=DIRECTION('',(-0.587785252292473,0.,0.809016994374947));
#15674=DIRECTION('center_axis',(0.,1.,0.));
#15675=DIRECTION('ref_axis',(1.,0.,0.));
#15676=DIRECTION('center_axis',(0.,1.,0.));
#15677=DIRECTION('ref_axis',(1.,0.,0.));
#15678=DIRECTION('',(0.,1.,0.));
#15679=DIRECTION('',(0.,1.,0.));
#15680=DIRECTION('center_axis',(-0.707106781186547,0.,-0.707106781186548));
#15681=DIRECTION('ref_axis',(-0.707106781186548,0.,0.707106781186547));
#15682=DIRECTION('',(-0.707106781186548,0.,0.707106781186547));
#15683=DIRECTION('center_axis',(0.,1.,0.));
#15684=DIRECTION('ref_axis',(1.,0.,0.));
#15685=DIRECTION('center_axis',(0.,1.,0.));
#15686=DIRECTION('ref_axis',(1.,0.,0.));
#15687=DIRECTION('',(0.,1.,0.));
#15688=DIRECTION('',(0.,1.,0.));
#15689=DIRECTION('center_axis',(-0.587785252292473,0.,-0.809016994374948));
#15690=DIRECTION('ref_axis',(-0.809016994374948,0.,0.587785252292473));
#15691=DIRECTION('',(-0.809016994374948,0.,0.587785252292473));
#15692=DIRECTION('center_axis',(0.,1.,0.));
#15693=DIRECTION('ref_axis',(1.,0.,0.));
#15694=DIRECTION('center_axis',(0.,1.,0.));
#15695=DIRECTION('ref_axis',(1.,0.,0.));
#15696=DIRECTION('',(0.,1.,0.));
#15697=DIRECTION('',(0.,1.,0.));
#15698=DIRECTION('center_axis',(-0.453990499739547,0.,-0.891006524188368));
#15699=DIRECTION('ref_axis',(-0.891006524188368,0.,0.453990499739547));
#15700=DIRECTION('',(-0.891006524188368,0.,0.453990499739547));
#15701=DIRECTION('center_axis',(0.,1.,0.));
#15702=DIRECTION('ref_axis',(1.,0.,0.));
#15703=DIRECTION('center_axis',(0.,1.,0.));
#15704=DIRECTION('ref_axis',(1.,0.,0.));
#15705=DIRECTION('',(0.,1.,0.));
#15706=DIRECTION('',(0.,1.,0.));
#15707=DIRECTION('center_axis',(-0.309016994374947,0.,-0.951056516295154));
#15708=DIRECTION('ref_axis',(-0.951056516295154,0.,0.309016994374947));
#15709=DIRECTION('',(-0.951056516295154,0.,0.309016994374947));
#15710=DIRECTION('center_axis',(0.,1.,0.));
#15711=DIRECTION('ref_axis',(1.,0.,0.));
#15712=DIRECTION('center_axis',(0.,1.,0.));
#15713=DIRECTION('ref_axis',(1.,0.,0.));
#15714=DIRECTION('',(0.,1.,0.));
#15715=DIRECTION('',(0.,1.,0.));
#15716=DIRECTION('center_axis',(-0.156434465040231,0.,-0.987688340595138));
#15717=DIRECTION('ref_axis',(-0.987688340595138,0.,0.156434465040231));
#15718=DIRECTION('',(-0.987688340595138,0.,0.156434465040231));
#15719=DIRECTION('center_axis',(0.,1.,0.));
#15720=DIRECTION('ref_axis',(1.,0.,0.));
#15721=DIRECTION('center_axis',(0.,1.,0.));
#15722=DIRECTION('ref_axis',(1.,0.,0.));
#15723=DIRECTION('',(0.,1.,0.));
#15724=DIRECTION('',(0.,1.,0.));
#15725=DIRECTION('center_axis',(6.12323399573677E-17,0.,-1.));
#15726=DIRECTION('ref_axis',(-1.,0.,-6.12323399573677E-17));
#15727=DIRECTION('',(-1.,0.,-6.12323399573677E-17));
#15728=DIRECTION('center_axis',(0.,1.,0.));
#15729=DIRECTION('ref_axis',(1.,0.,0.));
#15730=DIRECTION('center_axis',(0.,1.,0.));
#15731=DIRECTION('ref_axis',(1.,0.,0.));
#15732=DIRECTION('',(0.,1.,0.));
#15733=DIRECTION('',(0.,1.,0.));
#15734=DIRECTION('center_axis',(0.156434465040231,0.,-0.987688340595138));
#15735=DIRECTION('ref_axis',(-0.987688340595138,0.,-0.156434465040231));
#15736=DIRECTION('',(-0.987688340595138,0.,-0.156434465040231));
#15737=DIRECTION('center_axis',(0.,1.,0.));
#15738=DIRECTION('ref_axis',(1.,0.,0.));
#15739=DIRECTION('center_axis',(0.,1.,0.));
#15740=DIRECTION('ref_axis',(1.,0.,0.));
#15741=DIRECTION('',(0.,1.,0.));
#15742=DIRECTION('',(0.,1.,0.));
#15743=DIRECTION('center_axis',(0.309016994374948,0.,-0.951056516295154));
#15744=DIRECTION('ref_axis',(-0.951056516295154,0.,-0.309016994374948));
#15745=DIRECTION('',(-0.951056516295154,0.,-0.309016994374948));
#15746=DIRECTION('center_axis',(0.,1.,0.));
#15747=DIRECTION('ref_axis',(1.,0.,0.));
#15748=DIRECTION('center_axis',(0.,1.,0.));
#15749=DIRECTION('ref_axis',(1.,0.,0.));
#15750=DIRECTION('',(0.,1.,0.));
#15751=DIRECTION('',(0.,1.,0.));
#15752=DIRECTION('center_axis',(0.453990499739547,0.,-0.891006524188368));
#15753=DIRECTION('ref_axis',(-0.891006524188368,0.,-0.453990499739547));
#15754=DIRECTION('',(-0.891006524188368,0.,-0.453990499739547));
#15755=DIRECTION('center_axis',(0.,1.,0.));
#15756=DIRECTION('ref_axis',(1.,0.,0.));
#15757=DIRECTION('center_axis',(0.,1.,0.));
#15758=DIRECTION('ref_axis',(1.,0.,0.));
#15759=DIRECTION('',(0.,1.,0.));
#15760=DIRECTION('',(0.,1.,0.));
#15761=DIRECTION('center_axis',(0.587785252292473,0.,-0.809016994374947));
#15762=DIRECTION('ref_axis',(-0.809016994374947,0.,-0.587785252292473));
#15763=DIRECTION('',(-0.809016994374947,0.,-0.587785252292473));
#15764=DIRECTION('center_axis',(0.,1.,0.));
#15765=DIRECTION('ref_axis',(1.,0.,0.));
#15766=DIRECTION('center_axis',(0.,1.,0.));
#15767=DIRECTION('ref_axis',(1.,0.,0.));
#15768=DIRECTION('',(0.,1.,0.));
#15769=DIRECTION('',(0.,1.,0.));
#15770=DIRECTION('center_axis',(0.707106781186548,0.,-0.707106781186547));
#15771=DIRECTION('ref_axis',(-0.707106781186547,0.,-0.707106781186548));
#15772=DIRECTION('',(-0.707106781186547,0.,-0.707106781186548));
#15773=DIRECTION('center_axis',(0.,1.,0.));
#15774=DIRECTION('ref_axis',(1.,0.,0.));
#15775=DIRECTION('center_axis',(0.,1.,0.));
#15776=DIRECTION('ref_axis',(1.,0.,0.));
#15777=DIRECTION('',(0.,1.,0.));
#15778=DIRECTION('',(0.,1.,0.));
#15779=DIRECTION('center_axis',(0.809016994374947,0.,-0.587785252292473));
#15780=DIRECTION('ref_axis',(-0.587785252292473,0.,-0.809016994374947));
#15781=DIRECTION('',(-0.587785252292473,0.,-0.809016994374947));
#15782=DIRECTION('center_axis',(0.,1.,0.));
#15783=DIRECTION('ref_axis',(1.,0.,0.));
#15784=DIRECTION('center_axis',(0.,1.,0.));
#15785=DIRECTION('ref_axis',(1.,0.,0.));
#15786=DIRECTION('',(0.,1.,0.));
#15787=DIRECTION('',(0.,1.,0.));
#15788=DIRECTION('center_axis',(0.891006524188368,0.,-0.453990499739547));
#15789=DIRECTION('ref_axis',(-0.453990499739547,0.,-0.891006524188368));
#15790=DIRECTION('',(-0.453990499739547,0.,-0.891006524188368));
#15791=DIRECTION('center_axis',(0.,1.,0.));
#15792=DIRECTION('ref_axis',(1.,0.,0.));
#15793=DIRECTION('center_axis',(0.,1.,0.));
#15794=DIRECTION('ref_axis',(1.,0.,0.));
#15795=DIRECTION('',(0.,1.,0.));
#15796=DIRECTION('',(0.,1.,0.));
#15797=DIRECTION('center_axis',(0.951056516295154,0.,-0.309016994374947));
#15798=DIRECTION('ref_axis',(-0.309016994374947,0.,-0.951056516295154));
#15799=DIRECTION('',(-0.309016994374947,0.,-0.951056516295154));
#15800=DIRECTION('center_axis',(0.,1.,0.));
#15801=DIRECTION('ref_axis',(1.,0.,0.));
#15802=DIRECTION('center_axis',(0.,1.,0.));
#15803=DIRECTION('ref_axis',(1.,0.,0.));
#15804=DIRECTION('',(0.,1.,0.));
#15805=DIRECTION('center_axis',(0.987688340595138,0.,-0.156434465040231));
#15806=DIRECTION('ref_axis',(-0.156434465040231,0.,-0.987688340595138));
#15807=DIRECTION('',(-0.156434465040231,0.,-0.987688340595138));
#15808=DIRECTION('',(0.,1.,0.));
#15809=DIRECTION('center_axis',(0.,1.,0.));
#15810=DIRECTION('ref_axis',(1.,0.,0.));
#15811=DIRECTION('center_axis',(0.,1.,0.));
#15812=DIRECTION('ref_axis',(1.,0.,0.));
#15813=DIRECTION('',(0.,1.,0.));
#15814=DIRECTION('',(0.,1.,0.));
#15815=DIRECTION('center_axis',(1.,0.,0.));
#15816=DIRECTION('ref_axis',(0.,0.,-1.));
#15817=DIRECTION('',(0.,0.,-1.));
#15818=DIRECTION('center_axis',(0.,1.,0.));
#15819=DIRECTION('ref_axis',(1.,0.,0.));
#15820=DIRECTION('center_axis',(0.,1.,0.));
#15821=DIRECTION('ref_axis',(1.,0.,0.));
#15822=DIRECTION('center_axis',(0.,1.,0.));
#15823=DIRECTION('ref_axis',(1.,0.,0.));
#15824=DIRECTION('axis',(0.,0.,1.));
#15825=DIRECTION('refdir',(1.,0.,0.));
#15826=DIRECTION('center_axis',(1.,0.,0.));
#15827=DIRECTION('ref_axis',(0.,0.,-1.));
#15828=DIRECTION('',(0.,-0.707106781186547,-0.707106781186548));
#15829=DIRECTION('',(0.,-1.,0.));
#15830=DIRECTION('',(0.,-0.707106781186547,0.707106781186548));
#15831=DIRECTION('',(0.,0.,1.));
#15832=DIRECTION('',(0.,0.707106781186547,0.707106781186548));
#15833=DIRECTION('',(0.,1.,0.));
#15834=DIRECTION('',(0.,0.707106781186547,-0.707106781186548));
#15835=DIRECTION('',(0.,0.,-1.));
#15836=DIRECTION('center_axis',(0.,0.707106781186548,-0.707106781186547));
#15837=DIRECTION('ref_axis',(-1.,0.,0.));
#15838=DIRECTION('',(1.,0.,0.));
#15839=DIRECTION('',(0.,-0.707106781186547,-0.707106781186548));
#15840=DIRECTION('',(-1.,0.,0.));
#15841=DIRECTION('center_axis',(0.,1.,0.));
#15842=DIRECTION('ref_axis',(-1.,0.,0.));
#15843=DIRECTION('',(-1.,0.,0.));
#15844=DIRECTION('',(0.,0.,-1.));
#15845=DIRECTION('center_axis',(0.,0.707106781186548,0.707106781186547));
#15846=DIRECTION('ref_axis',(1.,0.,0.));
#15847=DIRECTION('',(1.,0.,0.));
#15848=DIRECTION('',(0.,0.707106781186547,-0.707106781186548));
#15849=DIRECTION('center_axis',(0.,0.,1.));
#15850=DIRECTION('ref_axis',(1.,0.,0.));
#15851=DIRECTION('',(-1.,0.,0.));
#15852=DIRECTION('',(0.,1.,0.));
#15853=DIRECTION('center_axis',(1.,0.,0.));
#15854=DIRECTION('ref_axis',(0.,0.,-1.));
#15855=DIRECTION('',(0.,-0.707106781186547,0.707106781186548));
#15856=DIRECTION('',(0.,-1.,0.));
#15857=DIRECTION('',(0.,0.707106781186547,0.707106781186548));
#15858=DIRECTION('',(0.,0.,1.));
#15859=DIRECTION('center_axis',(0.,0.,1.));
#15860=DIRECTION('ref_axis',(1.,0.,0.));
#15861=DIRECTION('',(1.,0.,0.));
#15862=DIRECTION('center_axis',(0.,-0.707106781186548,0.707106781186547));
#15863=DIRECTION('ref_axis',(1.,0.,0.));
#15864=DIRECTION('',(1.,0.,0.));
#15865=DIRECTION('center_axis',(0.,-0.707106781186548,-0.707106781186547));
#15866=DIRECTION('ref_axis',(-1.,0.,0.));
#15867=DIRECTION('',(-1.,0.,0.));
#15868=DIRECTION('center_axis',(0.,-1.,0.));
#15869=DIRECTION('ref_axis',(1.,0.,0.));
#15870=DIRECTION('axis',(0.,0.,1.));
#15871=DIRECTION('refdir',(1.,0.,0.));
#15872=DIRECTION('center_axis',(0.866025403784439,0.,-0.5));
#15873=DIRECTION('ref_axis',(0.5,0.,0.866025403784439));
#15874=DIRECTION('',(0.5,0.,0.866025403784439));
#15875=DIRECTION('',(0.,-1.,0.));
#15876=DIRECTION('',(0.5,0.,0.866025403784439));
#15877=DIRECTION('',(0.,-1.,0.));
#15878=DIRECTION('center_axis',(1.92296268638356E-16,0.,-1.));
#15879=DIRECTION('ref_axis',(1.,0.,1.92296268638356E-16));
#15880=DIRECTION('',(1.,0.,1.92296268638356E-16));
#15881=DIRECTION('',(0.,-1.,0.));
#15882=DIRECTION('',(1.,0.,1.92296268638356E-16));
#15883=DIRECTION('center_axis',(-0.866025403784439,0.,-0.5));
#15884=DIRECTION('ref_axis',(0.5,0.,-0.866025403784439));
#15885=DIRECTION('',(0.5,0.,-0.866025403784439));
#15886=DIRECTION('',(0.,-1.,0.));
#15887=DIRECTION('',(0.5,0.,-0.866025403784438));
#15888=DIRECTION('center_axis',(-0.866025403784439,0.,0.5));
#15889=DIRECTION('ref_axis',(-0.5,0.,-0.866025403784439));
#15890=DIRECTION('',(-0.5,0.,-0.866025403784439));
#15891=DIRECTION('',(0.,-1.,0.));
#15892=DIRECTION('',(-0.5,0.,-0.866025403784439));
#15893=DIRECTION('center_axis',(-1.92296268638356E-16,0.,1.));
#15894=DIRECTION('ref_axis',(-1.,0.,-1.92296268638356E-16));
#15895=DIRECTION('',(-1.,0.,-1.92296268638356E-16));
#15896=DIRECTION('',(0.,-1.,0.));
#15897=DIRECTION('',(-1.,0.,-1.92296268638356E-16));
#15898=DIRECTION('center_axis',(0.866025403784439,0.,0.5));
#15899=DIRECTION('ref_axis',(-0.5,0.,0.866025403784439));
#15900=DIRECTION('',(-0.5,0.,0.866025403784439));
#15901=DIRECTION('',(-0.5,0.,0.866025403784439));
#15902=DIRECTION('center_axis',(0.,-1.,0.));
#15903=DIRECTION('ref_axis',(0.,0.,-1.));
#15904=DIRECTION('center_axis',(0.,1.,0.));
#15905=DIRECTION('ref_axis',(0.,0.,1.));
#15906=DIRECTION('center_axis',(0.,-1.,0.));
#15907=DIRECTION('ref_axis',(1.,0.,0.));
#15908=DIRECTION('center_axis',(0.,-1.,0.));
#15909=DIRECTION('ref_axis',(1.,0.,0.));
#15910=DIRECTION('center_axis',(0.,-1.,0.));
#15911=DIRECTION('ref_axis',(1.,0.,0.));
#15912=DIRECTION('',(0.707106781186547,0.707106781186548,8.65956056235493E-17));
#15913=DIRECTION('center_axis',(0.,-1.,0.));
#15914=DIRECTION('ref_axis',(1.,0.,0.));
#15915=DIRECTION('center_axis',(0.,1.,0.));
#15916=DIRECTION('ref_axis',(1.,0.,0.));
#15917=DIRECTION('',(0.,1.,0.));
#15918=DIRECTION('center_axis',(0.,1.,0.));
#15919=DIRECTION('ref_axis',(1.,0.,0.));
#15920=DIRECTION('center_axis',(0.,-1.,0.));
#15921=DIRECTION('ref_axis',(1.,0.,0.));
#15922=DIRECTION('',(-0.707106781186547,0.707106781186548,-8.65956056235493E-17));
#15923=DIRECTION('center_axis',(0.,-1.,0.));
#15924=DIRECTION('ref_axis',(0.,0.,-1.));
#15925=DIRECTION('',(0.,0.,1.));
#15926=DIRECTION('',(1.,0.,0.));
#15927=DIRECTION('',(0.,0.,1.));
#15928=DIRECTION('',(1.,0.,0.));
#15929=DIRECTION('',(0.,0.,1.));
#15930=DIRECTION('',(1.,0.,0.));
#15931=DIRECTION('',(0.,0.,1.));
#15932=DIRECTION('',(1.,0.,0.));
#15933=DIRECTION('',(0.,0.,1.));
#15934=DIRECTION('',(1.,0.,0.));
#15935=DIRECTION('',(0.,0.,1.));
#15936=DIRECTION('',(1.,0.,0.));
#15937=DIRECTION('',(0.,0.,1.));
#15938=DIRECTION('',(1.,0.,0.));
#15939=DIRECTION('',(0.,0.,1.));
#15940=DIRECTION('',(1.,0.,0.));
#15941=DIRECTION('',(8.65956056235493E-17,-8.65956056235493E-17,-1.));
#15942=DIRECTION('',(2.22044604925031E-16,1.,-8.65956056235494E-17));
#15943=DIRECTION('',(0.,-1.,2.22044604925031E-16));
#15944=DIRECTION('',(1.,0.,0.));
#15945=DIRECTION('',(0.,-1.,2.22044604925031E-16));
#15946=DIRECTION('',(1.,0.,0.));
#15947=DIRECTION('',(0.,0.,1.));
#15948=DIRECTION('',(1.,0.,0.));
#15949=DIRECTION('',(0.,0.,1.));
#15950=DIRECTION('',(1.,0.,0.));
#15951=DIRECTION('',(0.,0.,1.));
#15952=DIRECTION('',(1.,0.,0.));
#15953=DIRECTION('',(0.,0.,1.));
#15954=DIRECTION('',(1.,0.,0.));
#15955=DIRECTION('',(0.,0.,1.));
#15956=DIRECTION('',(1.,0.,0.));
#15957=DIRECTION('',(0.,0.,1.));
#15958=DIRECTION('',(1.,0.,0.));
#15959=DIRECTION('',(0.,0.,1.));
#15960=DIRECTION('',(1.,0.,0.));
#15961=DIRECTION('',(0.,0.,1.));
#15962=DIRECTION('',(1.,0.,0.));
#15963=DIRECTION('',(8.65956056235493E-17,-8.65956056235493E-17,-1.));
#15964=DIRECTION('',(2.22044604925031E-16,1.,-8.65956056235494E-17));
#15965=DIRECTION('',(0.,-1.,2.22044604925031E-16));
#15966=DIRECTION('',(1.,0.,0.));
#15967=DIRECTION('',(0.,-1.,2.22044604925031E-16));
#15968=DIRECTION('',(1.,0.,0.));
#15969=DIRECTION('',(0.,0.,1.));
#15970=DIRECTION('',(1.,0.,0.));
#15971=DIRECTION('',(0.,0.,1.));
#15972=DIRECTION('',(1.,0.,0.));
#15973=DIRECTION('',(0.0784590957278449,0.,0.996917333733128));
#15974=DIRECTION('',(0.996917333733128,0.,-0.0784590957278449));
#15975=CARTESIAN_POINT('',(0.,0.,0.));
#15976=CARTESIAN_POINT('',(0.,0.,0.));
#15977=CARTESIAN_POINT('',(0.,0.,0.));
#15978=CARTESIAN_POINT('Origin',(10.,-3.5,-1.1));
#15979=CARTESIAN_POINT('',(9.67,-3.5,-1.));
#15980=CARTESIAN_POINT('Origin',(10.,-3.5,-1.));
#15981=CARTESIAN_POINT('',(9.67,-3.5,0.));
#15982=CARTESIAN_POINT('',(9.67,-3.5,-1.1));
#15983=CARTESIAN_POINT('Origin',(10.,-3.5,0.));
#15984=CARTESIAN_POINT('Origin',(-2.,3.5,-1.1));
#15985=CARTESIAN_POINT('',(-2.33,3.5,-1.));
#15986=CARTESIAN_POINT('Origin',(-2.,3.5,-1.));
#15987=CARTESIAN_POINT('',(-2.33,3.5,0.));
#15988=CARTESIAN_POINT('',(-2.33,3.5,-1.1));
#15989=CARTESIAN_POINT('Origin',(-2.,3.5,0.));
#15990=CARTESIAN_POINT('Origin',(-2.,-3.5,-1.1));
#15991=CARTESIAN_POINT('',(-2.33,-3.5,-1.));
#15992=CARTESIAN_POINT('Origin',(-2.,-3.5,-1.));
#15993=CARTESIAN_POINT('',(-2.33,-3.5,0.));
#15994=CARTESIAN_POINT('',(-2.33,-3.5,-1.1));
#15995=CARTESIAN_POINT('Origin',(-2.,-3.5,0.));
#15996=CARTESIAN_POINT('Origin',(10.,3.5,-1.1));
#15997=CARTESIAN_POINT('',(9.67,3.5,-1.));
#15998=CARTESIAN_POINT('Origin',(10.,3.5,-1.));
#15999=CARTESIAN_POINT('',(9.67,3.5,0.));
#16000=CARTESIAN_POINT('',(9.67,3.5,-1.1));
#16001=CARTESIAN_POINT('Origin',(10.,3.5,0.));
#16002=CARTESIAN_POINT('Origin',(12.,5.4,-1.));
#16003=CARTESIAN_POINT('',(12.,5.4,-1.));
#16004=CARTESIAN_POINT('',(-4.,5.4,-1.));
#16005=CARTESIAN_POINT('',(12.,5.4,-1.));
#16006=CARTESIAN_POINT('',(-4.,5.4,0.));
#16007=CARTESIAN_POINT('',(-4.,5.4,-1.));
#16008=CARTESIAN_POINT('',(12.,5.4,0.));
#16009=CARTESIAN_POINT('',(12.,5.4,0.));
#16010=CARTESIAN_POINT('',(12.,5.4,-1.));
#16011=CARTESIAN_POINT('Origin',(12.,-5.4,-1.));
#16012=CARTESIAN_POINT('',(12.,-5.4,-1.));
#16013=CARTESIAN_POINT('',(12.,-5.4,-1.));
#16014=CARTESIAN_POINT('',(12.,-5.4,0.));
#16015=CARTESIAN_POINT('',(12.,-5.4,0.));
#16016=CARTESIAN_POINT('',(12.,-5.4,-1.));
#16017=CARTESIAN_POINT('Origin',(-4.,-5.4,-1.));
#16018=CARTESIAN_POINT('',(-4.,-5.4,-1.));
#16019=CARTESIAN_POINT('',(-4.,-5.4,-1.));
#16020=CARTESIAN_POINT('',(-4.,-5.4,0.));
#16021=CARTESIAN_POINT('',(-4.,-5.4,0.));
#16022=CARTESIAN_POINT('',(-4.,-5.4,-1.));
#16023=CARTESIAN_POINT('Origin',(-4.,5.4,-1.));
#16024=CARTESIAN_POINT('',(-4.,5.4,-1.));
#16025=CARTESIAN_POINT('',(-4.,5.4,0.));
#16026=CARTESIAN_POINT('Origin',(4.,0.,0.));
#16027=CARTESIAN_POINT('Origin',(4.,0.,-1.));
#16028=CARTESIAN_POINT('',(0.,0.,0.));
#16029=CARTESIAN_POINT('Origin',(6.,-4.5,7.6));
#16030=CARTESIAN_POINT('',(5.835,-4.4,7.6));
#16031=CARTESIAN_POINT('Origin',(6.,-4.4,7.6));
#16032=CARTESIAN_POINT('',(5.835,-2.6,7.6));
#16033=CARTESIAN_POINT('',(5.835,-4.5,7.6));
#16034=CARTESIAN_POINT('Origin',(6.,-2.6,7.6));
#16035=CARTESIAN_POINT('Origin',(3.74833395016046,-4.5,3.7));
#16036=CARTESIAN_POINT('',(3.58333395016046,-4.4,3.7));
#16037=CARTESIAN_POINT('Origin',(3.74833395016046,-4.4,3.7));
#16038=CARTESIAN_POINT('',(3.58333395016046,-2.6,3.7));
#16039=CARTESIAN_POINT('',(3.58333395016046,-4.5,3.7));
#16040=CARTESIAN_POINT('Origin',(3.74833395016046,-2.6,3.7));
#16041=CARTESIAN_POINT('Origin',(8.25166604983954,-4.5,3.7));
#16042=CARTESIAN_POINT('',(8.08666604983954,-4.4,3.7));
#16043=CARTESIAN_POINT('Origin',(8.25166604983954,-4.4,3.7));
#16044=CARTESIAN_POINT('',(8.08666604983954,-2.6,3.7));
#16045=CARTESIAN_POINT('',(8.08666604983954,-4.5,3.7));
#16046=CARTESIAN_POINT('Origin',(8.25166604983954,-2.6,3.7));
#16047=CARTESIAN_POINT('Origin',(1.16341445918999E-16,-4.5,6.9));
#16048=CARTESIAN_POINT('',(-0.165,-4.4,6.9));
#16049=CARTESIAN_POINT('Origin',(1.16341445918999E-16,-4.4,6.9));
#16050=CARTESIAN_POINT('',(-0.165,-2.6,6.9));
#16051=CARTESIAN_POINT('',(-0.165,-4.5,6.9));
#16052=CARTESIAN_POINT('Origin',(1.16341445918999E-16,-2.6,6.9));
#16053=CARTESIAN_POINT('Origin',(-1.64544826719043,-4.5,4.05));
#16054=CARTESIAN_POINT('',(-1.81044826719043,-4.4,4.05));
#16055=CARTESIAN_POINT('Origin',(-1.64544826719043,-4.4,4.05));
#16056=CARTESIAN_POINT('',(-1.81044826719043,-2.6,4.05));
#16057=CARTESIAN_POINT('',(-1.81044826719043,-4.5,4.05));
#16058=CARTESIAN_POINT('Origin',(-1.64544826719043,-2.6,4.05));
#16059=CARTESIAN_POINT('Origin',(1.64544826719043,-4.5,4.05));
#16060=CARTESIAN_POINT('',(1.48044826719043,-4.4,4.05));
#16061=CARTESIAN_POINT('Origin',(1.64544826719043,-4.4,4.05));
#16062=CARTESIAN_POINT('',(1.48044826719043,-2.6,4.05));
#16063=CARTESIAN_POINT('',(1.48044826719043,-4.5,4.05));
#16064=CARTESIAN_POINT('Origin',(1.64544826719043,-2.6,4.05));
#16065=CARTESIAN_POINT('Origin',(10.,-4.5,2.));
#16066=CARTESIAN_POINT('',(9.525,-4.4,2.));
#16067=CARTESIAN_POINT('Origin',(10.,-4.4,2.));
#16068=CARTESIAN_POINT('',(9.525,-3.9,2.));
#16069=CARTESIAN_POINT('',(9.525,-4.5,2.));
#16070=CARTESIAN_POINT('Origin',(10.,-3.9,2.));
#16071=CARTESIAN_POINT('Origin',(10.,-3.9,2.));
#16072=CARTESIAN_POINT('',(9.725,-3.9,2.));
#16073=CARTESIAN_POINT('Origin',(10.,-3.9,2.));
#16074=CARTESIAN_POINT('Origin',(-2.,-4.5,9.));
#16075=CARTESIAN_POINT('',(-2.475,-4.4,9.));
#16076=CARTESIAN_POINT('Origin',(-2.,-4.4,9.));
#16077=CARTESIAN_POINT('',(-2.475,-3.9,9.));
#16078=CARTESIAN_POINT('',(-2.475,-4.5,9.));
#16079=CARTESIAN_POINT('Origin',(-2.,-3.9,9.));
#16080=CARTESIAN_POINT('Origin',(-2.,-3.9,9.));
#16081=CARTESIAN_POINT('',(-2.275,-3.9,9.));
#16082=CARTESIAN_POINT('Origin',(-2.,-3.9,9.));
#16083=CARTESIAN_POINT('Origin',(-2.,-4.5,2.));
#16084=CARTESIAN_POINT('',(-2.475,-4.4,2.));
#16085=CARTESIAN_POINT('Origin',(-2.,-4.4,2.));
#16086=CARTESIAN_POINT('',(-2.475,-3.9,2.));
#16087=CARTESIAN_POINT('',(-2.475,-4.5,2.));
#16088=CARTESIAN_POINT('Origin',(-2.,-3.9,2.));
#16089=CARTESIAN_POINT('Origin',(-2.,-3.9,2.));
#16090=CARTESIAN_POINT('',(-2.275,-3.9,2.));
#16091=CARTESIAN_POINT('Origin',(-2.,-3.9,2.));
#16092=CARTESIAN_POINT('Origin',(10.,-4.5,9.));
#16093=CARTESIAN_POINT('',(9.525,-4.4,9.));
#16094=CARTESIAN_POINT('Origin',(10.,-4.4,9.));
#16095=CARTESIAN_POINT('',(9.525,-3.9,9.));
#16096=CARTESIAN_POINT('',(9.525,-4.5,9.));
#16097=CARTESIAN_POINT('Origin',(10.,-3.9,9.));
#16098=CARTESIAN_POINT('Origin',(10.,-3.9,9.));
#16099=CARTESIAN_POINT('',(9.725,-3.9,9.));
#16100=CARTESIAN_POINT('Origin',(10.,-3.9,9.));
#16101=CARTESIAN_POINT('Origin',(10.,-4.5,2.));
#16102=CARTESIAN_POINT('',(9.725,-2.6,2.));
#16103=CARTESIAN_POINT('',(9.725,-4.5,2.));
#16104=CARTESIAN_POINT('Origin',(10.,-2.6,2.));
#16105=CARTESIAN_POINT('Origin',(-2.,-4.5,9.));
#16106=CARTESIAN_POINT('',(-2.275,-2.6,9.));
#16107=CARTESIAN_POINT('',(-2.275,-4.5,9.));
#16108=CARTESIAN_POINT('Origin',(-2.,-2.6,9.));
#16109=CARTESIAN_POINT('Origin',(-2.,-4.5,2.));
#16110=CARTESIAN_POINT('',(-2.275,-2.6,2.));
#16111=CARTESIAN_POINT('',(-2.275,-4.5,2.));
#16112=CARTESIAN_POINT('Origin',(-2.,-2.6,2.));
#16113=CARTESIAN_POINT('Origin',(10.,-4.5,9.));
#16114=CARTESIAN_POINT('',(9.725,-2.6,9.));
#16115=CARTESIAN_POINT('',(9.725,-4.5,9.));
#16116=CARTESIAN_POINT('Origin',(10.,-2.6,9.));
#16117=CARTESIAN_POINT('Origin',(10.,-3.5,-0.1));
#16118=CARTESIAN_POINT('',(9.75,-3.5,0.));
#16119=CARTESIAN_POINT('Origin',(10.,-3.5,0.));
#16120=CARTESIAN_POINT('',(9.75,-3.5,1.7));
#16121=CARTESIAN_POINT('',(9.75,-3.5,-0.1));
#16122=CARTESIAN_POINT('Origin',(10.,-3.5,1.7));
#16123=CARTESIAN_POINT('Origin',(10.,-3.5,1.7));
#16124=CARTESIAN_POINT('Origin',(-2.,-3.5,-0.1));
#16125=CARTESIAN_POINT('',(-2.25,-3.5,0.));
#16126=CARTESIAN_POINT('Origin',(-2.,-3.5,0.));
#16127=CARTESIAN_POINT('',(-2.25,-3.5,1.7));
#16128=CARTESIAN_POINT('',(-2.25,-3.5,-0.1));
#16129=CARTESIAN_POINT('Origin',(-2.,-3.5,1.7));
#16130=CARTESIAN_POINT('Origin',(-2.,-3.5,1.7));
#16131=CARTESIAN_POINT('Origin',(6.,-4.5,5.));
#16132=CARTESIAN_POINT('',(3.65,-4.4,5.));
#16133=CARTESIAN_POINT('Origin',(6.,-4.4,5.));
#16134=CARTESIAN_POINT('',(3.65,-2.8,5.));
#16135=CARTESIAN_POINT('',(3.65,-4.5,5.));
#16136=CARTESIAN_POINT('Origin',(6.,-2.8,5.));
#16137=CARTESIAN_POINT('Origin',(6.,-2.8,5.));
#16138=CARTESIAN_POINT('',(3.85,-2.8,5.));
#16139=CARTESIAN_POINT('Origin',(6.,-2.8,5.));
#16140=CARTESIAN_POINT('Origin',(6.,-4.5,5.));
#16141=CARTESIAN_POINT('',(3.85,-2.6,5.));
#16142=CARTESIAN_POINT('',(3.85,-4.5,5.));
#16143=CARTESIAN_POINT('Origin',(6.,-2.6,5.));
#16144=CARTESIAN_POINT('Origin',(0.,-4.5,5.));
#16145=CARTESIAN_POINT('',(-1.6,-4.4,5.));
#16146=CARTESIAN_POINT('Origin',(0.,-4.4,5.));
#16147=CARTESIAN_POINT('',(-1.6,-3.,5.));
#16148=CARTESIAN_POINT('',(-1.6,-4.5,5.));
#16149=CARTESIAN_POINT('Origin',(0.,-3.,5.));
#16150=CARTESIAN_POINT('Origin',(0.,-3.,5.));
#16151=CARTESIAN_POINT('',(-1.4,-3.,5.));
#16152=CARTESIAN_POINT('Origin',(0.,-3.,5.));
#16153=CARTESIAN_POINT('Origin',(0.,-4.5,5.));
#16154=CARTESIAN_POINT('',(-1.4,-2.6,5.));
#16155=CARTESIAN_POINT('',(-1.4,-4.5,5.));
#16156=CARTESIAN_POINT('Origin',(0.,-2.6,5.));
#16157=CARTESIAN_POINT('Origin',(11.,-2.6,0.));
#16158=CARTESIAN_POINT('',(11.,-2.6,0.));
#16159=CARTESIAN_POINT('',(-3.,-2.6,0.));
#16160=CARTESIAN_POINT('',(11.,-2.6,0.));
#16161=CARTESIAN_POINT('',(-3.,-2.6,10.));
#16162=CARTESIAN_POINT('',(-3.,-2.6,0.));
#16163=CARTESIAN_POINT('',(11.,-2.6,10.));
#16164=CARTESIAN_POINT('',(11.,-2.6,10.));
#16165=CARTESIAN_POINT('',(11.,-2.6,0.));
#16166=CARTESIAN_POINT('Origin',(11.,-4.4,0.));
#16167=CARTESIAN_POINT('',(11.,-4.4,0.));
#16168=CARTESIAN_POINT('',(11.,-4.4,0.));
#16169=CARTESIAN_POINT('',(11.,-4.4,10.));
#16170=CARTESIAN_POINT('',(11.,-4.4,10.));
#16171=CARTESIAN_POINT('',(11.,-4.4,0.));
#16172=CARTESIAN_POINT('Origin',(-3.,-4.4,0.));
#16173=CARTESIAN_POINT('',(-3.,-4.4,0.));
#16174=CARTESIAN_POINT('',(-3.,-4.4,0.));
#16175=CARTESIAN_POINT('',(-3.,-4.4,10.));
#16176=CARTESIAN_POINT('',(-3.,-4.4,10.));
#16177=CARTESIAN_POINT('',(-3.,-4.4,0.));
#16178=CARTESIAN_POINT('Origin',(-3.,-2.6,0.));
#16179=CARTESIAN_POINT('',(-3.,-2.6,0.));
#16180=CARTESIAN_POINT('',(-3.,-2.6,10.));
#16181=CARTESIAN_POINT('Origin',(4.,-3.5,10.));
#16182=CARTESIAN_POINT('Origin',(4.,-3.5,0.));
#16183=CARTESIAN_POINT('',(0.,0.,0.));
#16184=CARTESIAN_POINT('Origin',(6.,2.5,7.6));
#16185=CARTESIAN_POINT('',(5.835,2.6,7.6));
#16186=CARTESIAN_POINT('Origin',(6.,2.6,7.6));
#16187=CARTESIAN_POINT('',(5.835,4.4,7.6));
#16188=CARTESIAN_POINT('',(5.835,2.5,7.6));
#16189=CARTESIAN_POINT('Origin',(6.,4.4,7.6));
#16190=CARTESIAN_POINT('Origin',(3.74833395016046,2.5,3.7));
#16191=CARTESIAN_POINT('',(3.58333395016046,2.6,3.7));
#16192=CARTESIAN_POINT('Origin',(3.74833395016046,2.6,3.7));
#16193=CARTESIAN_POINT('',(3.58333395016046,4.4,3.7));
#16194=CARTESIAN_POINT('',(3.58333395016046,2.5,3.7));
#16195=CARTESIAN_POINT('Origin',(3.74833395016046,4.4,3.7));
#16196=CARTESIAN_POINT('Origin',(8.25166604983954,2.5,3.7));
#16197=CARTESIAN_POINT('',(8.08666604983954,2.6,3.7));
#16198=CARTESIAN_POINT('Origin',(8.25166604983954,2.6,3.7));
#16199=CARTESIAN_POINT('',(8.08666604983954,4.4,3.7));
#16200=CARTESIAN_POINT('',(8.08666604983954,2.5,3.7));
#16201=CARTESIAN_POINT('Origin',(8.25166604983954,4.4,3.7));
#16202=CARTESIAN_POINT('Origin',(1.16341445918999E-16,2.5,6.9));
#16203=CARTESIAN_POINT('',(-0.165,2.6,6.9));
#16204=CARTESIAN_POINT('Origin',(1.16341445918999E-16,2.6,6.9));
#16205=CARTESIAN_POINT('',(-0.165,4.4,6.9));
#16206=CARTESIAN_POINT('',(-0.165,2.5,6.9));
#16207=CARTESIAN_POINT('Origin',(1.16341445918999E-16,4.4,6.9));
#16208=CARTESIAN_POINT('Origin',(-1.64544826719043,2.5,4.05));
#16209=CARTESIAN_POINT('',(-1.81044826719043,2.6,4.05));
#16210=CARTESIAN_POINT('Origin',(-1.64544826719043,2.6,4.05));
#16211=CARTESIAN_POINT('',(-1.81044826719043,4.4,4.05));
#16212=CARTESIAN_POINT('',(-1.81044826719043,2.5,4.05));
#16213=CARTESIAN_POINT('Origin',(-1.64544826719043,4.4,4.05));
#16214=CARTESIAN_POINT('Origin',(1.64544826719043,2.5,4.05));
#16215=CARTESIAN_POINT('',(1.48044826719043,2.6,4.05));
#16216=CARTESIAN_POINT('Origin',(1.64544826719043,2.6,4.05));
#16217=CARTESIAN_POINT('',(1.48044826719043,4.4,4.05));
#16218=CARTESIAN_POINT('',(1.48044826719043,2.5,4.05));
#16219=CARTESIAN_POINT('Origin',(1.64544826719043,4.4,4.05));
#16220=CARTESIAN_POINT('Origin',(10.,3.9,2.));
#16221=CARTESIAN_POINT('',(9.525,3.9,2.));
#16222=CARTESIAN_POINT('Origin',(10.,3.9,2.));
#16223=CARTESIAN_POINT('',(9.525,4.4,2.));
#16224=CARTESIAN_POINT('',(9.525,3.9,2.));
#16225=CARTESIAN_POINT('Origin',(10.,4.4,2.));
#16226=CARTESIAN_POINT('Origin',(10.,3.9,2.));
#16227=CARTESIAN_POINT('',(9.725,3.9,2.));
#16228=CARTESIAN_POINT('Origin',(10.,3.9,2.));
#16229=CARTESIAN_POINT('Origin',(-2.,3.9,9.));
#16230=CARTESIAN_POINT('',(-2.475,3.9,9.));
#16231=CARTESIAN_POINT('Origin',(-2.,3.9,9.));
#16232=CARTESIAN_POINT('',(-2.475,4.4,9.));
#16233=CARTESIAN_POINT('',(-2.475,3.9,9.));
#16234=CARTESIAN_POINT('Origin',(-2.,4.4,9.));
#16235=CARTESIAN_POINT('Origin',(-2.,3.9,9.));
#16236=CARTESIAN_POINT('',(-2.275,3.9,9.));
#16237=CARTESIAN_POINT('Origin',(-2.,3.9,9.));
#16238=CARTESIAN_POINT('Origin',(-2.,3.9,2.));
#16239=CARTESIAN_POINT('',(-2.475,3.9,2.));
#16240=CARTESIAN_POINT('Origin',(-2.,3.9,2.));
#16241=CARTESIAN_POINT('',(-2.475,4.4,2.));
#16242=CARTESIAN_POINT('',(-2.475,3.9,2.));
#16243=CARTESIAN_POINT('Origin',(-2.,4.4,2.));
#16244=CARTESIAN_POINT('Origin',(-2.,3.9,2.));
#16245=CARTESIAN_POINT('',(-2.275,3.9,2.));
#16246=CARTESIAN_POINT('Origin',(-2.,3.9,2.));
#16247=CARTESIAN_POINT('Origin',(10.,3.9,9.));
#16248=CARTESIAN_POINT('',(9.525,3.9,9.));
#16249=CARTESIAN_POINT('Origin',(10.,3.9,9.));
#16250=CARTESIAN_POINT('',(9.525,4.4,9.));
#16251=CARTESIAN_POINT('',(9.525,3.9,9.));
#16252=CARTESIAN_POINT('Origin',(10.,4.4,9.));
#16253=CARTESIAN_POINT('Origin',(10.,3.9,9.));
#16254=CARTESIAN_POINT('',(9.725,3.9,9.));
#16255=CARTESIAN_POINT('Origin',(10.,3.9,9.));
#16256=CARTESIAN_POINT('Origin',(10.,2.5,2.));
#16257=CARTESIAN_POINT('',(9.725,2.6,2.));
#16258=CARTESIAN_POINT('Origin',(10.,2.6,2.));
#16259=CARTESIAN_POINT('',(9.725,2.5,2.));
#16260=CARTESIAN_POINT('Origin',(-2.,2.5,9.));
#16261=CARTESIAN_POINT('',(-2.275,2.6,9.));
#16262=CARTESIAN_POINT('Origin',(-2.,2.6,9.));
#16263=CARTESIAN_POINT('',(-2.275,2.5,9.));
#16264=CARTESIAN_POINT('Origin',(-2.,2.5,2.));
#16265=CARTESIAN_POINT('',(-2.275,2.6,2.));
#16266=CARTESIAN_POINT('Origin',(-2.,2.6,2.));
#16267=CARTESIAN_POINT('',(-2.275,2.5,2.));
#16268=CARTESIAN_POINT('Origin',(10.,2.5,9.));
#16269=CARTESIAN_POINT('',(9.725,2.6,9.));
#16270=CARTESIAN_POINT('Origin',(10.,2.6,9.));
#16271=CARTESIAN_POINT('',(9.725,2.5,9.));
#16272=CARTESIAN_POINT('Origin',(10.,3.5,-0.1));
#16273=CARTESIAN_POINT('',(9.75,3.5,0.));
#16274=CARTESIAN_POINT('Origin',(10.,3.5,0.));
#16275=CARTESIAN_POINT('',(9.75,3.5,1.7));
#16276=CARTESIAN_POINT('',(9.75,3.5,-0.1));
#16277=CARTESIAN_POINT('Origin',(10.,3.5,1.7));
#16278=CARTESIAN_POINT('Origin',(10.,3.5,1.7));
#16279=CARTESIAN_POINT('Origin',(-2.,3.5,-0.1));
#16280=CARTESIAN_POINT('',(-2.25,3.5,0.));
#16281=CARTESIAN_POINT('Origin',(-2.,3.5,0.));
#16282=CARTESIAN_POINT('',(-2.25,3.5,1.7));
#16283=CARTESIAN_POINT('',(-2.25,3.5,-0.1));
#16284=CARTESIAN_POINT('Origin',(-2.,3.5,1.7));
#16285=CARTESIAN_POINT('Origin',(-2.,3.5,1.7));
#16286=CARTESIAN_POINT('Origin',(6.,2.8,5.));
#16287=CARTESIAN_POINT('',(3.65,2.8,5.));
#16288=CARTESIAN_POINT('Origin',(6.,2.8,5.));
#16289=CARTESIAN_POINT('',(3.65,4.4,5.));
#16290=CARTESIAN_POINT('',(3.65,2.8,5.));
#16291=CARTESIAN_POINT('Origin',(6.,4.4,5.));
#16292=CARTESIAN_POINT('Origin',(6.,2.8,5.));
#16293=CARTESIAN_POINT('',(3.85,2.8,5.));
#16294=CARTESIAN_POINT('Origin',(6.,2.8,5.));
#16295=CARTESIAN_POINT('Origin',(6.,2.5,5.));
#16296=CARTESIAN_POINT('',(3.85,2.6,5.));
#16297=CARTESIAN_POINT('Origin',(6.,2.6,5.));
#16298=CARTESIAN_POINT('',(3.85,2.5,5.));
#16299=CARTESIAN_POINT('Origin',(0.,3.,5.));
#16300=CARTESIAN_POINT('',(-1.6,3.,5.));
#16301=CARTESIAN_POINT('Origin',(0.,3.,5.));
#16302=CARTESIAN_POINT('',(-1.6,4.4,5.));
#16303=CARTESIAN_POINT('',(-1.6,3.,5.));
#16304=CARTESIAN_POINT('Origin',(0.,4.4,5.));
#16305=CARTESIAN_POINT('Origin',(0.,3.,5.));
#16306=CARTESIAN_POINT('',(-1.4,3.,5.));
#16307=CARTESIAN_POINT('Origin',(0.,3.,5.));
#16308=CARTESIAN_POINT('Origin',(0.,2.5,5.));
#16309=CARTESIAN_POINT('',(-1.4,2.6,5.));
#16310=CARTESIAN_POINT('Origin',(0.,2.6,5.));
#16311=CARTESIAN_POINT('',(-1.4,2.5,5.));
#16312=CARTESIAN_POINT('Origin',(11.,4.4,0.));
#16313=CARTESIAN_POINT('',(11.,4.4,0.));
#16314=CARTESIAN_POINT('',(-3.,4.4,0.));
#16315=CARTESIAN_POINT('',(11.,4.4,0.));
#16316=CARTESIAN_POINT('',(-3.,4.4,10.));
#16317=CARTESIAN_POINT('',(-3.,4.4,0.));
#16318=CARTESIAN_POINT('',(11.,4.4,10.));
#16319=CARTESIAN_POINT('',(11.,4.4,10.));
#16320=CARTESIAN_POINT('',(11.,4.4,0.));
#16321=CARTESIAN_POINT('Origin',(11.,2.6,0.));
#16322=CARTESIAN_POINT('',(11.,2.6,0.));
#16323=CARTESIAN_POINT('',(11.,2.6,0.));
#16324=CARTESIAN_POINT('',(11.,2.6,10.));
#16325=CARTESIAN_POINT('',(11.,2.6,10.));
#16326=CARTESIAN_POINT('',(11.,2.6,0.));
#16327=CARTESIAN_POINT('Origin',(-3.,2.6,0.));
#16328=CARTESIAN_POINT('',(-3.,2.6,0.));
#16329=CARTESIAN_POINT('',(-3.,2.6,0.));
#16330=CARTESIAN_POINT('',(-3.,2.6,10.));
#16331=CARTESIAN_POINT('',(-3.,2.6,10.));
#16332=CARTESIAN_POINT('',(-3.,2.6,0.));
#16333=CARTESIAN_POINT('Origin',(-3.,4.4,0.));
#16334=CARTESIAN_POINT('',(-3.,4.4,0.));
#16335=CARTESIAN_POINT('',(-3.,4.4,10.));
#16336=CARTESIAN_POINT('Origin',(4.,3.5,10.));
#16337=CARTESIAN_POINT('Origin',(4.,3.5,0.));
#16338=CARTESIAN_POINT('',(0.,0.,0.));
#16339=CARTESIAN_POINT('Origin',(-2.,-2.6,2.));
#16340=CARTESIAN_POINT('',(-2.21,2.6,2.));
#16341=CARTESIAN_POINT('Origin',(-2.,2.6,2.));
#16342=CARTESIAN_POINT('',(-2.21,-2.6,2.));
#16343=CARTESIAN_POINT('',(-2.21,-2.6,2.));
#16344=CARTESIAN_POINT('Origin',(-2.,-2.6,2.));
#16345=CARTESIAN_POINT('Origin',(-2.,-2.6,2.));
#16346=CARTESIAN_POINT('',(-2.5,2.6,2.));
#16347=CARTESIAN_POINT('Origin',(-2.,2.6,2.));
#16348=CARTESIAN_POINT('',(-2.5,-2.6,2.));
#16349=CARTESIAN_POINT('',(-2.5,-2.6,2.));
#16350=CARTESIAN_POINT('Origin',(-2.,-2.6,2.));
#16351=CARTESIAN_POINT('Origin',(-2.,2.6,2.));
#16352=CARTESIAN_POINT('Origin',(-2.,-2.6,2.));
#16353=CARTESIAN_POINT('',(0.,0.,0.));
#16354=CARTESIAN_POINT('Origin',(-2.,-2.6,9.));
#16355=CARTESIAN_POINT('',(-2.21,2.6,9.));
#16356=CARTESIAN_POINT('Origin',(-2.,2.6,9.));
#16357=CARTESIAN_POINT('',(-2.21,-2.6,9.));
#16358=CARTESIAN_POINT('',(-2.21,-2.6,9.));
#16359=CARTESIAN_POINT('Origin',(-2.,-2.6,9.));
#16360=CARTESIAN_POINT('Origin',(-2.,-2.6,9.));
#16361=CARTESIAN_POINT('',(-2.5,2.6,9.));
#16362=CARTESIAN_POINT('Origin',(-2.,2.6,9.));
#16363=CARTESIAN_POINT('',(-2.5,-2.6,9.));
#16364=CARTESIAN_POINT('',(-2.5,-2.6,9.));
#16365=CARTESIAN_POINT('Origin',(-2.,-2.6,9.));
#16366=CARTESIAN_POINT('Origin',(-2.,2.6,9.));
#16367=CARTESIAN_POINT('Origin',(-2.,-2.6,9.));
#16368=CARTESIAN_POINT('',(0.,0.,0.));
#16369=CARTESIAN_POINT('Origin',(10.,-2.6,2.));
#16370=CARTESIAN_POINT('',(9.79,2.6,2.));
#16371=CARTESIAN_POINT('Origin',(10.,2.6,2.));
#16372=CARTESIAN_POINT('',(9.79,-2.6,2.));
#16373=CARTESIAN_POINT('',(9.79,-2.6,2.));
#16374=CARTESIAN_POINT('Origin',(10.,-2.6,2.));
#16375=CARTESIAN_POINT('Origin',(10.,-2.6,2.));
#16376=CARTESIAN_POINT('',(9.5,2.6,2.));
#16377=CARTESIAN_POINT('Origin',(10.,2.6,2.));
#16378=CARTESIAN_POINT('',(9.5,-2.6,2.));
#16379=CARTESIAN_POINT('',(9.5,-2.6,2.));
#16380=CARTESIAN_POINT('Origin',(10.,-2.6,2.));
#16381=CARTESIAN_POINT('Origin',(10.,2.6,2.));
#16382=CARTESIAN_POINT('Origin',(10.,-2.6,2.));
#16383=CARTESIAN_POINT('',(0.,0.,0.));
#16384=CARTESIAN_POINT('Origin',(10.,-2.6,9.));
#16385=CARTESIAN_POINT('',(9.79,2.6,9.));
#16386=CARTESIAN_POINT('Origin',(10.,2.6,9.));
#16387=CARTESIAN_POINT('',(9.79,-2.6,9.));
#16388=CARTESIAN_POINT('',(9.79,-2.6,9.));
#16389=CARTESIAN_POINT('Origin',(10.,-2.6,9.));
#16390=CARTESIAN_POINT('Origin',(10.,-2.6,9.));
#16391=CARTESIAN_POINT('',(9.5,2.6,9.));
#16392=CARTESIAN_POINT('Origin',(10.,2.6,9.));
#16393=CARTESIAN_POINT('',(9.5,-2.6,9.));
#16394=CARTESIAN_POINT('',(9.5,-2.6,9.));
#16395=CARTESIAN_POINT('Origin',(10.,-2.6,9.));
#16396=CARTESIAN_POINT('Origin',(10.,2.6,9.));
#16397=CARTESIAN_POINT('Origin',(10.,-2.6,9.));
#16398=CARTESIAN_POINT('',(0.,0.,0.));
#16399=CARTESIAN_POINT('Origin',(1.16341445918999E-16,-4.8,6.9));
#16400=CARTESIAN_POINT('',(-0.225,-4.7,6.9));
#16401=CARTESIAN_POINT('Origin',(1.16341445918999E-16,-4.7,6.9));
#16402=CARTESIAN_POINT('',(-0.225,-4.4,6.9));
#16403=CARTESIAN_POINT('',(-0.225,-4.8,6.9));
#16404=CARTESIAN_POINT('Origin',(1.16341445918999E-16,-4.4,6.9));
#16405=CARTESIAN_POINT('Origin',(-1.64544826719043,-4.8,4.05));
#16406=CARTESIAN_POINT('',(-1.87044826719043,-4.7,4.05));
#16407=CARTESIAN_POINT('Origin',(-1.64544826719043,-4.7,4.05));
#16408=CARTESIAN_POINT('',(-1.87044826719043,-4.4,4.05));
#16409=CARTESIAN_POINT('',(-1.87044826719043,-4.8,4.05));
#16410=CARTESIAN_POINT('Origin',(-1.64544826719043,-4.4,4.05));
#16411=CARTESIAN_POINT('Origin',(1.64544826719043,-4.8,4.05));
#16412=CARTESIAN_POINT('',(1.42044826719043,-4.7,4.05));
#16413=CARTESIAN_POINT('Origin',(1.64544826719043,-4.7,4.05));
#16414=CARTESIAN_POINT('',(1.42044826719043,-4.4,4.05));
#16415=CARTESIAN_POINT('',(1.42044826719043,-4.8,4.05));
#16416=CARTESIAN_POINT('Origin',(1.64544826719043,-4.4,4.05));
#16417=CARTESIAN_POINT('Origin',(0.,-4.4,5.));
#16418=CARTESIAN_POINT('',(-1.59,-4.,5.));
#16419=CARTESIAN_POINT('Origin',(0.,-4.,5.));
#16420=CARTESIAN_POINT('',(-1.59,-4.4,5.));
#16421=CARTESIAN_POINT('',(-1.59,-4.4,5.));
#16422=CARTESIAN_POINT('Origin',(0.,-4.4,5.));
#16423=CARTESIAN_POINT('Origin',(0.,-4.,5.));
#16424=CARTESIAN_POINT('',(-1.2,-4.,5.));
#16425=CARTESIAN_POINT('Origin',(0.,-4.,5.));
#16426=CARTESIAN_POINT('Origin',(0.,-4.7,5.));
#16427=CARTESIAN_POINT('',(-1.2,-4.7,5.));
#16428=CARTESIAN_POINT('',(-1.2,-4.7,5.));
#16429=CARTESIAN_POINT('Origin',(0.,-4.7,5.));
#16430=CARTESIAN_POINT('Origin',(0.,-4.7,5.));
#16431=CARTESIAN_POINT('',(-2.2,-4.4,5.));
#16432=CARTESIAN_POINT('Origin',(0.,-4.4,5.));
#16433=CARTESIAN_POINT('',(-2.2,-4.7,5.));
#16434=CARTESIAN_POINT('',(-2.2,-4.7,5.));
#16435=CARTESIAN_POINT('Origin',(0.,-4.7,5.));
#16436=CARTESIAN_POINT('Origin',(0.,-4.4,5.));
#16437=CARTESIAN_POINT('Origin',(0.,-4.7,5.));
#16438=CARTESIAN_POINT('',(0.,0.,0.));
#16439=CARTESIAN_POINT('Origin',(6.,-4.8,7.6));
#16440=CARTESIAN_POINT('',(5.775,-4.7,7.6));
#16441=CARTESIAN_POINT('Origin',(6.,-4.7,7.6));
#16442=CARTESIAN_POINT('',(5.775,-4.4,7.6));
#16443=CARTESIAN_POINT('',(5.775,-4.8,7.6));
#16444=CARTESIAN_POINT('Origin',(6.,-4.4,7.6));
#16445=CARTESIAN_POINT('Origin',(3.74833395016046,-4.8,3.7));
#16446=CARTESIAN_POINT('',(3.52333395016046,-4.7,3.7));
#16447=CARTESIAN_POINT('Origin',(3.74833395016046,-4.7,3.7));
#16448=CARTESIAN_POINT('',(3.52333395016046,-4.4,3.7));
#16449=CARTESIAN_POINT('',(3.52333395016046,-4.8,3.7));
#16450=CARTESIAN_POINT('Origin',(3.74833395016046,-4.4,3.7));
#16451=CARTESIAN_POINT('Origin',(8.25166604983954,-4.8,3.7));
#16452=CARTESIAN_POINT('',(8.02666604983954,-4.7,3.7));
#16453=CARTESIAN_POINT('Origin',(8.25166604983954,-4.7,3.7));
#16454=CARTESIAN_POINT('',(8.02666604983954,-4.4,3.7));
#16455=CARTESIAN_POINT('',(8.02666604983954,-4.8,3.7));
#16456=CARTESIAN_POINT('Origin',(8.25166604983954,-4.4,3.7));
#16457=CARTESIAN_POINT('Origin',(6.,-4.4,5.));
#16458=CARTESIAN_POINT('',(3.66,-4.2,5.));
#16459=CARTESIAN_POINT('Origin',(6.,-4.2,5.));
#16460=CARTESIAN_POINT('',(3.66,-4.4,5.));
#16461=CARTESIAN_POINT('',(3.66,-4.4,5.));
#16462=CARTESIAN_POINT('Origin',(6.,-4.4,5.));
#16463=CARTESIAN_POINT('Origin',(6.,-4.2,5.));
#16464=CARTESIAN_POINT('',(4.2,-4.2,5.));
#16465=CARTESIAN_POINT('Origin',(6.,-4.2,5.));
#16466=CARTESIAN_POINT('Origin',(6.,-4.7,5.));
#16467=CARTESIAN_POINT('',(4.2,-4.7,5.));
#16468=CARTESIAN_POINT('',(4.2,-4.7,5.));
#16469=CARTESIAN_POINT('Origin',(6.,-4.7,5.));
#16470=CARTESIAN_POINT('Origin',(6.,-4.7,5.));
#16471=CARTESIAN_POINT('',(3.,-4.4,5.));
#16472=CARTESIAN_POINT('Origin',(6.,-4.4,5.));
#16473=CARTESIAN_POINT('',(3.,-4.7,5.));
#16474=CARTESIAN_POINT('',(3.,-4.7,5.));
#16475=CARTESIAN_POINT('Origin',(6.,-4.7,5.));
#16476=CARTESIAN_POINT('Origin',(6.,-4.4,5.));
#16477=CARTESIAN_POINT('Origin',(6.,-4.7,5.));
#16478=CARTESIAN_POINT('',(0.,0.,0.));
#16479=CARTESIAN_POINT('Origin',(1.16341445918999E-16,4.3,6.9));
#16480=CARTESIAN_POINT('',(-0.225,4.4,6.9));
#16481=CARTESIAN_POINT('Origin',(1.16341445918999E-16,4.4,6.9));
#16482=CARTESIAN_POINT('',(-0.225,4.7,6.9));
#16483=CARTESIAN_POINT('',(-0.225,4.3,6.9));
#16484=CARTESIAN_POINT('Origin',(1.16341445918999E-16,4.7,6.9));
#16485=CARTESIAN_POINT('Origin',(-1.64544826719043,4.3,4.05));
#16486=CARTESIAN_POINT('',(-1.87044826719043,4.4,4.05));
#16487=CARTESIAN_POINT('Origin',(-1.64544826719043,4.4,4.05));
#16488=CARTESIAN_POINT('',(-1.87044826719043,4.7,4.05));
#16489=CARTESIAN_POINT('',(-1.87044826719043,4.3,4.05));
#16490=CARTESIAN_POINT('Origin',(-1.64544826719043,4.7,4.05));
#16491=CARTESIAN_POINT('Origin',(1.64544826719043,4.3,4.05));
#16492=CARTESIAN_POINT('',(1.42044826719043,4.4,4.05));
#16493=CARTESIAN_POINT('Origin',(1.64544826719043,4.4,4.05));
#16494=CARTESIAN_POINT('',(1.42044826719043,4.7,4.05));
#16495=CARTESIAN_POINT('',(1.42044826719043,4.3,4.05));
#16496=CARTESIAN_POINT('Origin',(1.64544826719043,4.7,4.05));
#16497=CARTESIAN_POINT('Origin',(0.,4.,5.));
#16498=CARTESIAN_POINT('',(-1.59,4.4,5.));
#16499=CARTESIAN_POINT('Origin',(0.,4.4,5.));
#16500=CARTESIAN_POINT('',(-1.59,4.,5.));
#16501=CARTESIAN_POINT('',(-1.59,4.,5.));
#16502=CARTESIAN_POINT('Origin',(0.,4.,5.));
#16503=CARTESIAN_POINT('Origin',(0.,4.,5.));
#16504=CARTESIAN_POINT('',(-1.2,4.,5.));
#16505=CARTESIAN_POINT('Origin',(0.,4.,5.));
#16506=CARTESIAN_POINT('Origin',(0.,4.4,5.));
#16507=CARTESIAN_POINT('',(-1.2,4.7,5.));
#16508=CARTESIAN_POINT('Origin',(0.,4.7,5.));
#16509=CARTESIAN_POINT('',(-1.2,4.4,5.));
#16510=CARTESIAN_POINT('Origin',(0.,4.4,5.));
#16511=CARTESIAN_POINT('',(-2.2,4.7,5.));
#16512=CARTESIAN_POINT('Origin',(0.,4.7,5.));
#16513=CARTESIAN_POINT('',(-2.2,4.4,5.));
#16514=CARTESIAN_POINT('',(-2.2,4.4,5.));
#16515=CARTESIAN_POINT('Origin',(0.,4.4,5.));
#16516=CARTESIAN_POINT('Origin',(0.,4.7,5.));
#16517=CARTESIAN_POINT('Origin',(0.,4.4,5.));
#16518=CARTESIAN_POINT('',(0.,0.,0.));
#16519=CARTESIAN_POINT('Origin',(6.,4.3,7.6));
#16520=CARTESIAN_POINT('',(5.775,4.4,7.6));
#16521=CARTESIAN_POINT('Origin',(6.,4.4,7.6));
#16522=CARTESIAN_POINT('',(5.775,4.7,7.6));
#16523=CARTESIAN_POINT('',(5.775,4.3,7.6));
#16524=CARTESIAN_POINT('Origin',(6.,4.7,7.6));
#16525=CARTESIAN_POINT('Origin',(3.74833395016046,4.3,3.7));
#16526=CARTESIAN_POINT('',(3.52333395016046,4.4,3.7));
#16527=CARTESIAN_POINT('Origin',(3.74833395016046,4.4,3.7));
#16528=CARTESIAN_POINT('',(3.52333395016046,4.7,3.7));
#16529=CARTESIAN_POINT('',(3.52333395016046,4.3,3.7));
#16530=CARTESIAN_POINT('Origin',(3.74833395016046,4.7,3.7));
#16531=CARTESIAN_POINT('Origin',(8.25166604983954,4.3,3.7));
#16532=CARTESIAN_POINT('',(8.02666604983954,4.4,3.7));
#16533=CARTESIAN_POINT('Origin',(8.25166604983954,4.4,3.7));
#16534=CARTESIAN_POINT('',(8.02666604983954,4.7,3.7));
#16535=CARTESIAN_POINT('',(8.02666604983954,4.3,3.7));
#16536=CARTESIAN_POINT('Origin',(8.25166604983954,4.7,3.7));
#16537=CARTESIAN_POINT('Origin',(6.,4.2,5.));
#16538=CARTESIAN_POINT('',(3.66,4.4,5.));
#16539=CARTESIAN_POINT('Origin',(6.,4.4,5.));
#16540=CARTESIAN_POINT('',(3.66,4.2,5.));
#16541=CARTESIAN_POINT('',(3.66,4.2,5.));
#16542=CARTESIAN_POINT('Origin',(6.,4.2,5.));
#16543=CARTESIAN_POINT('Origin',(6.,4.2,5.));
#16544=CARTESIAN_POINT('',(4.2,4.2,5.));
#16545=CARTESIAN_POINT('Origin',(6.,4.2,5.));
#16546=CARTESIAN_POINT('Origin',(6.,4.4,5.));
#16547=CARTESIAN_POINT('',(4.2,4.7,5.));
#16548=CARTESIAN_POINT('Origin',(6.,4.7,5.));
#16549=CARTESIAN_POINT('',(4.2,4.4,5.));
#16550=CARTESIAN_POINT('Origin',(6.,4.4,5.));
#16551=CARTESIAN_POINT('',(3.,4.7,5.));
#16552=CARTESIAN_POINT('Origin',(6.,4.7,5.));
#16553=CARTESIAN_POINT('',(3.,4.4,5.));
#16554=CARTESIAN_POINT('',(3.,4.4,5.));
#16555=CARTESIAN_POINT('Origin',(6.,4.4,5.));
#16556=CARTESIAN_POINT('Origin',(6.,4.7,5.));
#16557=CARTESIAN_POINT('Origin',(6.,4.4,5.));
#16558=CARTESIAN_POINT('',(0.,0.,0.));
#16559=CARTESIAN_POINT('Origin',(0.375,0.5,0.));
#16560=CARTESIAN_POINT('',(-0.375,0.5,-4.59242549680257E-17));
#16561=CARTESIAN_POINT('Origin',(0.,0.5,0.));
#16562=CARTESIAN_POINT('Origin',(0.,0.475,0.));
#16563=CARTESIAN_POINT('',(-0.425,0.45,-5.20474889637625E-17));
#16564=CARTESIAN_POINT('Origin',(0.,0.45,0.));
#16565=CARTESIAN_POINT('',(-0.4,0.475,-4.89858719658941E-17));
#16566=CARTESIAN_POINT('Origin',(0.,0.24,0.));
#16567=CARTESIAN_POINT('',(-0.425,0.0299999999999998,-5.20474889637625E-17));
#16568=CARTESIAN_POINT('Origin',(0.,0.0299999999999998,0.));
#16569=CARTESIAN_POINT('',(-0.425,0.24,-5.20474889637625E-17));
#16570=CARTESIAN_POINT('Origin',(0.,0.0150000000000001,0.));
#16571=CARTESIAN_POINT('',(-0.395,4.85722573273506E-17,-4.83735485663204E-17));
#16572=CARTESIAN_POINT('Origin',(0.,0.,0.));
#16573=CARTESIAN_POINT('',(-0.41,0.0150000000000001,-5.02105187650415E-17));
#16574=CARTESIAN_POINT('Origin',(0.27,0.,0.));
#16575=CARTESIAN_POINT('',(-0.27,0.,-3.30654635769785E-17));
#16576=CARTESIAN_POINT('Origin',(0.,0.,0.));
#16577=CARTESIAN_POINT('Origin',(0.,-0.02,0.));
#16578=CARTESIAN_POINT('',(-0.24505,-0.0498999999999999,3.00099698131059E-17));
#16579=CARTESIAN_POINT('Origin',(0.,-0.0498999999999999,0.));
#16580=CARTESIAN_POINT('',(-0.26,-0.02,-3.18408167778312E-17));
#16581=CARTESIAN_POINT('Origin',(0.,-0.995,0.));
#16582=CARTESIAN_POINT('',(-0.24505,-1.95495,3.00099698131059E-17));
#16583=CARTESIAN_POINT('Origin',(0.,-1.95495,0.));
#16584=CARTESIAN_POINT('',(-0.24505,-0.995,-3.00099698131059E-17));
#16585=CARTESIAN_POINT('Origin',(0.,-1.975,0.));
#16586=CARTESIAN_POINT('',(-0.2,-2.,-2.44929359829471E-17));
#16587=CARTESIAN_POINT('Origin',(0.,-2.,0.));
#16588=CARTESIAN_POINT('',(-0.225,-1.975,-2.75545529808154E-17));
#16589=CARTESIAN_POINT('Origin',(0.,-2.,0.));
#16590=CARTESIAN_POINT('Origin',(0.115470053837925,-0.5,-0.2));
#16591=CARTESIAN_POINT('',(0.23094010767585,-0.5,0.));
#16592=CARTESIAN_POINT('',(0.115470053837925,-0.5,-0.2));
#16593=CARTESIAN_POINT('',(0.23094010767585,-0.5,0.));
#16594=CARTESIAN_POINT('',(0.115470053837925,-0.8,-0.2));
#16595=CARTESIAN_POINT('',(0.115470053837925,-0.5,-0.2));
#16596=CARTESIAN_POINT('',(0.23094010767585,-0.8,0.));
#16597=CARTESIAN_POINT('',(0.23094010767585,-0.8,0.));
#16598=CARTESIAN_POINT('',(0.23094010767585,-0.5,0.));
#16599=CARTESIAN_POINT('Origin',(-0.115470053837925,-0.5,-0.2));
#16600=CARTESIAN_POINT('',(-0.115470053837925,-0.5,-0.2));
#16601=CARTESIAN_POINT('',(0.115470053837925,-0.5,-0.2));
#16602=CARTESIAN_POINT('',(-0.115470053837925,-0.8,-0.2));
#16603=CARTESIAN_POINT('',(-0.115470053837925,-0.5,-0.2));
#16604=CARTESIAN_POINT('',(0.115470053837925,-0.8,-0.2));
#16605=CARTESIAN_POINT('Origin',(-0.23094010767585,-0.5,-2.77555756156289E-17));
#16606=CARTESIAN_POINT('',(-0.23094010767585,-0.5,-2.82820063659975E-17));
#16607=CARTESIAN_POINT('',(-0.115470053837925,-0.5,-0.2));
#16608=CARTESIAN_POINT('',(-0.23094010767585,-0.8,-2.77555756156289E-17));
#16609=CARTESIAN_POINT('',(-0.23094010767585,-0.5,-2.82820063659975E-17));
#16610=CARTESIAN_POINT('',(-0.115470053837925,-0.8,-0.2));
#16611=CARTESIAN_POINT('Origin',(-0.115470053837925,-0.5,0.2));
#16612=CARTESIAN_POINT('',(-0.115470053837925,-0.5,0.2));
#16613=CARTESIAN_POINT('',(-0.23094010767585,-0.5,-2.82820063659975E-17));
#16614=CARTESIAN_POINT('',(-0.115470053837925,-0.8,0.2));
#16615=CARTESIAN_POINT('',(-0.115470053837925,-0.5,0.2));
#16616=CARTESIAN_POINT('',(-0.23094010767585,-0.8,-2.82820063659975E-17));
#16617=CARTESIAN_POINT('Origin',(0.115470053837925,-0.5,0.2));
#16618=CARTESIAN_POINT('',(0.115470053837925,-0.5,0.2));
#16619=CARTESIAN_POINT('',(-0.115470053837925,-0.5,0.2));
#16620=CARTESIAN_POINT('',(0.115470053837925,-0.8,0.2));
#16621=CARTESIAN_POINT('',(0.115470053837925,-0.5,0.2));
#16622=CARTESIAN_POINT('',(-0.115470053837925,-0.8,0.2));
#16623=CARTESIAN_POINT('Origin',(0.23094010767585,-0.5,0.));
#16624=CARTESIAN_POINT('',(0.115470053837925,-0.5,0.2));
#16625=CARTESIAN_POINT('',(0.115470053837925,-0.8,0.2));
#16626=CARTESIAN_POINT('Origin',(0.,-0.5,0.));
#16627=CARTESIAN_POINT('Origin',(0.,-0.8,0.));
#16628=CARTESIAN_POINT('',(0.,0.,0.));
#16629=CARTESIAN_POINT('Origin',(0.45,0.6,0.));
#16630=CARTESIAN_POINT('',(-0.45,0.6,-5.51091059616309E-17));
#16631=CARTESIAN_POINT('Origin',(0.,0.6,0.));
#16632=CARTESIAN_POINT('Origin',(0.,0.575,0.));
#16633=CARTESIAN_POINT('',(-0.5,0.55,-6.12323399573677E-17));
#16634=CARTESIAN_POINT('Origin',(0.,0.55,0.));
#16635=CARTESIAN_POINT('',(-0.475,0.575,-5.81707229594993E-17));
#16636=CARTESIAN_POINT('Origin',(0.,0.29,0.));
#16637=CARTESIAN_POINT('',(-0.5,0.0299999999999998,-6.12323399573677E-17));
#16638=CARTESIAN_POINT('Origin',(0.,0.0299999999999998,0.));
#16639=CARTESIAN_POINT('',(-0.5,0.29,-6.12323399573677E-17));
#16640=CARTESIAN_POINT('Origin',(0.,0.0150000000000001,0.));
#16641=CARTESIAN_POINT('',(-0.47,7.11236625150491E-17,-5.75583995599256E-17));
#16642=CARTESIAN_POINT('Origin',(0.,0.,0.));
#16643=CARTESIAN_POINT('',(-0.485,0.0150000000000001,-5.93953697586466E-17));
#16644=CARTESIAN_POINT('Origin',(0.32,0.,0.));
#16645=CARTESIAN_POINT('',(-0.32,-6.93889390390723E-18,-3.91886975727153E-17));
#16646=CARTESIAN_POINT('Origin',(0.,0.,0.));
#16647=CARTESIAN_POINT('Origin',(0.,-0.02,0.));
#16648=CARTESIAN_POINT('',(-0.2942,-0.0515999999999999,3.60291088309151E-17));
#16649=CARTESIAN_POINT('Origin',(0.,-0.0515999999999999,0.));
#16650=CARTESIAN_POINT('',(-0.31,-0.02,-3.7964050773568E-17));
#16651=CARTESIAN_POINT('Origin',(0.,-1.24,0.));
#16652=CARTESIAN_POINT('',(-0.2942,-2.4458,3.60291088309151E-17));
#16653=CARTESIAN_POINT('Origin',(0.,-2.4458,0.));
#16654=CARTESIAN_POINT('',(-0.2942,-1.24,-3.60291088309151E-17));
#16655=CARTESIAN_POINT('Origin',(0.,-2.47,0.));
#16656=CARTESIAN_POINT('',(-0.24,-2.5,-2.93915231795365E-17));
#16657=CARTESIAN_POINT('Origin',(0.,-2.5,0.));
#16658=CARTESIAN_POINT('',(-0.27,-2.47,-3.30654635769785E-17));
#16659=CARTESIAN_POINT('Origin',(0.,-2.5,0.));
#16660=CARTESIAN_POINT('Origin',(0.144337567297406,-0.6,-0.25));
#16661=CARTESIAN_POINT('',(0.288675134594813,-0.6,0.));
#16662=CARTESIAN_POINT('',(0.144337567297406,-0.6,-0.25));
#16663=CARTESIAN_POINT('',(0.288675134594813,-0.6,0.));
#16664=CARTESIAN_POINT('',(0.144337567297406,-0.96,-0.25));
#16665=CARTESIAN_POINT('',(0.144337567297406,-0.6,-0.25));
#16666=CARTESIAN_POINT('',(0.288675134594813,-0.96,0.));
#16667=CARTESIAN_POINT('',(0.288675134594813,-0.96,0.));
#16668=CARTESIAN_POINT('',(0.288675134594813,-0.6,0.));
#16669=CARTESIAN_POINT('Origin',(-0.144337567297406,-0.6,-0.25));
#16670=CARTESIAN_POINT('',(-0.144337567297406,-0.6,-0.25));
#16671=CARTESIAN_POINT('',(0.144337567297406,-0.6,-0.25));
#16672=CARTESIAN_POINT('',(-0.144337567297406,-0.96,-0.25));
#16673=CARTESIAN_POINT('',(-0.144337567297406,-0.6,-0.25));
#16674=CARTESIAN_POINT('',(0.144337567297406,-0.96,-0.25));
#16675=CARTESIAN_POINT('Origin',(-0.288675134594813,-0.6,-8.32667268468867E-17));
#16676=CARTESIAN_POINT('',(-0.288675134594813,-0.6,-3.53525079574969E-17));
#16677=CARTESIAN_POINT('',(-0.144337567297406,-0.6,-0.25));
#16678=CARTESIAN_POINT('',(-0.288675134594813,-0.96,-5.55111512312578E-17));
#16679=CARTESIAN_POINT('',(-0.288675134594813,-0.6,-3.53525079574969E-17));
#16680=CARTESIAN_POINT('',(-0.144337567297406,-0.96,-0.25));
#16681=CARTESIAN_POINT('Origin',(-0.144337567297407,-0.6,0.25));
#16682=CARTESIAN_POINT('',(-0.144337567297407,-0.6,0.25));
#16683=CARTESIAN_POINT('',(-0.288675134594813,-0.6,-3.53525079574969E-17));
#16684=CARTESIAN_POINT('',(-0.144337567297407,-0.96,0.25));
#16685=CARTESIAN_POINT('',(-0.144337567297407,-0.6,0.25));
#16686=CARTESIAN_POINT('',(-0.288675134594813,-0.96,-3.53525079574969E-17));
#16687=CARTESIAN_POINT('Origin',(0.144337567297406,-0.6,0.25));
#16688=CARTESIAN_POINT('',(0.144337567297406,-0.6,0.25));
#16689=CARTESIAN_POINT('',(-0.144337567297407,-0.6,0.25));
#16690=CARTESIAN_POINT('',(0.144337567297406,-0.96,0.25));
#16691=CARTESIAN_POINT('',(0.144337567297406,-0.6,0.25));
#16692=CARTESIAN_POINT('',(-0.144337567297407,-0.96,0.25));
#16693=CARTESIAN_POINT('Origin',(0.288675134594813,-0.6,0.));
#16694=CARTESIAN_POINT('',(0.144337567297406,-0.6,0.25));
#16695=CARTESIAN_POINT('',(0.144337567297406,-0.96,0.25));
#16696=CARTESIAN_POINT('Origin',(0.,-0.6,0.));
#16697=CARTESIAN_POINT('Origin',(0.,-0.96,0.));
#16698=CARTESIAN_POINT('',(0.,0.,0.));
#16699=CARTESIAN_POINT('',(0.,0.,0.));
#16700=CARTESIAN_POINT('Origin',(0.,0.,0.));
#16701=CARTESIAN_POINT('',(-1.070235,-0.308121667383195,-1.31065986708547E-16));
#16702=CARTESIAN_POINT('',(-1.31065986708547E-16,-0.308121667383195,1.070235));
#16703=CARTESIAN_POINT('Origin',(0.,-0.308121667383195,0.));
#16704=CARTESIAN_POINT('Origin',(0.,-0.308121667383195,0.));
#16705=CARTESIAN_POINT('',(-1.31065986708547E-16,0.308121667383195,1.070235));
#16706=CARTESIAN_POINT('Origin',(-1.34711147906209E-16,0.,1.1));
#16707=CARTESIAN_POINT('',(-1.070235,0.308121667383195,1.31065986708547E-16));
#16708=CARTESIAN_POINT('Origin',(0.,0.308121667383195,0.));
#16709=CARTESIAN_POINT('Origin',(0.,0.308121667383195,0.));
#16710=CARTESIAN_POINT('Origin',(0.,0.,0.));
#16711=CARTESIAN_POINT('',(-1.070235,0.5,-1.31065986708547E-16));
#16712=CARTESIAN_POINT('',(-1.070235,0.,-1.31065986708547E-16));
#16713=CARTESIAN_POINT('Origin',(0.,0.5,0.));
#16714=CARTESIAN_POINT('Origin',(0.,0.,0.));
#16715=CARTESIAN_POINT('',(-0.6,-0.44,-7.34788079488412E-17));
#16716=CARTESIAN_POINT('Origin',(0.,-0.44,0.));
#16717=CARTESIAN_POINT('',(-0.6,0.44,-7.34788079488412E-17));
#16718=CARTESIAN_POINT('',(-0.6,0.,-7.34788079488412E-17));
#16719=CARTESIAN_POINT('Origin',(0.,0.44,0.));
#16720=CARTESIAN_POINT('Origin',(0.,0.47,0.));
#16721=CARTESIAN_POINT('',(-0.66,0.5,-8.08266887437253E-17));
#16722=CARTESIAN_POINT('',(-0.63,0.47,-7.71527483462832E-17));
#16723=CARTESIAN_POINT('Origin',(0.,0.5,0.));
#16724=CARTESIAN_POINT('Origin',(1.070235,0.5,0.));
#16725=CARTESIAN_POINT('Origin',(0.,0.,0.));
#16726=CARTESIAN_POINT('',(-1.070235,-0.5,-1.31065986708547E-16));
#16727=CARTESIAN_POINT('Origin',(0.,-0.5,0.));
#16728=CARTESIAN_POINT('',(-1.070235,0.,-1.31065986708547E-16));
#16729=CARTESIAN_POINT('Origin',(0.66,-0.5,0.));
#16730=CARTESIAN_POINT('',(-0.66,-0.5,-8.08266887437253E-17));
#16731=CARTESIAN_POINT('Origin',(0.,-0.5,0.));
#16732=CARTESIAN_POINT('Origin',(0.,-0.47,0.));
#16733=CARTESIAN_POINT('',(-0.63,-0.47,-7.71527483462832E-17));
#16734=CARTESIAN_POINT('',(0.,0.,0.));
#16735=CARTESIAN_POINT('Origin',(0.,0.,0.));
#16736=CARTESIAN_POINT('',(-1.129765,0.308121667383195,-1.38356309103871E-16));
#16737=CARTESIAN_POINT('',(-1.38356309103871E-16,0.308121667383195,1.129765));
#16738=CARTESIAN_POINT('Origin',(0.,0.308121667383195,0.));
#16739=CARTESIAN_POINT('Origin',(0.,0.308121667383195,0.));
#16740=CARTESIAN_POINT('',(-1.38356309103871E-16,-0.308121667383195,1.129765));
#16741=CARTESIAN_POINT('Origin',(-1.34711147906209E-16,0.,1.1));
#16742=CARTESIAN_POINT('',(-1.129765,-0.308121667383195,1.38356309103871E-16));
#16743=CARTESIAN_POINT('Origin',(0.,-0.308121667383195,0.));
#16744=CARTESIAN_POINT('Origin',(0.,-0.308121667383195,0.));
#16745=CARTESIAN_POINT('Origin',(0.,0.,0.));
#16746=CARTESIAN_POINT('',(-1.129765,-0.5,-1.38356309103871E-16));
#16747=CARTESIAN_POINT('Origin',(0.,-0.5,0.));
#16748=CARTESIAN_POINT('',(-1.129765,0.,-1.38356309103871E-16));
#16749=CARTESIAN_POINT('Origin',(1.54,0.5,0.));
#16750=CARTESIAN_POINT('',(-1.54,0.5,-1.88595607068692E-16));
#16751=CARTESIAN_POINT('Origin',(0.,0.5,0.));
#16752=CARTESIAN_POINT('',(-1.129765,0.5,-1.38356309103871E-16));
#16753=CARTESIAN_POINT('Origin',(0.,0.5,0.));
#16754=CARTESIAN_POINT('Origin',(0.,0.47,0.));
#16755=CARTESIAN_POINT('',(-1.6,0.44,-1.95943487863577E-16));
#16756=CARTESIAN_POINT('Origin',(0.,0.44,0.));
#16757=CARTESIAN_POINT('',(-1.57,0.47,-1.92269547466134E-16));
#16758=CARTESIAN_POINT('Origin',(0.,0.,0.));
#16759=CARTESIAN_POINT('',(-1.6,-0.44,-1.95943487863577E-16));
#16760=CARTESIAN_POINT('Origin',(0.,-0.44,0.));
#16761=CARTESIAN_POINT('',(-1.6,0.,-1.95943487863577E-16));
#16762=CARTESIAN_POINT('Origin',(0.,-0.47,0.));
#16763=CARTESIAN_POINT('',(-1.54,-0.5,-1.88595607068692E-16));
#16764=CARTESIAN_POINT('Origin',(0.,-0.5,0.));
#16765=CARTESIAN_POINT('',(-1.57,-0.47,-1.92269547466134E-16));
#16766=CARTESIAN_POINT('Origin',(1.129765,-0.5,0.));
#16767=CARTESIAN_POINT('Origin',(0.,0.,0.));
#16768=CARTESIAN_POINT('',(-1.129765,0.,-1.38356309103871E-16));
#16769=CARTESIAN_POINT('',(0.,0.,0.));
#16770=CARTESIAN_POINT('Origin',(1.1,0.,0.));
#16771=CARTESIAN_POINT('',(1.1,-2.23201749654651E-33,0.29765));
#16772=CARTESIAN_POINT('',(1.1,-2.23201749654651E-33,-0.29765));
#16773=CARTESIAN_POINT('Origin',(1.1,0.,0.));
#16774=CARTESIAN_POINT('Origin',(0.685838782044607,0.,-0.860014630714833));
#16775=CARTESIAN_POINT('',(0.918550922801216,-5.31350540756609E-33,-0.674432891191581));
#16776=CARTESIAN_POINT('',(0.453126641287998,8.49470414473068E-34,-1.04559637023808));
#16777=CARTESIAN_POINT('Origin',(0.685838782044607,0.,-0.860014630714833));
#16778=CARTESIAN_POINT('Origin',(-0.244773027351946,0.,-1.07242070340001));
#16779=CARTESIAN_POINT('',(0.0454142657089739,-2.23201749654651E-33,-1.1386540593921));
#16780=CARTESIAN_POINT('',(-0.534960320412865,-2.23201749654651E-33,-1.00618734740791));
#16781=CARTESIAN_POINT('Origin',(-0.244773027351946,0.,-1.07242070340001));
#16782=CARTESIAN_POINT('Origin',(-0.991065754692661,0.,-0.477272113029314));
#16783=CARTESIAN_POINT('',(-0.86192025974432,8.49470414473067E-34,-0.745445496560469));
#16784=CARTESIAN_POINT('',(-1.120211249641,-5.31350540756609E-33,-0.209098729498159));
#16785=CARTESIAN_POINT('Origin',(-0.991065754692661,0.,-0.477272113029314));
#16786=CARTESIAN_POINT('Origin',(-0.991065754692661,0.,0.477272113029314));
#16787=CARTESIAN_POINT('',(-1.120211249641,-2.23201749654651E-33,0.209098729498159));
#16788=CARTESIAN_POINT('',(-0.86192025974432,-2.23201749654651E-33,0.745445496560469));
#16789=CARTESIAN_POINT('Origin',(-0.991065754692661,0.,0.477272113029314));
#16790=CARTESIAN_POINT('Origin',(-0.244773027351946,0.,1.07242070340001));
#16791=CARTESIAN_POINT('',(-0.534960320412866,-2.23201749654651E-33,1.00618734740791));
#16792=CARTESIAN_POINT('',(0.0454142657089737,-2.23201749654651E-33,1.1386540593921));
#16793=CARTESIAN_POINT('Origin',(-0.244773027351946,0.,1.07242070340001));
#16794=CARTESIAN_POINT('Origin',(0.685838782044607,0.,0.860014630714833));
#16795=CARTESIAN_POINT('',(0.453126641287998,-2.23201749654651E-33,1.04559637023808));
#16796=CARTESIAN_POINT('',(0.918550922801216,-2.23201749654651E-33,0.674432891191581));
#16797=CARTESIAN_POINT('Origin',(0.685838782044607,0.,0.860014630714833));
#16798=CARTESIAN_POINT('',(0.,0.,0.));
#16799=CARTESIAN_POINT('Origin',(0.685838782044607,0.,0.860014630714833));
#16800=CARTESIAN_POINT('',(0.413083465285518,-0.05953,0.993751811093549));
#16801=CARTESIAN_POINT('',(0.876916659919095,-0.05953,0.623857181492959));
#16802=CARTESIAN_POINT('Ctrl Pts',(0.413083465285518,-0.05953,0.993751811093549));
#16803=CARTESIAN_POINT('Ctrl Pts',(0.419070565453383,-0.0925528133349865,
0.991263089003441));
#16804=CARTESIAN_POINT('Ctrl Pts',(0.430199341854858,-0.124911173756694,
0.986608710139579));
#16805=CARTESIAN_POINT('Ctrl Pts',(0.457978755888596,-0.177924977804098,
0.973971221090534));
#16806=CARTESIAN_POINT('Ctrl Pts',(0.473077587363685,-0.199697230012983,
0.966820759530997));
#16807=CARTESIAN_POINT('Ctrl Pts',(0.507057380724533,-0.237895043532788,
0.949440676105255));
#16808=CARTESIAN_POINT('Ctrl Pts',(0.525933334162555,-0.254319232363049,
0.939198248544428));
#16809=CARTESIAN_POINT('Ctrl Pts',(0.564362943424238,-0.28018331644634,
0.916597376014514));
#16810=CARTESIAN_POINT('Ctrl Pts',(0.585840553788742,-0.29104845371857,
0.903141581680914));
#16811=CARTESIAN_POINT('Ctrl Pts',(0.629305439856167,-0.30527573347708,
0.873412008702649));
#16812=CARTESIAN_POINT('Ctrl Pts',(0.651278921914856,-0.308638795020976,
0.857118508332695));
#16813=CARTESIAN_POINT('Ctrl Pts',(0.690705563850638,-0.308638795020976,
0.825676810575914));
#16814=CARTESIAN_POINT('Ctrl Pts',(0.711480111898423,-0.30527573347708,
0.807879894508811));
#16815=CARTESIAN_POINT('Ctrl Pts',(0.750136149454208,-0.29104845371857,
0.772120216227122));
#16816=CARTESIAN_POINT('Ctrl Pts',(0.768033796848072,-0.28018331644634,
0.754175290318038));
#16817=CARTESIAN_POINT('Ctrl Pts',(0.798619410861634,-0.254319232363049,
0.721738358858166));
#16818=CARTESIAN_POINT('Ctrl Pts',(0.812805334167529,-0.237895043532788,
0.705614819529209));
#16819=CARTESIAN_POINT('Ctrl Pts',(0.837310877969633,-0.199697230012983,
0.676354402927683));
#16820=CARTESIAN_POINT('Ctrl Pts',(0.847641868610495,-0.177924977804098,
0.663225258065736));
#16821=CARTESIAN_POINT('Ctrl Pts',(0.866144010579847,-0.124911173756694,
0.638954437806245));
#16822=CARTESIAN_POINT('Ctrl Pts',(0.873158080166742,-0.0925528133349865,
0.62914037979579));
#16823=CARTESIAN_POINT('Ctrl Pts',(0.876916659919095,-0.05953,0.623857181492959));
#16824=CARTESIAN_POINT('',(0.437601487681057,-0.05953,1.03511272300331));
#16825=CARTESIAN_POINT('Origin',(0.685838782044607,-0.05953,0.860014630714833));
#16826=CARTESIAN_POINT('',(0.911784794170997,-0.05953,0.656964154625313));
#16827=CARTESIAN_POINT('Ctrl Pts',(0.911784794170998,-0.0595300000000001,
0.656964154625312));
#16828=CARTESIAN_POINT('Ctrl Pts',(0.909827729890942,-0.0762225747374255,
0.659680317203144));
#16829=CARTESIAN_POINT('Ctrl Pts',(0.907004864562642,-0.0928409665394228,
0.663576540841106));
#16830=CARTESIAN_POINT('Ctrl Pts',(0.895234408667242,-0.144299303100741,
0.679480524217551));
#16831=CARTESIAN_POINT('Ctrl Pts',(0.882797231409153,-0.177024326825049,
0.695831250979106));
#16832=CARTESIAN_POINT('Ctrl Pts',(0.854332839576145,-0.227269801620064,
0.73042219438957));
#16833=CARTESIAN_POINT('Ctrl Pts',(0.834863020612702,-0.251265615809407,
0.752807465209441));
#16834=CARTESIAN_POINT('Ctrl Pts',(0.800439809856111,-0.279889827963178,
0.789147407129766));
#16835=CARTESIAN_POINT('Ctrl Pts',(0.781998747691871,-0.290879136862659,
0.80756613568454));
#16836=CARTESIAN_POINT('Ctrl Pts',(0.742239891936898,-0.305251990234487,
0.844254137480382));
#16837=CARTESIAN_POINT('Ctrl Pts',(0.720906778729541,-0.308638795020976,
0.862505527716294));
#16838=CARTESIAN_POINT('Ctrl Pts',(0.680463863683392,-0.308638795020976,
0.894757676234429));
#16839=CARTESIAN_POINT('Ctrl Pts',(0.657923009631182,-0.305251990234488,
0.91149460735272));
#16840=CARTESIAN_POINT('Ctrl Pts',(0.613307674922609,-0.290879136862659,
0.942092777160053));
#16841=CARTESIAN_POINT('Ctrl Pts',(0.591247219971725,-0.279889827963178,
0.955972930713954));
#16842=CARTESIAN_POINT('Ctrl Pts',(0.548158511259202,-0.251265615809407,
0.981446681891443));
#16843=CARTESIAN_POINT('Ctrl Pts',(0.522002043615455,-0.227269801620063,
0.995447160474328));
#16844=CARTESIAN_POINT('Ctrl Pts',(0.481944444320713,-0.177024326825049,
1.01550068154148));
#16845=CARTESIAN_POINT('Ctrl Pts',(0.463236132117164,-0.14429930310074,
1.0239876538093));
#16846=CARTESIAN_POINT('Ctrl Pts',(0.445111721969657,-0.0928409665394226,
1.03192403056628));
#16847=CARTESIAN_POINT('Ctrl Pts',(0.440685038163619,-0.0762225747374254,
1.03380912944435));
#16848=CARTESIAN_POINT('Ctrl Pts',(0.437601487681056,-0.05953,1.03511272300331));
#16849=CARTESIAN_POINT('Origin',(0.685838782044607,-0.05953,0.860014630714833));
#16850=CARTESIAN_POINT('Origin',(0.,-0.208355,0.));
#16851=CARTESIAN_POINT('',(0.0548532617164168,-0.05953,1.12247250791415));
#16852=CARTESIAN_POINT('Origin',(0.,-0.05953,0.));
#16853=CARTESIAN_POINT('',(-0.536443649899848,-0.05953,0.987512846410683));
#16854=CARTESIAN_POINT('Ctrl Pts',(0.0548532617164173,-0.0595300000000001,
1.12247250791414));
#16855=CARTESIAN_POINT('Ctrl Pts',(0.05150947068137,-0.0762225747374254,
1.12263591311425));
#16856=CARTESIAN_POINT('Ctrl Pts',(0.0467032526342597,-0.0928409665394227,
1.12285816383385));
#16857=CARTESIAN_POINT('Ctrl Pts',(0.0269302585198975,-0.144299303100741,
1.12357162229597));
#16858=CARTESIAN_POINT('Ctrl Pts',(0.006392292392153,-0.177024326825049,
1.12404235695137));
#16859=CARTESIAN_POINT('Ctrl Pts',(-0.0383992541984087,-0.227269801620063,
1.12335509974011));
#16860=CARTESIAN_POINT('Ctrl Pts',(-0.0680399972366993,-0.251265615809407,
1.12208997038458));
#16861=CARTESIAN_POINT('Ctrl Pts',(-0.117914228755037,-0.279889827963178,
1.1178344036749));
#16862=CARTESIAN_POINT('Ctrl Pts',(-0.14381238480104,-0.290879136862659,
1.11490049012186));
#16863=CARTESIAN_POINT('Ctrl Pts',(-0.19728546073067,-0.305251990234488,
1.10669035995599));
#16864=CARTESIAN_POINT('Ctrl Pts',(-0.224855950742601,-0.308638795020976,
1.10139101611326));
#16865=CARTESIAN_POINT('Ctrl Pts',(-0.275287440920027,-0.308638795020976,
1.0898803575765));
#16866=CARTESIAN_POINT('Ctrl Pts',(-0.302426893214945,-0.305251990234488,
1.08269251410343));
#16867=CARTESIAN_POINT('Ctrl Pts',(-0.35416671187353,-0.290879136862659,
1.06688848765783));
#16868=CARTESIAN_POINT('Ctrl Pts',(-0.3787731215897,-0.279889827963178,
1.05829506364875));
#16869=CARTESIAN_POINT('Ctrl Pts',(-0.425554672694338,-0.251265615809407,
1.04048957871266));
#16870=CARTESIAN_POINT('Ctrl Pts',(-0.452808978448581,-0.227269801620063,
1.02876878445619));
#16871=CARTESIAN_POINT('Ctrl Pts',(-0.493462957200432,-0.177024326825049,
1.0099536580922));
#16872=CARTESIAN_POINT('Ctrl Pts',(-0.511762781179148,-0.14429930310074,
1.00061845128527));
#16873=CARTESIAN_POINT('Ctrl Pts',(-0.529268075276157,-0.0928409665394226,
0.991396466802468));
#16874=CARTESIAN_POINT('Ctrl Pts',(-0.533501897135713,-0.0762225747374254,
0.989110885965947));
#16875=CARTESIAN_POINT('Ctrl Pts',(-0.536443649899848,-0.0595300000000001,
0.987512846410683));
#16876=CARTESIAN_POINT('',(-0.843383895613249,-0.05953,0.742736168477219));
#16877=CARTESIAN_POINT('Origin',(0.,-0.05953,0.));
#16878=CARTESIAN_POINT('',(-1.10653577764992,-0.05953,0.196295654879792));
#16879=CARTESIAN_POINT('Ctrl Pts',(-0.843383895613249,-0.0595300000000001,
0.742736168477219));
#16880=CARTESIAN_POINT('Ctrl Pts',(-0.84559647055299,-0.0762225747374255,
0.740223768851062));
#16881=CARTESIAN_POINT('Ctrl Pts',(-0.848766861100456,-0.0928409665394227,
0.736604687327351));
#16882=CARTESIAN_POINT('Ctrl Pts',(-0.861652925570091,-0.144299303100741,
0.721590372101268));
#16883=CARTESIAN_POINT('Ctrl Pts',(-0.87482617317514,-0.177024326825049,
0.705826641853758));
#16884=CARTESIAN_POINT('Ctrl Pts',(-0.902215926359523,-0.227269801620063,
0.670378702718353));
#16885=CARTESIAN_POINT('Ctrl Pts',(-0.919707509403859,-0.251265615809407,
0.646415841396062));
#16886=CARTESIAN_POINT('Ctrl Pts',(-0.947476448101718,-0.279889827963178,
0.604769294586516));
#16887=CARTESIAN_POINT('Ctrl Pts',(-0.961329858300736,-0.290879136862659,
0.582692035672022));
#16888=CARTESIAN_POINT('Ctrl Pts',(-0.988250837578047,-0.305251990234488,
0.535766169015486));
#16889=CARTESIAN_POINT('Ctrl Pts',(-1.00129756308006,-0.308638795020976,
0.510906605094603));
#16890=CARTESIAN_POINT('Ctrl Pts',(-1.02374168767024,-0.308638795020976,
0.46430090015576));
#16891=CARTESIAN_POINT('Ctrl Pts',(-1.03504317708586,-0.305251990234488,
0.438600874831839));
#16892=CARTESIAN_POINT('Ctrl Pts',(-1.05494634094458,-0.290879136862659,
0.388295406390235));
#16893=CARTESIAN_POINT('Ctrl Pts',(-1.06356957703048,-0.279889827963178,
0.363699428370917));
#16894=CARTESIAN_POINT('Ctrl Pts',(-1.0788165083757,-0.251265615809407,
0.316022600643821));
#16895=CARTESIAN_POINT('Ctrl Pts',(-1.08664560412098,-0.227269801620063,
0.287406530683752));
#16896=CARTESIAN_POINT('Ctrl Pts',(-1.09728268713976,-0.177024326825049,
0.243890930799337));
#16897=CARTESIAN_POINT('Ctrl Pts',(-1.10139388218929,-0.144299303100741,
0.22376314604679));
#16898=CARTESIAN_POINT('Ctrl Pts',(-1.10509821673782,-0.0928409665394227,
0.204327142733961));
#16899=CARTESIAN_POINT('Ctrl Pts',(-1.10595102243643,-0.0762225747374254,
0.199591971170104));
#16900=CARTESIAN_POINT('Ctrl Pts',(-1.10653577764992,-0.0595300000000001,
0.196295654879792));
#16901=CARTESIAN_POINT('',(-1.123812,-0.05953,1.37627276864339E-16));
#16902=CARTESIAN_POINT('Origin',(0.,-0.05953,0.));
#16903=CARTESIAN_POINT('',(-1.123812,-0.35718,1.37627276864339E-16));
#16904=CARTESIAN_POINT('',(-1.123812,-0.208355,1.37627276864339E-16));
#16905=CARTESIAN_POINT('Origin',(0.,-0.35718,0.));
#16906=CARTESIAN_POINT('',(-1.10653577764992,-0.05953,-0.196295654879793));
#16907=CARTESIAN_POINT('Origin',(0.,-0.05953,0.));
#16908=CARTESIAN_POINT('',(-0.843383895613249,-0.05953,-0.742736168477219));
#16909=CARTESIAN_POINT('Ctrl Pts',(-1.10653577764992,-0.0595300000000001,
-0.196295654879792));
#16910=CARTESIAN_POINT('Ctrl Pts',(-1.10595102243643,-0.0762225747374255,
-0.199591971170104));
#16911=CARTESIAN_POINT('Ctrl Pts',(-1.10509821673782,-0.0928409665394228,
-0.204327142733962));
#16912=CARTESIAN_POINT('Ctrl Pts',(-1.10139388218929,-0.144299303100741,
-0.22376314604679));
#16913=CARTESIAN_POINT('Ctrl Pts',(-1.09728268713976,-0.177024326825049,
-0.243890930799338));
#16914=CARTESIAN_POINT('Ctrl Pts',(-1.08664560412098,-0.227269801620063,
-0.287406530683753));
#16915=CARTESIAN_POINT('Ctrl Pts',(-1.0788165083757,-0.251265615809407,
-0.316022600643821));
#16916=CARTESIAN_POINT('Ctrl Pts',(-1.06356957703048,-0.279889827963178,
-0.363699428370918));
#16917=CARTESIAN_POINT('Ctrl Pts',(-1.05494634094458,-0.290879136862659,
-0.388295406390235));
#16918=CARTESIAN_POINT('Ctrl Pts',(-1.03504317708586,-0.305251990234488,
-0.438600874831839));
#16919=CARTESIAN_POINT('Ctrl Pts',(-1.02374168767024,-0.308638795020976,
-0.46430090015576));
#16920=CARTESIAN_POINT('Ctrl Pts',(-1.00129756308006,-0.308638795020976,
-0.510906605094603));
#16921=CARTESIAN_POINT('Ctrl Pts',(-0.988250837578047,-0.305251990234488,
-0.535766169015486));
#16922=CARTESIAN_POINT('Ctrl Pts',(-0.961329858300736,-0.290879136862659,
-0.582692035672022));
#16923=CARTESIAN_POINT('Ctrl Pts',(-0.947476448101718,-0.279889827963178,
-0.604769294586516));
#16924=CARTESIAN_POINT('Ctrl Pts',(-0.919707509403859,-0.251265615809407,
-0.646415841396062));
#16925=CARTESIAN_POINT('Ctrl Pts',(-0.902215926359523,-0.227269801620064,
-0.670378702718353));
#16926=CARTESIAN_POINT('Ctrl Pts',(-0.87482617317514,-0.177024326825049,
-0.705826641853758));
#16927=CARTESIAN_POINT('Ctrl Pts',(-0.861652925570091,-0.144299303100741,
-0.721590372101268));
#16928=CARTESIAN_POINT('Ctrl Pts',(-0.848766861100456,-0.0928409665394229,
-0.736604687327351));
#16929=CARTESIAN_POINT('Ctrl Pts',(-0.84559647055299,-0.0762225747374255,
-0.740223768851063));
#16930=CARTESIAN_POINT('Ctrl Pts',(-0.843383895613249,-0.0595300000000001,
-0.742736168477219));
#16931=CARTESIAN_POINT('',(-0.536443649899847,-0.05953,-0.987512846410683));
#16932=CARTESIAN_POINT('Origin',(0.,-0.05953,0.));
#16933=CARTESIAN_POINT('',(0.0548532617164172,-0.05953,-1.12247250791415));
#16934=CARTESIAN_POINT('Ctrl Pts',(-0.536443649899848,-0.0595300000000001,
-0.987512846410683));
#16935=CARTESIAN_POINT('Ctrl Pts',(-0.533501897135712,-0.0762225747374254,
-0.989110885965947));
#16936=CARTESIAN_POINT('Ctrl Pts',(-0.529268075276156,-0.0928409665394227,
-0.991396466802469));
#16937=CARTESIAN_POINT('Ctrl Pts',(-0.511762781179147,-0.144299303100741,
-1.00061845128527));
#16938=CARTESIAN_POINT('Ctrl Pts',(-0.493462957200432,-0.177024326825049,
-1.0099536580922));
#16939=CARTESIAN_POINT('Ctrl Pts',(-0.45280897844858,-0.227269801620063,
-1.02876878445619));
#16940=CARTESIAN_POINT('Ctrl Pts',(-0.425554672694337,-0.251265615809407,
-1.04048957871266));
#16941=CARTESIAN_POINT('Ctrl Pts',(-0.3787731215897,-0.279889827963178,
-1.05829506364875));
#16942=CARTESIAN_POINT('Ctrl Pts',(-0.354166711873529,-0.290879136862659,
-1.06688848765783));
#16943=CARTESIAN_POINT('Ctrl Pts',(-0.302426893214944,-0.305251990234488,
-1.08269251410343));
#16944=CARTESIAN_POINT('Ctrl Pts',(-0.275287440920027,-0.308638795020976,
-1.0898803575765));
#16945=CARTESIAN_POINT('Ctrl Pts',(-0.224855950742601,-0.308638795020976,
-1.10139101611326));
#16946=CARTESIAN_POINT('Ctrl Pts',(-0.19728546073067,-0.305251990234488,
-1.10669035995599));
#16947=CARTESIAN_POINT('Ctrl Pts',(-0.143812384801039,-0.290879136862659,
-1.11490049012186));
#16948=CARTESIAN_POINT('Ctrl Pts',(-0.117914228755037,-0.279889827963178,
-1.1178344036749));
#16949=CARTESIAN_POINT('Ctrl Pts',(-0.0680399972366989,-0.251265615809407,
-1.12208997038458));
#16950=CARTESIAN_POINT('Ctrl Pts',(-0.0383992541984084,-0.227269801620063,
-1.12335509974011));
#16951=CARTESIAN_POINT('Ctrl Pts',(0.00639229239215326,-0.177024326825049,
-1.12404235695137));
#16952=CARTESIAN_POINT('Ctrl Pts',(0.0269302585198977,-0.144299303100741,
-1.12357162229597));
#16953=CARTESIAN_POINT('Ctrl Pts',(0.04670325263426,-0.0928409665394228,
-1.12285816383385));
#16954=CARTESIAN_POINT('Ctrl Pts',(0.0515094706813703,-0.0762225747374255,
-1.12263591311425));
#16955=CARTESIAN_POINT('Ctrl Pts',(0.0548532617164176,-0.0595300000000001,
-1.12247250791414));
#16956=CARTESIAN_POINT('',(0.437601487681057,-0.05953,-1.03511272300331));
#16957=CARTESIAN_POINT('Origin',(0.,-0.05953,0.));
#16958=CARTESIAN_POINT('',(0.911784794170997,-0.05953,-0.656964154625313));
#16959=CARTESIAN_POINT('Ctrl Pts',(0.437601487681056,-0.0595300000000001,
-1.03511272300331));
#16960=CARTESIAN_POINT('Ctrl Pts',(0.440685038163619,-0.0762225747374255,
-1.03380912944435));
#16961=CARTESIAN_POINT('Ctrl Pts',(0.445111721969657,-0.0928409665394228,
-1.03192403056628));
#16962=CARTESIAN_POINT('Ctrl Pts',(0.463236132117164,-0.144299303100741,
-1.0239876538093));
#16963=CARTESIAN_POINT('Ctrl Pts',(0.481944444320713,-0.177024326825049,
-1.01550068154148));
#16964=CARTESIAN_POINT('Ctrl Pts',(0.522002043615455,-0.227269801620064,
-0.995447160474328));
#16965=CARTESIAN_POINT('Ctrl Pts',(0.548158511259203,-0.251265615809407,
-0.981446681891443));
#16966=CARTESIAN_POINT('Ctrl Pts',(0.591247219971725,-0.279889827963178,
-0.955972930713954));
#16967=CARTESIAN_POINT('Ctrl Pts',(0.613307674922609,-0.290879136862659,
-0.942092777160053));
#16968=CARTESIAN_POINT('Ctrl Pts',(0.657923009631182,-0.305251990234487,
-0.91149460735272));
#16969=CARTESIAN_POINT('Ctrl Pts',(0.680463863683393,-0.308638795020976,
-0.894757676234429));
#16970=CARTESIAN_POINT('Ctrl Pts',(0.720906778729542,-0.308638795020976,
-0.862505527716294));
#16971=CARTESIAN_POINT('Ctrl Pts',(0.742239891936899,-0.305251990234488,
-0.844254137480381));
#16972=CARTESIAN_POINT('Ctrl Pts',(0.781998747691872,-0.290879136862659,
-0.80756613568454));
#16973=CARTESIAN_POINT('Ctrl Pts',(0.800439809856112,-0.279889827963178,
-0.789147407129765));
#16974=CARTESIAN_POINT('Ctrl Pts',(0.834863020612702,-0.251265615809407,
-0.752807465209441));
#16975=CARTESIAN_POINT('Ctrl Pts',(0.854332839576145,-0.227269801620064,
-0.73042219438957));
#16976=CARTESIAN_POINT('Ctrl Pts',(0.882797231409153,-0.177024326825049,
-0.695831250979106));
#16977=CARTESIAN_POINT('Ctrl Pts',(0.895234408667242,-0.144299303100741,
-0.679480524217551));
#16978=CARTESIAN_POINT('Ctrl Pts',(0.907004864562642,-0.0928409665394228,
-0.663576540841106));
#16979=CARTESIAN_POINT('Ctrl Pts',(0.909827729890942,-0.0762225747374256,
-0.659680317203144));
#16980=CARTESIAN_POINT('Ctrl Pts',(0.911784794170998,-0.0595300000000001,
-0.656964154625312));
#16981=CARTESIAN_POINT('',(1.08212377959455,-0.05953,-0.303251606722892));
#16982=CARTESIAN_POINT('Origin',(0.,-0.05953,0.));
#16983=CARTESIAN_POINT('',(1.08212377959455,-0.05953,0.303251606722892));
#16984=CARTESIAN_POINT('Ctrl Pts',(1.08212377959455,-0.0595300000000001,
-0.303251606722892));
#16985=CARTESIAN_POINT('Ctrl Pts',(1.0830271513892,-0.0762225747374255,
-0.300028012588062));
#16986=CARTESIAN_POINT('Ctrl Pts',(1.08431331394788,-0.0928409665394228,
-0.2953917518996));
#16987=CARTESIAN_POINT('Ctrl Pts',(1.08940878963422,-0.144299303100741,
-0.276273267473431));
#16988=CARTESIAN_POINT('Ctrl Pts',(1.09443784939331,-0.177024326825049,
-0.256354979351213));
#16989=CARTESIAN_POINT('Ctrl Pts',(1.10373487993589,-0.227269801620064,
-0.212533521233765));
#16990=CARTESIAN_POINT('Ctrl Pts',(1.10909715583869,-0.251265615809407,
-0.183354415742157));
#16991=CARTESIAN_POINT('Ctrl Pts',(1.1160463456491,-0.279889827963178,-0.133783682657561));
#16992=CARTESIAN_POINT('Ctrl Pts',(1.11894887330541,-0.290879136862659,
-0.107881990270302));
#16993=CARTESIAN_POINT('Ctrl Pts',(1.12284346704144,-0.305251990234488,
-0.0539226701638766));
#16994=CARTESIAN_POINT('Ctrl Pts',(1.123812,-0.308638795020976,-0.025864214957475));
#16995=CARTESIAN_POINT('Ctrl Pts',(1.123812,-0.308638795020976,0.025864214957475));
#16996=CARTESIAN_POINT('Ctrl Pts',(1.12284346704144,-0.305251990234488,
0.0539226701638766));
#16997=CARTESIAN_POINT('Ctrl Pts',(1.11894887330541,-0.290879136862659,
0.107881990270302));
#16998=CARTESIAN_POINT('Ctrl Pts',(1.1160463456491,-0.279889827963178,0.133783682657561));
#16999=CARTESIAN_POINT('Ctrl Pts',(1.10909715583869,-0.251265615809407,
0.183354415742157));
#17000=CARTESIAN_POINT('Ctrl Pts',(1.10373487993589,-0.227269801620064,
0.212533521233765));
#17001=CARTESIAN_POINT('Ctrl Pts',(1.09443784939331,-0.177024326825049,
0.256354979351213));
#17002=CARTESIAN_POINT('Ctrl Pts',(1.08940878963422,-0.144299303100741,
0.276273267473431));
#17003=CARTESIAN_POINT('Ctrl Pts',(1.08431331394788,-0.0928409665394228,
0.2953917518996));
#17004=CARTESIAN_POINT('Ctrl Pts',(1.0830271513892,-0.0762225747374255,
0.300028012588062));
#17005=CARTESIAN_POINT('Ctrl Pts',(1.08212377959455,-0.0595300000000001,
0.303251606722892));
#17006=CARTESIAN_POINT('Origin',(0.,-0.05953,0.));
#17007=CARTESIAN_POINT('Origin',(0.,-0.05953,0.));
#17008=CARTESIAN_POINT('',(0.0589974094846122,-0.05953,1.07456964270265));
#17009=CARTESIAN_POINT('Origin',(0.,-0.05953,0.));
#17010=CARTESIAN_POINT('Origin',(-0.244773027351946,-0.05953,1.07242070340001));
#17011=CARTESIAN_POINT('Origin',(-0.244773027351946,0.,1.07242070340001));
#17012=CARTESIAN_POINT('',(-0.519393123750572,-0.05953,0.942555777842682));
#17013=CARTESIAN_POINT('Ctrl Pts',(-0.519393123750572,-0.05953,0.942555777842682));
#17014=CARTESIAN_POINT('Ctrl Pts',(-0.513714466572041,-0.0925528133349865,
0.945684988399766));
#17015=CARTESIAN_POINT('Ctrl Pts',(-0.503136848051455,-0.124911173756694,
0.951483858396181));
#17016=CARTESIAN_POINT('Ctrl Pts',(-0.47593627990192,-0.177924977804098,
0.965323333309091));
#17017=CARTESIAN_POINT('Ctrl Pts',(-0.460931856495794,-0.199697230012983,
0.972669835243841));
#17018=CARTESIAN_POINT('Ctrl Pts',(-0.426157505475872,-0.237895043532788,
0.988400002689705));
#17019=CARTESIAN_POINT('Ctrl Pts',(-0.406380688682952,-0.254319232363049,
0.996771768218699));
#17020=CARTESIAN_POINT('Ctrl Pts',(-0.364750145543744,-0.28018331644634,
1.01272583306292));
#17021=CARTESIAN_POINT('Ctrl Pts',(-0.340838910881557,-0.29104845371857,
1.02112815447116));
#17022=CARTESIAN_POINT('Ctrl Pts',(-0.290495481564827,-0.30527573347708,
1.036574285215));
#17023=CARTESIAN_POINT('Ctrl Pts',(-0.264056468041074,-0.308638795020976,
1.04359501395068));
#17024=CARTESIAN_POINT('Ctrl Pts',(-0.214892249704082,-0.308638795020976,
1.05481642595959));
#17025=CARTESIAN_POINT('Ctrl Pts',(-0.188025341585962,-0.30527573347708,
1.05996242598502));
#17026=CARTESIAN_POINT('Ctrl Pts',(-0.135965654106109,-0.29104845371857,
1.06788913840721));
#17027=CARTESIAN_POINT('Ctrl Pts',(-0.110776745452494,-0.28018331644634,
1.07069360430242));
#17028=CARTESIAN_POINT('Ctrl Pts',(-0.0663467128214646,-0.254319232363049,
1.07438230428002));
#17029=CARTESIAN_POINT('Ctrl Pts',(-0.0448960436540983,-0.237895043532788,
1.07542044338697));
#17030=CARTESIAN_POINT('Ctrl Pts',(-0.00674037211528124,-0.199697230012983,
1.07633607767727));
#17031=CARTESIAN_POINT('Ctrl Pts',(0.00996567398334777,-0.177924977804098,
1.07622728347683));
#17032=CARTESIAN_POINT('Ctrl Pts',(0.0404772621979741,-0.124911173756694,
1.07556023164702));
#17033=CARTESIAN_POINT('Ctrl Pts',(0.0525234025782719,-0.0925528133349865,
1.07492508698591));
#17034=CARTESIAN_POINT('Ctrl Pts',(0.0589974094846124,-0.05953,1.07456964270265));
#17035=CARTESIAN_POINT('Origin',(-0.244773027351946,-0.05953,1.07242070340001));
#17036=CARTESIAN_POINT('Origin',(0.,-0.05953,0.));
#17037=CARTESIAN_POINT('',(-0.803348093619616,-0.05953,0.716109245731214));
#17038=CARTESIAN_POINT('Origin',(0.,-0.05953,0.));
#17039=CARTESIAN_POINT('Origin',(-0.991065754692661,-0.05953,0.477272113029314));
#17040=CARTESIAN_POINT('Origin',(-0.991065754692661,0.,0.477272113029314));
#17041=CARTESIAN_POINT('',(-1.06075609691358,-0.05953,0.181596019242328));
#17042=CARTESIAN_POINT('Ctrl Pts',(-1.06075609691358,-0.05953,0.181596019242328));
#17043=CARTESIAN_POINT('Ctrl Pts',(-1.05966202740332,-0.0925528133349865,
0.187986803072856));
#17044=CARTESIAN_POINT('Ctrl Pts',(-1.05760072925372,-0.124911173756694,
0.199872254546857));
#17045=CARTESIAN_POINT('Ctrl Pts',(-1.05146158959546,-0.177924977804098,
0.22976728653846));
#17046=CARTESIAN_POINT('Ctrl Pts',(-1.04785021111757,-0.199697230012983,
0.246078686169301));
#17047=CARTESIAN_POINT('Ctrl Pts',(-1.03846709802406,-0.237895043532788,
0.283073967563097));
#17048=CARTESIAN_POINT('Ctrl Pts',(-1.03268176429485,-0.254319232363049,
0.303755815985685));
#17049=CARTESIAN_POINT('Ctrl Pts',(-1.01919893537026,-0.28018331644634,
0.346251081972725));
#17050=CARTESIAN_POINT('Ctrl Pts',(-1.01085972381132,-0.29104845371857,
0.370184399726282));
#17051=CARTESIAN_POINT('Ctrl Pts',(-0.99154738033959,-0.30527573347708,
0.419174982698463));
#17052=CARTESIAN_POINT('Ctrl Pts',(-0.980551951791748,-0.308638795020976,
0.444223188605045));
#17053=CARTESIAN_POINT('Ctrl Pts',(-0.958671816228589,-0.308638795020976,
0.489657758261848));
#17054=CARTESIAN_POINT('Ctrl Pts',(-0.945943877838127,-0.30527573347708,
0.51387163140139));
#17055=CARTESIAN_POINT('Ctrl Pts',(-0.91968254693063,-0.29104845371857,
0.559515758398093));
#17056=CARTESIAN_POINT('Ctrl Pts',(-0.906170138993533,-0.28018331644634,
0.580957796077825));
#17057=CARTESIAN_POINT('Ctrl Pts',(-0.8813524085237,-0.254319232363049,
0.617994461173994));
#17058=CARTESIAN_POINT('Ctrl Pts',(-0.868789784891799,-0.237895043532788,
0.635412538795143));
#17059=CARTESIAN_POINT('Ctrl Pts',(-0.845715984518854,-0.199697230012983,
0.66581473268113));
#17060=CARTESIAN_POINT('Ctrl Pts',(-0.835214876415962,-0.177924977804098,
0.678808213394124));
#17061=CARTESIAN_POINT('Ctrl Pts',(-0.815669690204649,-0.124911173756694,
0.702247233627224));
#17062=CARTESIAN_POINT('Ctrl Pts',(-0.807662468433796,-0.0925528133349865,
0.711269279199861));
#17063=CARTESIAN_POINT('Ctrl Pts',(-0.803348093619616,-0.05953,0.716109245731214));
#17064=CARTESIAN_POINT('Origin',(-0.991065754692661,-0.05953,0.477272113029314));
#17065=CARTESIAN_POINT('Origin',(0.,-0.05953,0.));
#17066=CARTESIAN_POINT('',(-1.076188,-0.05953,1.31795018948079E-16));
#17067=CARTESIAN_POINT('Origin',(0.,-0.05953,0.));
#17068=CARTESIAN_POINT('',(-1.06075609691358,-0.05953,-0.181596019242328));
#17069=CARTESIAN_POINT('Origin',(0.,-0.05953,0.));
#17070=CARTESIAN_POINT('Origin',(-0.991065754692661,-0.05953,-0.477272113029314));
#17071=CARTESIAN_POINT('Origin',(-0.991065754692661,0.,-0.477272113029314));
#17072=CARTESIAN_POINT('',(-0.803348093619616,-0.05953,-0.716109245731215));
#17073=CARTESIAN_POINT('Ctrl Pts',(-0.803348093619616,-0.05953,-0.716109245731215));
#17074=CARTESIAN_POINT('Ctrl Pts',(-0.807662468433795,-0.0925528133349865,
-0.711269279199862));
#17075=CARTESIAN_POINT('Ctrl Pts',(-0.815669690204649,-0.124911173756694,
-0.702247233627224));
#17076=CARTESIAN_POINT('Ctrl Pts',(-0.835214876415962,-0.177924977804098,
-0.678808213394124));
#17077=CARTESIAN_POINT('Ctrl Pts',(-0.845715984518854,-0.199697230012983,
-0.66581473268113));
#17078=CARTESIAN_POINT('Ctrl Pts',(-0.868789784891799,-0.237895043532788,
-0.635412538795143));
#17079=CARTESIAN_POINT('Ctrl Pts',(-0.8813524085237,-0.254319232363049,
-0.617994461173994));
#17080=CARTESIAN_POINT('Ctrl Pts',(-0.906170138993533,-0.28018331644634,
-0.580957796077826));
#17081=CARTESIAN_POINT('Ctrl Pts',(-0.91968254693063,-0.29104845371857,
-0.559515758398093));
#17082=CARTESIAN_POINT('Ctrl Pts',(-0.945943877838127,-0.30527573347708,
-0.51387163140139));
#17083=CARTESIAN_POINT('Ctrl Pts',(-0.958671816228589,-0.308638795020976,
-0.489657758261848));
#17084=CARTESIAN_POINT('Ctrl Pts',(-0.980551951791748,-0.308638795020976,
-0.444223188605045));
#17085=CARTESIAN_POINT('Ctrl Pts',(-0.99154738033959,-0.30527573347708,
-0.419174982698463));
#17086=CARTESIAN_POINT('Ctrl Pts',(-1.01085972381132,-0.29104845371857,
-0.370184399726282));
#17087=CARTESIAN_POINT('Ctrl Pts',(-1.01919893537026,-0.28018331644634,
-0.346251081972725));
#17088=CARTESIAN_POINT('Ctrl Pts',(-1.03268176429485,-0.254319232363049,
-0.303755815985685));
#17089=CARTESIAN_POINT('Ctrl Pts',(-1.03846709802406,-0.237895043532788,
-0.283073967563097));
#17090=CARTESIAN_POINT('Ctrl Pts',(-1.04785021111757,-0.199697230012983,
-0.246078686169302));
#17091=CARTESIAN_POINT('Ctrl Pts',(-1.05146158959546,-0.177924977804098,
-0.229767286538461));
#17092=CARTESIAN_POINT('Ctrl Pts',(-1.05760072925372,-0.124911173756694,
-0.199872254546858));
#17093=CARTESIAN_POINT('Ctrl Pts',(-1.05966202740332,-0.0925528133349864,
-0.187986803072857));
#17094=CARTESIAN_POINT('Ctrl Pts',(-1.06075609691358,-0.05953,-0.181596019242328));
#17095=CARTESIAN_POINT('Origin',(-0.991065754692661,-0.05953,-0.477272113029314));
#17096=CARTESIAN_POINT('Origin',(0.,-0.05953,0.));
#17097=CARTESIAN_POINT('',(-0.519393123750572,-0.05953,-0.942555777842682));
#17098=CARTESIAN_POINT('Origin',(0.,-0.05953,0.));
#17099=CARTESIAN_POINT('Origin',(-0.244773027351946,-0.05953,-1.07242070340001));
#17100=CARTESIAN_POINT('Origin',(-0.244773027351946,0.,-1.07242070340001));
#17101=CARTESIAN_POINT('',(0.0589974094846125,-0.05953,-1.07456964270265));
#17102=CARTESIAN_POINT('Ctrl Pts',(0.0589974094846127,-0.05953,-1.07456964270265));
#17103=CARTESIAN_POINT('Ctrl Pts',(0.0525234025782722,-0.0925528133349865,
-1.07492508698591));
#17104=CARTESIAN_POINT('Ctrl Pts',(0.0404772621979744,-0.124911173756694,
-1.07556023164702));
#17105=CARTESIAN_POINT('Ctrl Pts',(0.0099656739833481,-0.177924977804098,
-1.07622728347683));
#17106=CARTESIAN_POINT('Ctrl Pts',(-0.00674037211528096,-0.199697230012983,
-1.07633607767727));
#17107=CARTESIAN_POINT('Ctrl Pts',(-0.044896043654098,-0.237895043532788,
-1.07542044338697));
#17108=CARTESIAN_POINT('Ctrl Pts',(-0.0663467128214644,-0.254319232363049,
-1.07438230428002));
#17109=CARTESIAN_POINT('Ctrl Pts',(-0.110776745452493,-0.28018331644634,
-1.07069360430242));
#17110=CARTESIAN_POINT('Ctrl Pts',(-0.135965654106109,-0.29104845371857,
-1.06788913840721));
#17111=CARTESIAN_POINT('Ctrl Pts',(-0.188025341585962,-0.30527573347708,
-1.05996242598502));
#17112=CARTESIAN_POINT('Ctrl Pts',(-0.214892249704082,-0.308638795020976,
-1.05481642595959));
#17113=CARTESIAN_POINT('Ctrl Pts',(-0.264056468041074,-0.308638795020976,
-1.04359501395068));
#17114=CARTESIAN_POINT('Ctrl Pts',(-0.290495481564827,-0.30527573347708,
-1.036574285215));
#17115=CARTESIAN_POINT('Ctrl Pts',(-0.340838910881557,-0.291048453718569,
-1.02112815447116));
#17116=CARTESIAN_POINT('Ctrl Pts',(-0.364750145543744,-0.28018331644634,
-1.01272583306292));
#17117=CARTESIAN_POINT('Ctrl Pts',(-0.406380688682952,-0.254319232363049,
-0.996771768218699));
#17118=CARTESIAN_POINT('Ctrl Pts',(-0.426157505475872,-0.237895043532788,
-0.988400002689705));
#17119=CARTESIAN_POINT('Ctrl Pts',(-0.460931856495794,-0.199697230012983,
-0.972669835243841));
#17120=CARTESIAN_POINT('Ctrl Pts',(-0.475936279901919,-0.177924977804098,
-0.965323333309091));
#17121=CARTESIAN_POINT('Ctrl Pts',(-0.503136848051454,-0.124911173756694,
-0.951483858396181));
#17122=CARTESIAN_POINT('Ctrl Pts',(-0.513714466572041,-0.0925528133349865,
-0.945684988399766));
#17123=CARTESIAN_POINT('Ctrl Pts',(-0.519393123750572,-0.05953,-0.942555777842682));
#17124=CARTESIAN_POINT('Origin',(-0.244773027351946,-0.05953,-1.07242070340001));
#17125=CARTESIAN_POINT('Origin',(0.,-0.05953,0.));
#17126=CARTESIAN_POINT('',(0.413083465285518,-0.05953,-0.993751811093549));
#17127=CARTESIAN_POINT('Origin',(0.,-0.05953,0.));
#17128=CARTESIAN_POINT('Origin',(0.685838782044607,-0.05953,-0.860014630714833));
#17129=CARTESIAN_POINT('Origin',(0.685838782044607,0.,-0.860014630714833));
#17130=CARTESIAN_POINT('',(0.876916659919095,-0.05953,-0.623857181492959));
#17131=CARTESIAN_POINT('Ctrl Pts',(0.876916659919095,-0.05953,-0.623857181492958));
#17132=CARTESIAN_POINT('Ctrl Pts',(0.873158080166742,-0.0925528133349865,
-0.62914037979579));
#17133=CARTESIAN_POINT('Ctrl Pts',(0.866144010579847,-0.124911173756694,
-0.638954437806245));
#17134=CARTESIAN_POINT('Ctrl Pts',(0.847641868610495,-0.177924977804098,
-0.663225258065736));
#17135=CARTESIAN_POINT('Ctrl Pts',(0.837310877969633,-0.199697230012983,
-0.676354402927683));
#17136=CARTESIAN_POINT('Ctrl Pts',(0.81280533416753,-0.237895043532788,
-0.705614819529209));
#17137=CARTESIAN_POINT('Ctrl Pts',(0.798619410861634,-0.254319232363049,
-0.721738358858166));
#17138=CARTESIAN_POINT('Ctrl Pts',(0.768033796848072,-0.28018331644634,
-0.754175290318038));
#17139=CARTESIAN_POINT('Ctrl Pts',(0.750136149454208,-0.29104845371857,
-0.772120216227122));
#17140=CARTESIAN_POINT('Ctrl Pts',(0.711480111898423,-0.30527573347708,
-0.807879894508811));
#17141=CARTESIAN_POINT('Ctrl Pts',(0.690705563850638,-0.308638795020976,
-0.825676810575913));
#17142=CARTESIAN_POINT('Ctrl Pts',(0.651278921914856,-0.308638795020976,
-0.857118508332695));
#17143=CARTESIAN_POINT('Ctrl Pts',(0.629305439856167,-0.30527573347708,
-0.873412008702649));
#17144=CARTESIAN_POINT('Ctrl Pts',(0.585840553788742,-0.29104845371857,
-0.903141581680914));
#17145=CARTESIAN_POINT('Ctrl Pts',(0.564362943424239,-0.28018331644634,
-0.916597376014514));
#17146=CARTESIAN_POINT('Ctrl Pts',(0.525933334162556,-0.254319232363049,
-0.939198248544427));
#17147=CARTESIAN_POINT('Ctrl Pts',(0.507057380724533,-0.237895043532788,
-0.949440676105255));
#17148=CARTESIAN_POINT('Ctrl Pts',(0.473077587363686,-0.199697230012983,
-0.966820759530997));
#17149=CARTESIAN_POINT('Ctrl Pts',(0.457978755888596,-0.177924977804098,
-0.973971221090534));
#17150=CARTESIAN_POINT('Ctrl Pts',(0.430199341854858,-0.124911173756694,
-0.986608710139579));
#17151=CARTESIAN_POINT('Ctrl Pts',(0.419070565453384,-0.0925528133349865,
-0.991263089003441));
#17152=CARTESIAN_POINT('Ctrl Pts',(0.413083465285518,-0.05953,-0.993751811093549));
#17153=CARTESIAN_POINT('Origin',(0.685838782044607,-0.05953,-0.860014630714833));
#17154=CARTESIAN_POINT('Origin',(0.,-0.208355,0.));
#17155=CARTESIAN_POINT('',(-1.076188,-0.35718,1.31795018948079E-16));
#17156=CARTESIAN_POINT('Origin',(0.,-0.35718,0.));
#17157=CARTESIAN_POINT('',(-1.076188,-0.208355,1.31795018948079E-16));
#17158=CARTESIAN_POINT('',(1.03449977959455,-0.05953,0.296632461748266));
#17159=CARTESIAN_POINT('Origin',(0.,-0.05953,0.));
#17160=CARTESIAN_POINT('',(1.03449977959455,-0.05953,-0.296632461748266));
#17161=CARTESIAN_POINT('Ctrl Pts',(1.03449977959455,-0.05953,0.296632461748267));
#17162=CARTESIAN_POINT('Ctrl Pts',(1.03628691421076,-0.0925528133349865,
0.290399865505497));
#17163=CARTESIAN_POINT('Ctrl Pts',(1.03958665287714,-0.124911173756694,
0.278797079997872));
#17164=CARTESIAN_POINT('Ctrl Pts',(1.0470264474309,-0.177924977804098,0.249198913998601));
#17165=CARTESIAN_POINT('Ctrl Pts',(1.05084995891418,-0.199697230012983,
0.232935932341942));
#17166=CARTESIAN_POINT('Ctrl Pts',(1.05844771715377,-0.237895043532788,
0.195533155353269));
#17167=CARTESIAN_POINT('Ctrl Pts',(1.06220882929878,-0.254319232363049,
0.17438929156337));
#17168=CARTESIAN_POINT('Ctrl Pts',(1.06849922508772,-0.28018331644634,0.130252399648131));
#17169=CARTESIAN_POINT('Ctrl Pts',(1.07137013248666,-0.29104845371857,0.105070977154072));
#17170=CARTESIAN_POINT('Ctrl Pts',(1.07522652957392,-0.30527573347708,0.0525526752791107));
#17171=CARTESIAN_POINT('Ctrl Pts',(1.076188,-0.308638795020976,0.025214283908933));
#17172=CARTESIAN_POINT('Ctrl Pts',(1.076188,-0.308638795020976,-0.025214283908933));
#17173=CARTESIAN_POINT('Ctrl Pts',(1.07522652957392,-0.30527573347708,-0.0525526752791107));
#17174=CARTESIAN_POINT('Ctrl Pts',(1.07137013248666,-0.29104845371857,-0.105070977154072));
#17175=CARTESIAN_POINT('Ctrl Pts',(1.06849922508772,-0.28018331644634,-0.130252399648131));
#17176=CARTESIAN_POINT('Ctrl Pts',(1.06220882929878,-0.254319232363049,
-0.17438929156337));
#17177=CARTESIAN_POINT('Ctrl Pts',(1.05844771715377,-0.237895043532788,
-0.195533155353269));
#17178=CARTESIAN_POINT('Ctrl Pts',(1.05084995891418,-0.199697230012983,
-0.232935932341942));
#17179=CARTESIAN_POINT('Ctrl Pts',(1.0470264474309,-0.177924977804098,-0.249198913998601));
#17180=CARTESIAN_POINT('Ctrl Pts',(1.03958665287714,-0.124911173756694,
-0.278797079997872));
#17181=CARTESIAN_POINT('Ctrl Pts',(1.03628691421076,-0.0925528133349865,
-0.290399865505497));
#17182=CARTESIAN_POINT('Ctrl Pts',(1.03449977959455,-0.05953,-0.296632461748267));
#17183=CARTESIAN_POINT('Origin',(0.,-0.05953,0.));
#17184=CARTESIAN_POINT('Origin',(0.,-0.05953,0.));
#17185=CARTESIAN_POINT('Origin',(1.1,-0.05953,0.));
#17186=CARTESIAN_POINT('Origin',(1.1,0.,0.));
#17187=CARTESIAN_POINT('Origin',(1.1,-0.05953,0.));
#17188=CARTESIAN_POINT('Origin',(0.,-0.35718,0.));
#17189=CARTESIAN_POINT('Origin',(0.,-0.05953,0.));
#17190=CARTESIAN_POINT('',(0.,0.,0.));
#17191=CARTESIAN_POINT('Origin',(1.119765,0.495,0.));
#17192=CARTESIAN_POINT('',(-1.119765,0.495,-1.37131662304724E-16));
#17193=CARTESIAN_POINT('Origin',(0.,0.495,0.));
#17194=CARTESIAN_POINT('',(-1.085235,0.495,-1.32902956907268E-16));
#17195=CARTESIAN_POINT('Origin',(0.,0.495,0.));
#17196=CARTESIAN_POINT('Origin',(0.,0.4575,0.));
#17197=CARTESIAN_POINT('',(-1.119765,0.42,-1.37131662304724E-16));
#17198=CARTESIAN_POINT('Origin',(0.,0.42,0.));
#17199=CARTESIAN_POINT('',(-1.119765,0.4575,-1.37131662304724E-16));
#17200=CARTESIAN_POINT('Origin',(1.085235,0.42,0.));
#17201=CARTESIAN_POINT('',(-1.085235,0.42,-1.32902956907268E-16));
#17202=CARTESIAN_POINT('Origin',(0.,0.42,0.));
#17203=CARTESIAN_POINT('Origin',(0.,0.4575,0.));
#17204=CARTESIAN_POINT('',(-1.085235,0.4575,-1.32902956907268E-16));
#17205=CARTESIAN_POINT('Origin',(1.119765,-0.42,0.));
#17206=CARTESIAN_POINT('',(-1.119765,-0.42,-1.37131662304724E-16));
#17207=CARTESIAN_POINT('Origin',(0.,-0.42,0.));
#17208=CARTESIAN_POINT('',(-1.085235,-0.42,-1.32902956907268E-16));
#17209=CARTESIAN_POINT('Origin',(0.,-0.42,0.));
#17210=CARTESIAN_POINT('Origin',(0.,-0.4575,0.));
#17211=CARTESIAN_POINT('',(-1.119765,-0.495,-1.37131662304724E-16));
#17212=CARTESIAN_POINT('Origin',(0.,-0.495,0.));
#17213=CARTESIAN_POINT('',(-1.119765,-0.4575,-1.37131662304724E-16));
#17214=CARTESIAN_POINT('Origin',(1.085235,-0.495,0.));
#17215=CARTESIAN_POINT('',(-1.085235,-0.495,-1.32902956907268E-16));
#17216=CARTESIAN_POINT('Origin',(0.,-0.495,0.));
#17217=CARTESIAN_POINT('Origin',(0.,-0.4575,0.));
#17218=CARTESIAN_POINT('',(-1.085235,-0.4575,-1.32902956907268E-16));
#17219=CARTESIAN_POINT('',(0.,0.,0.));
#17220=CARTESIAN_POINT('',(0.,0.,0.));
#17221=CARTESIAN_POINT('',(0.,0.,0.));
#17222=CARTESIAN_POINT('',(0.,0.,0.));
#17223=CARTESIAN_POINT('',(0.,0.,0.));
#17224=CARTESIAN_POINT('',(0.,0.,0.));
#17225=CARTESIAN_POINT('',(0.,0.,0.));
#17226=CARTESIAN_POINT('Origin',(0.,0.,0.));
#17227=CARTESIAN_POINT('',(-1.63531,-0.410863395882378,-2.00267715711366E-16));
#17228=CARTESIAN_POINT('',(-2.00267715711366E-16,-0.410863395882378,1.63531));
#17229=CARTESIAN_POINT('Origin',(0.,-0.410863395882378,0.));
#17230=CARTESIAN_POINT('Origin',(0.,-0.410863395882378,0.));
#17231=CARTESIAN_POINT('',(-2.00267715711366E-16,0.410863395882378,1.63531));
#17232=CARTESIAN_POINT('Origin',(-2.05128338857182E-16,0.,1.675));
#17233=CARTESIAN_POINT('',(-1.63531,0.410863395882378,2.00267715711366E-16));
#17234=CARTESIAN_POINT('Origin',(0.,0.410863395882378,0.));
#17235=CARTESIAN_POINT('Origin',(0.,0.410863395882378,0.));
#17236=CARTESIAN_POINT('Origin',(0.,0.,0.));
#17237=CARTESIAN_POINT('',(-1.63531,0.7,-2.00267715711366E-16));
#17238=CARTESIAN_POINT('',(-1.63531,0.,-2.00267715711366E-16));
#17239=CARTESIAN_POINT('Origin',(0.,0.7,0.));
#17240=CARTESIAN_POINT('Origin',(0.,0.,0.));
#17241=CARTESIAN_POINT('',(-1.,-0.6,-1.22464679914735E-16));
#17242=CARTESIAN_POINT('Origin',(0.,-0.6,0.));
#17243=CARTESIAN_POINT('',(-1.,0.6,-1.22464679914735E-16));
#17244=CARTESIAN_POINT('',(-1.,0.,-1.22464679914735E-16));
#17245=CARTESIAN_POINT('Origin',(0.,0.6,0.));
#17246=CARTESIAN_POINT('Origin',(0.,0.65,0.));
#17247=CARTESIAN_POINT('',(-1.1,0.7,-1.34711147906209E-16));
#17248=CARTESIAN_POINT('',(-1.05,0.65,-1.28587913910472E-16));
#17249=CARTESIAN_POINT('Origin',(0.,0.7,0.));
#17250=CARTESIAN_POINT('Origin',(1.63531,0.7,0.));
#17251=CARTESIAN_POINT('Origin',(0.,0.,0.));
#17252=CARTESIAN_POINT('',(-1.63531,-0.7,-2.00267715711366E-16));
#17253=CARTESIAN_POINT('Origin',(0.,-0.7,0.));
#17254=CARTESIAN_POINT('',(-1.63531,0.,-2.00267715711366E-16));
#17255=CARTESIAN_POINT('Origin',(1.1,-0.7,0.));
#17256=CARTESIAN_POINT('',(-1.1,-0.7,-1.34711147906209E-16));
#17257=CARTESIAN_POINT('Origin',(0.,-0.7,0.));
#17258=CARTESIAN_POINT('Origin',(0.,-0.65,0.));
#17259=CARTESIAN_POINT('',(-1.05,-0.65,-1.28587913910472E-16));
#17260=CARTESIAN_POINT('',(0.,0.,0.));
#17261=CARTESIAN_POINT('Origin',(0.,0.,0.));
#17262=CARTESIAN_POINT('',(-1.71469,0.410863395882378,-2.09988962002998E-16));
#17263=CARTESIAN_POINT('',(-2.09988962002998E-16,0.410863395882378,1.71469));
#17264=CARTESIAN_POINT('Origin',(0.,0.410863395882378,0.));
#17265=CARTESIAN_POINT('Origin',(0.,0.410863395882378,0.));
#17266=CARTESIAN_POINT('',(-2.09988962002998E-16,-0.410863395882378,1.71469));
#17267=CARTESIAN_POINT('Origin',(-2.05128338857182E-16,0.,1.675));
#17268=CARTESIAN_POINT('',(-1.71469,-0.410863395882378,2.09988962002998E-16));
#17269=CARTESIAN_POINT('Origin',(0.,-0.410863395882378,0.));
#17270=CARTESIAN_POINT('Origin',(0.,-0.410863395882378,0.));
#17271=CARTESIAN_POINT('Origin',(0.,0.,0.));
#17272=CARTESIAN_POINT('',(-1.71469,-0.7,-2.09988962002998E-16));
#17273=CARTESIAN_POINT('Origin',(0.,-0.7,0.));
#17274=CARTESIAN_POINT('',(-1.71469,0.,-2.09988962002998E-16));
#17275=CARTESIAN_POINT('Origin',(2.25,0.7,0.));
#17276=CARTESIAN_POINT('',(-2.25,0.7,-2.75545529808154E-16));
#17277=CARTESIAN_POINT('Origin',(0.,0.7,0.));
#17278=CARTESIAN_POINT('',(-1.71469,0.7,-2.09988962002998E-16));
#17279=CARTESIAN_POINT('Origin',(0.,0.7,0.));
#17280=CARTESIAN_POINT('Origin',(0.,0.65,0.));
#17281=CARTESIAN_POINT('',(-2.35,0.6,-2.87791997799628E-16));
#17282=CARTESIAN_POINT('Origin',(0.,0.6,0.));
#17283=CARTESIAN_POINT('',(-2.3,0.65,-2.81668763803891E-16));
#17284=CARTESIAN_POINT('Origin',(0.,0.,0.));
#17285=CARTESIAN_POINT('',(-2.35,-0.6,-2.87791997799628E-16));
#17286=CARTESIAN_POINT('Origin',(0.,-0.6,0.));
#17287=CARTESIAN_POINT('',(-2.35,0.,-2.87791997799628E-16));
#17288=CARTESIAN_POINT('Origin',(0.,-0.65,0.));
#17289=CARTESIAN_POINT('',(-2.25,-0.7,-2.75545529808154E-16));
#17290=CARTESIAN_POINT('Origin',(0.,-0.7,0.));
#17291=CARTESIAN_POINT('',(-2.3,-0.65,-2.81668763803891E-16));
#17292=CARTESIAN_POINT('Origin',(1.71469,-0.7,0.));
#17293=CARTESIAN_POINT('Origin',(0.,0.,0.));
#17294=CARTESIAN_POINT('',(-1.71469,0.,-2.09988962002998E-16));
#17295=CARTESIAN_POINT('',(0.,0.,0.));
#17296=CARTESIAN_POINT('Origin',(1.675,0.,0.));
#17297=CARTESIAN_POINT('',(1.675,-2.97627328869245E-33,0.3969));
#17298=CARTESIAN_POINT('',(1.675,-2.97627328869245E-33,-0.3969));
#17299=CARTESIAN_POINT('Origin',(1.675,0.,0.));
#17300=CARTESIAN_POINT('Origin',(1.18440385848747,0.,-1.18440385848747));
#17301=CARTESIAN_POINT('',(1.46505453994041,3.1867025333467E-33,-0.903753177034526));
#17302=CARTESIAN_POINT('',(0.903753177034527,-9.13924911073161E-33,-1.46505453994041));
#17303=CARTESIAN_POINT('Origin',(1.18440385848747,0.,-1.18440385848747));
#17304=CARTESIAN_POINT('Origin',(1.02564169428591E-16,0.,-1.675));
#17305=CARTESIAN_POINT('',(0.3969,-2.97627328869246E-33,-1.675));
#17306=CARTESIAN_POINT('',(-0.3969,-2.97627328869245E-33,-1.675));
#17307=CARTESIAN_POINT('Origin',(1.02564169428591E-16,0.,-1.675));
#17308=CARTESIAN_POINT('Origin',(-1.18440385848747,0.,-1.18440385848747));
#17309=CARTESIAN_POINT('',(-0.903753177034526,3.1867025333467E-33,-1.46505453994041));
#17310=CARTESIAN_POINT('',(-1.46505453994041,-9.13924911073161E-33,-0.903753177034527));
#17311=CARTESIAN_POINT('Origin',(-1.18440385848747,0.,-1.18440385848747));
#17312=CARTESIAN_POINT('Origin',(-1.675,0.,-2.05128338857182E-16));
#17313=CARTESIAN_POINT('',(-1.675,-2.97627328869246E-33,-0.3969));
#17314=CARTESIAN_POINT('',(-1.675,-2.97627328869245E-33,0.3969));
#17315=CARTESIAN_POINT('Origin',(-1.675,0.,-2.05128338857182E-16));
#17316=CARTESIAN_POINT('Origin',(-1.18440385848747,0.,1.18440385848747));
#17317=CARTESIAN_POINT('',(-1.46505453994041,6.26819044436628E-33,0.903753177034526));
#17318=CARTESIAN_POINT('',(-0.903753177034527,-1.22207370217512E-32,1.46505453994041));
#17319=CARTESIAN_POINT('Origin',(-1.18440385848747,0.,1.18440385848747));
#17320=CARTESIAN_POINT('Origin',(-3.07692508285772E-16,0.,1.675));
#17321=CARTESIAN_POINT('',(-0.3969,-2.97627328869246E-33,1.675));
#17322=CARTESIAN_POINT('',(0.396899999999999,-2.97627328869245E-33,1.675));
#17323=CARTESIAN_POINT('Origin',(-3.07692508285772E-16,0.,1.675));
#17324=CARTESIAN_POINT('Origin',(1.18440385848747,0.,1.18440385848747));
#17325=CARTESIAN_POINT('',(0.903753177034526,9.34967835538585E-33,1.46505453994041));
#17326=CARTESIAN_POINT('',(1.46505453994041,-1.53022249327708E-32,0.903753177034527));
#17327=CARTESIAN_POINT('Origin',(1.18440385848747,0.,1.18440385848747));
#17328=CARTESIAN_POINT('',(0.,0.,0.));
#17329=CARTESIAN_POINT('Origin',(1.18440385848747,0.,1.18440385848747));
#17330=CARTESIAN_POINT('',(0.846804978391753,-0.07938,1.40825612658882));
#17331=CARTESIAN_POINT('',(1.40825612658882,-0.07938,0.846804978391754));
#17332=CARTESIAN_POINT('Ctrl Pts',(0.846804978391752,-0.0793800000000001,
1.40825612658882));
#17333=CARTESIAN_POINT('Ctrl Pts',(0.854205272175554,-0.123401821157026,
1.40380622184538));
#17334=CARTESIAN_POINT('Ctrl Pts',(0.867957148219441,-0.166543350814306,
1.39550172959303));
#17335=CARTESIAN_POINT('Ctrl Pts',(0.902193646979982,-0.237231147975234,
1.3735491215176));
#17336=CARTESIAN_POINT('Ctrl Pts',(0.920778333482564,-0.266264900654909,
1.36127834356734));
#17337=CARTESIAN_POINT('Ctrl Pts',(0.962485392528369,-0.317195968905306,
1.33211611256184));
#17338=CARTESIAN_POINT('Ctrl Pts',(0.985600426557816,-0.33909093068465,
1.31521005565926));
#17339=CARTESIAN_POINT('Ctrl Pts',(1.03253285680459,-0.373586846396559,
1.27866649102984));
#17340=CARTESIAN_POINT('Ctrl Pts',(1.05871835910697,-0.388086240756494,
1.25722555095714));
#17341=CARTESIAN_POINT('Ctrl Pts',(1.11153475808518,-0.407068917407805,
1.2107812086231));
#17342=CARTESIAN_POINT('Ctrl Pts',(1.13814686046673,-0.411552957311693,
1.18575674747573));
#17343=CARTESIAN_POINT('Ctrl Pts',(1.18575674747573,-0.411552957311693,
1.13814686046673));
#17344=CARTESIAN_POINT('Ctrl Pts',(1.2107812086231,-0.407068917407805,1.11153475808518));
#17345=CARTESIAN_POINT('Ctrl Pts',(1.25722555095713,-0.388086240756494,
1.05871835910697));
#17346=CARTESIAN_POINT('Ctrl Pts',(1.27866649102984,-0.373586846396559,
1.03253285680459));
#17347=CARTESIAN_POINT('Ctrl Pts',(1.31521005565926,-0.33909093068465,0.985600426557816));
#17348=CARTESIAN_POINT('Ctrl Pts',(1.33211611256184,-0.317195968905306,
0.962485392528369));
#17349=CARTESIAN_POINT('Ctrl Pts',(1.36127834356734,-0.266264900654909,
0.920778333482565));
#17350=CARTESIAN_POINT('Ctrl Pts',(1.3735491215176,-0.237231147975234,0.902193646979983));
#17351=CARTESIAN_POINT('Ctrl Pts',(1.39550172959303,-0.166543350814306,
0.867957148219442));
#17352=CARTESIAN_POINT('Ctrl Pts',(1.40380622184538,-0.123401821157026,
0.854205272175555));
#17353=CARTESIAN_POINT('Ctrl Pts',(1.40825612658882,-0.0793800000000001,
0.846804978391753));
#17354=CARTESIAN_POINT('',(0.886256117232623,-0.07938,1.45861320581289));
#17355=CARTESIAN_POINT('Origin',(1.18440385848747,-0.07938,1.18440385848747));
#17356=CARTESIAN_POINT('',(1.45861320581289,-0.07938,0.886256117232624));
#17357=CARTESIAN_POINT('Ctrl Pts',(1.45861320581289,-0.0793800000000001,
0.886256117232623));
#17358=CARTESIAN_POINT('Ctrl Pts',(1.45630208793976,-0.101649918886749,
0.890059788636852));
#17359=CARTESIAN_POINT('Ctrl Pts',(1.45296717977858,-0.123823518623746,
0.895520212222107));
#17360=CARTESIAN_POINT('Ctrl Pts',(1.43904931717599,-0.192480977588836,
0.917859913453975));
#17361=CARTESIAN_POINT('Ctrl Pts',(1.4243271592157,-0.236152929235938,0.940896403863072));
#17362=CARTESIAN_POINT('Ctrl Pts',(1.39055359345152,-0.303141259068212,
0.990027513266106));
#17363=CARTESIAN_POINT('Ctrl Pts',(1.36743459453896,-0.335108247315849,
1.02199477007745));
#17364=CARTESIAN_POINT('Ctrl Pts',(1.32643091652006,-0.373243761060364,
1.07446535104584));
#17365=CARTESIAN_POINT('Ctrl Pts',(1.30441816675528,-0.387888272594439,
1.10126842659597));
#17366=CARTESIAN_POINT('Ctrl Pts',(1.25681160160691,-0.407041111792943,
1.15530234155453));
#17367=CARTESIAN_POINT('Ctrl Pts',(1.23119764287622,-0.411552957311693,
1.18251418313119));
#17368=CARTESIAN_POINT('Ctrl Pts',(1.18251418313119,-0.411552957311693,
1.23119764287622));
#17369=CARTESIAN_POINT('Ctrl Pts',(1.15530234155453,-0.407041111792943,
1.25681160160691));
#17370=CARTESIAN_POINT('Ctrl Pts',(1.10126842659597,-0.387888272594439,
1.30441816675528));
#17371=CARTESIAN_POINT('Ctrl Pts',(1.07446535104584,-0.373243761060364,
1.32643091652006));
#17372=CARTESIAN_POINT('Ctrl Pts',(1.02199477007745,-0.335108247315848,
1.36743459453896));
#17373=CARTESIAN_POINT('Ctrl Pts',(0.990027513266105,-0.303141259068211,
1.39055359345152));
#17374=CARTESIAN_POINT('Ctrl Pts',(0.940896403863071,-0.236152929235937,
1.42432715921571));
#17375=CARTESIAN_POINT('Ctrl Pts',(0.917859913453974,-0.192480977588835,
1.43904931717599));
#17376=CARTESIAN_POINT('Ctrl Pts',(0.895520212222106,-0.123823518623745,
1.45296717977858));
#17377=CARTESIAN_POINT('Ctrl Pts',(0.890059788636851,-0.101649918886749,
1.45630208793976));
#17378=CARTESIAN_POINT('Ctrl Pts',(0.886256117232622,-0.0793800000000001,
1.45861320581289));
#17379=CARTESIAN_POINT('Origin',(1.18440385848747,-0.07938,1.18440385848747));
#17380=CARTESIAN_POINT('Origin',(0.,-0.27783,0.));
#17381=CARTESIAN_POINT('',(0.404717578595295,-0.07938,1.65807299932179));
#17382=CARTESIAN_POINT('Origin',(0.,-0.07938,0.));
#17383=CARTESIAN_POINT('',(-0.404717578595296,-0.07938,1.65807299932179));
#17384=CARTESIAN_POINT('Ctrl Pts',(0.404717578595296,-0.0793800000000001,
1.65807299932179));
#17385=CARTESIAN_POINT('Ctrl Pts',(0.400393769631747,-0.101649918886749,
1.65912839404491));
#17386=CARTESIAN_POINT('Ctrl Pts',(0.394174530911058,-0.123823518623745,
1.66063136041479));
#17387=CARTESIAN_POINT('Ctrl Pts',(0.368536561654407,-0.192480977588835,
1.66658649961961));
#17388=CARTESIAN_POINT('Ctrl Pts',(0.341837165343982,-0.236152929235937,
1.67246562047521));
#17389=CARTESIAN_POINT('Ctrl Pts',(0.283214707341173,-0.303141259068211,
1.68332504372461));
#17390=CARTESIAN_POINT('Ctrl Pts',(0.244262842368623,-0.335108247315849,
1.68958170688653));
#17391=CARTESIAN_POINT('Ctrl Pts',(0.178166559972324,-0.373243761060364,
1.69769003172132));
#17392=CARTESIAN_POINT('Ctrl Pts',(0.143648558862931,-0.387888272594439,
1.70107730356824));
#17393=CARTESIAN_POINT('Ctrl Pts',(0.0717778861362652,-0.407041111792943,
1.70562212620408));
#17394=CARTESIAN_POINT('Ctrl Pts',(0.0344244045173309,-0.411552957311693,
1.706752));
#17395=CARTESIAN_POINT('Ctrl Pts',(-0.0344244045173315,-0.411552957311693,
1.706752));
#17396=CARTESIAN_POINT('Ctrl Pts',(-0.0717778861362658,-0.407041111792943,
1.70562212620408));
#17397=CARTESIAN_POINT('Ctrl Pts',(-0.143648558862932,-0.387888272594439,
1.70107730356824));
#17398=CARTESIAN_POINT('Ctrl Pts',(-0.178166559972325,-0.373243761060364,
1.69769003172132));
#17399=CARTESIAN_POINT('Ctrl Pts',(-0.244262842368624,-0.335108247315849,
1.68958170688653));
#17400=CARTESIAN_POINT('Ctrl Pts',(-0.283214707341173,-0.303141259068212,
1.68332504372461));
#17401=CARTESIAN_POINT('Ctrl Pts',(-0.341837165343982,-0.236152929235937,
1.67246562047521));
#17402=CARTESIAN_POINT('Ctrl Pts',(-0.368536561654408,-0.192480977588835,
1.66658649961961));
#17403=CARTESIAN_POINT('Ctrl Pts',(-0.394174530911059,-0.123823518623745,
1.66063136041479));
#17404=CARTESIAN_POINT('Ctrl Pts',(-0.400393769631748,-0.101649918886749,
1.65912839404491));
#17405=CARTESIAN_POINT('Ctrl Pts',(-0.404717578595297,-0.0793800000000001,
1.65807299932179));
#17406=CARTESIAN_POINT('',(-0.886256117232624,-0.07938,1.45861320581289));
#17407=CARTESIAN_POINT('Origin',(0.,-0.07938,0.));
#17408=CARTESIAN_POINT('',(-1.45861320581289,-0.07938,0.886256117232623));
#17409=CARTESIAN_POINT('Ctrl Pts',(-0.886256117232623,-0.0793800000000001,
1.45861320581289));
#17410=CARTESIAN_POINT('Ctrl Pts',(-0.890059788636852,-0.101649918886749,
1.45630208793976));
#17411=CARTESIAN_POINT('Ctrl Pts',(-0.895520212222106,-0.123823518623745,
1.45296717977858));
#17412=CARTESIAN_POINT('Ctrl Pts',(-0.917859913453974,-0.192480977588835,
1.43904931717599));
#17413=CARTESIAN_POINT('Ctrl Pts',(-0.940896403863071,-0.236152929235937,
1.4243271592157));
#17414=CARTESIAN_POINT('Ctrl Pts',(-0.990027513266105,-0.303141259068211,
1.39055359345152));
#17415=CARTESIAN_POINT('Ctrl Pts',(-1.02199477007745,-0.335108247315848,
1.36743459453896));
#17416=CARTESIAN_POINT('Ctrl Pts',(-1.07446535104584,-0.373243761060364,
1.32643091652006));
#17417=CARTESIAN_POINT('Ctrl Pts',(-1.10126842659597,-0.387888272594439,
1.30441816675528));
#17418=CARTESIAN_POINT('Ctrl Pts',(-1.15530234155453,-0.407041111792943,
1.25681160160691));
#17419=CARTESIAN_POINT('Ctrl Pts',(-1.18251418313119,-0.411552957311693,
1.23119764287622));
#17420=CARTESIAN_POINT('Ctrl Pts',(-1.23119764287622,-0.411552957311693,
1.18251418313119));
#17421=CARTESIAN_POINT('Ctrl Pts',(-1.25681160160691,-0.407041111792943,
1.15530234155453));
#17422=CARTESIAN_POINT('Ctrl Pts',(-1.30441816675528,-0.387888272594439,
1.10126842659597));
#17423=CARTESIAN_POINT('Ctrl Pts',(-1.32643091652006,-0.373243761060365,
1.07446535104584));
#17424=CARTESIAN_POINT('Ctrl Pts',(-1.36743459453896,-0.335108247315849,
1.02199477007745));
#17425=CARTESIAN_POINT('Ctrl Pts',(-1.39055359345152,-0.303141259068212,
0.990027513266106));
#17426=CARTESIAN_POINT('Ctrl Pts',(-1.4243271592157,-0.236152929235938,
0.940896403863071));
#17427=CARTESIAN_POINT('Ctrl Pts',(-1.43904931717599,-0.192480977588836,
0.917859913453974));
#17428=CARTESIAN_POINT('Ctrl Pts',(-1.45296717977858,-0.123823518623746,
0.895520212222106));
#17429=CARTESIAN_POINT('Ctrl Pts',(-1.45630208793976,-0.101649918886749,
0.890059788636852));
#17430=CARTESIAN_POINT('Ctrl Pts',(-1.45861320581289,-0.0793800000000001,
0.886256117232623));
#17431=CARTESIAN_POINT('',(-1.65807299932179,-0.07938,0.404717578595295));
#17432=CARTESIAN_POINT('Origin',(0.,-0.07938,0.));
#17433=CARTESIAN_POINT('',(-1.706752,-0.411552957311693,2.08591827245526E-16));
#17434=CARTESIAN_POINT('Ctrl Pts',(-1.65807299932179,-0.0793800000000001,
0.404717578595296));
#17435=CARTESIAN_POINT('Ctrl Pts',(-1.65912839404491,-0.101649918886749,
0.400393769631747));
#17436=CARTESIAN_POINT('Ctrl Pts',(-1.66063136041479,-0.123823518623745,
0.394174530911058));
#17437=CARTESIAN_POINT('Ctrl Pts',(-1.66658649961961,-0.192480977588835,
0.368536561654407));
#17438=CARTESIAN_POINT('Ctrl Pts',(-1.67246562047521,-0.236152929235937,
0.341837165343982));
#17439=CARTESIAN_POINT('Ctrl Pts',(-1.68332504372461,-0.303141259068211,
0.283214707341173));
#17440=CARTESIAN_POINT('Ctrl Pts',(-1.68958170688653,-0.335108247315848,
0.244262842368623));
#17441=CARTESIAN_POINT('Ctrl Pts',(-1.69769003172132,-0.373243761060364,
0.178166559972324));
#17442=CARTESIAN_POINT('Ctrl Pts',(-1.70107730356824,-0.387888272594439,
0.143648558862931));
#17443=CARTESIAN_POINT('Ctrl Pts',(-1.70562212620408,-0.407041111792943,
0.0717778861362656));
#17444=CARTESIAN_POINT('Ctrl Pts',(-1.706752,-0.411552957311693,0.0344244045173313));
#17445=CARTESIAN_POINT('Ctrl Pts',(-1.706752,-0.411552957311693,2.08166817117217E-16));
#17446=CARTESIAN_POINT('',(-1.706752,-0.47628,2.09016837373834E-16));
#17447=CARTESIAN_POINT('',(-1.706752,-0.27783,2.09016837373834E-16));
#17448=CARTESIAN_POINT('Origin',(0.,-0.47628,0.));
#17449=CARTESIAN_POINT('',(-1.65807299932179,-0.07938,-0.404717578595296));
#17450=CARTESIAN_POINT('Ctrl Pts',(-1.706752,-0.411552957311693,2.0122792321331E-16));
#17451=CARTESIAN_POINT('Ctrl Pts',(-1.706752,-0.411552957311693,-0.0344244045173309));
#17452=CARTESIAN_POINT('Ctrl Pts',(-1.70562212620408,-0.407041111792943,
-0.0717778861362652));
#17453=CARTESIAN_POINT('Ctrl Pts',(-1.70107730356824,-0.387888272594439,
-0.143648558862931));
#17454=CARTESIAN_POINT('Ctrl Pts',(-1.69769003172132,-0.373243761060365,
-0.178166559972324));
#17455=CARTESIAN_POINT('Ctrl Pts',(-1.68958170688653,-0.335108247315849,
-0.244262842368623));
#17456=CARTESIAN_POINT('Ctrl Pts',(-1.68332504372461,-0.303141259068212,
-0.283214707341173));
#17457=CARTESIAN_POINT('Ctrl Pts',(-1.67246562047521,-0.236152929235938,
-0.341837165343982));
#17458=CARTESIAN_POINT('Ctrl Pts',(-1.66658649961961,-0.192480977588836,
-0.368536561654407));
#17459=CARTESIAN_POINT('Ctrl Pts',(-1.66063136041479,-0.123823518623745,
-0.394174530911059));
#17460=CARTESIAN_POINT('Ctrl Pts',(-1.65912839404491,-0.101649918886749,
-0.400393769631748));
#17461=CARTESIAN_POINT('Ctrl Pts',(-1.65807299932179,-0.0793800000000001,
-0.404717578595296));
#17462=CARTESIAN_POINT('',(-1.45861320581289,-0.07938,-0.886256117232623));
#17463=CARTESIAN_POINT('Origin',(0.,-0.07938,0.));
#17464=CARTESIAN_POINT('',(-0.886256117232623,-0.07938,-1.45861320581289));
#17465=CARTESIAN_POINT('Ctrl Pts',(-1.45861320581289,-0.0793800000000001,
-0.886256117232623));
#17466=CARTESIAN_POINT('Ctrl Pts',(-1.45630208793976,-0.101649918886749,
-0.890059788636852));
#17467=CARTESIAN_POINT('Ctrl Pts',(-1.45296717977858,-0.123823518623745,
-0.895520212222106));
#17468=CARTESIAN_POINT('Ctrl Pts',(-1.43904931717599,-0.192480977588835,
-0.917859913453974));
#17469=CARTESIAN_POINT('Ctrl Pts',(-1.4243271592157,-0.236152929235937,
-0.940896403863072));
#17470=CARTESIAN_POINT('Ctrl Pts',(-1.39055359345152,-0.303141259068212,
-0.990027513266106));
#17471=CARTESIAN_POINT('Ctrl Pts',(-1.36743459453896,-0.335108247315849,
-1.02199477007745));
#17472=CARTESIAN_POINT('Ctrl Pts',(-1.32643091652006,-0.373243761060364,
-1.07446535104584));
#17473=CARTESIAN_POINT('Ctrl Pts',(-1.30441816675528,-0.387888272594439,
-1.10126842659597));
#17474=CARTESIAN_POINT('Ctrl Pts',(-1.25681160160691,-0.407041111792943,
-1.15530234155453));
#17475=CARTESIAN_POINT('Ctrl Pts',(-1.23119764287622,-0.411552957311693,
-1.18251418313119));
#17476=CARTESIAN_POINT('Ctrl Pts',(-1.18251418313119,-0.411552957311693,
-1.23119764287622));
#17477=CARTESIAN_POINT('Ctrl Pts',(-1.15530234155453,-0.407041111792943,
-1.25681160160691));
#17478=CARTESIAN_POINT('Ctrl Pts',(-1.10126842659597,-0.387888272594439,
-1.30441816675528));
#17479=CARTESIAN_POINT('Ctrl Pts',(-1.07446535104584,-0.373243761060364,
-1.32643091652006));
#17480=CARTESIAN_POINT('Ctrl Pts',(-1.02199477007745,-0.335108247315848,
-1.36743459453896));
#17481=CARTESIAN_POINT('Ctrl Pts',(-0.990027513266105,-0.303141259068211,
-1.39055359345152));
#17482=CARTESIAN_POINT('Ctrl Pts',(-0.940896403863071,-0.236152929235936,
-1.42432715921571));
#17483=CARTESIAN_POINT('Ctrl Pts',(-0.917859913453974,-0.192480977588835,
-1.43904931717599));
#17484=CARTESIAN_POINT('Ctrl Pts',(-0.895520212222106,-0.123823518623745,
-1.45296717977858));
#17485=CARTESIAN_POINT('Ctrl Pts',(-0.890059788636851,-0.101649918886749,
-1.45630208793976));
#17486=CARTESIAN_POINT('Ctrl Pts',(-0.886256117232623,-0.0793800000000001,
-1.45861320581289));
#17487=CARTESIAN_POINT('',(-0.404717578595295,-0.07938,-1.65807299932179));
#17488=CARTESIAN_POINT('Origin',(0.,-0.07938,0.));
#17489=CARTESIAN_POINT('',(0.404717578595296,-0.07938,-1.65807299932179));
#17490=CARTESIAN_POINT('Ctrl Pts',(-0.404717578595296,-0.0793800000000001,
-1.65807299932179));
#17491=CARTESIAN_POINT('Ctrl Pts',(-0.400393769631747,-0.101649918886749,
-1.65912839404491));
#17492=CARTESIAN_POINT('Ctrl Pts',(-0.394174530911058,-0.123823518623746,
-1.66063136041479));
#17493=CARTESIAN_POINT('Ctrl Pts',(-0.368536561654407,-0.192480977588836,
-1.66658649961961));
#17494=CARTESIAN_POINT('Ctrl Pts',(-0.341837165343982,-0.236152929235938,
-1.67246562047521));
#17495=CARTESIAN_POINT('Ctrl Pts',(-0.283214707341173,-0.303141259068212,
-1.68332504372461));
#17496=CARTESIAN_POINT('Ctrl Pts',(-0.244262842368623,-0.335108247315849,
-1.68958170688653));
#17497=CARTESIAN_POINT('Ctrl Pts',(-0.178166559972324,-0.373243761060364,
-1.69769003172132));
#17498=CARTESIAN_POINT('Ctrl Pts',(-0.143648558862931,-0.387888272594439,
-1.70107730356824));
#17499=CARTESIAN_POINT('Ctrl Pts',(-0.0717778861362653,-0.407041111792943,
-1.70562212620408));
#17500=CARTESIAN_POINT('Ctrl Pts',(-0.034424404517331,-0.411552957311693,
-1.706752));
#17501=CARTESIAN_POINT('Ctrl Pts',(0.0344244045173312,-0.411552957311693,
-1.706752));
#17502=CARTESIAN_POINT('Ctrl Pts',(0.0717778861362655,-0.407041111792943,
-1.70562212620408));
#17503=CARTESIAN_POINT('Ctrl Pts',(0.143648558862931,-0.387888272594439,
-1.70107730356824));
#17504=CARTESIAN_POINT('Ctrl Pts',(0.178166559972324,-0.373243761060364,
-1.69769003172132));
#17505=CARTESIAN_POINT('Ctrl Pts',(0.244262842368623,-0.335108247315849,
-1.68958170688653));
#17506=CARTESIAN_POINT('Ctrl Pts',(0.283214707341173,-0.303141259068212,
-1.68332504372461));
#17507=CARTESIAN_POINT('Ctrl Pts',(0.341837165343982,-0.236152929235937,
-1.67246562047521));
#17508=CARTESIAN_POINT('Ctrl Pts',(0.368536561654407,-0.192480977588835,
-1.66658649961961));
#17509=CARTESIAN_POINT('Ctrl Pts',(0.394174530911059,-0.123823518623745,
-1.66063136041479));
#17510=CARTESIAN_POINT('Ctrl Pts',(0.400393769631748,-0.101649918886749,
-1.65912839404491));
#17511=CARTESIAN_POINT('Ctrl Pts',(0.404717578595296,-0.0793800000000001,
-1.65807299932179));
#17512=CARTESIAN_POINT('',(0.886256117232623,-0.07938,-1.45861320581289));
#17513=CARTESIAN_POINT('Origin',(0.,-0.07938,0.));
#17514=CARTESIAN_POINT('',(1.45861320581289,-0.07938,-0.886256117232623));
#17515=CARTESIAN_POINT('Ctrl Pts',(0.886256117232623,-0.0793800000000001,
-1.45861320581289));
#17516=CARTESIAN_POINT('Ctrl Pts',(0.890059788636852,-0.101649918886749,
-1.45630208793976));
#17517=CARTESIAN_POINT('Ctrl Pts',(0.895520212222106,-0.123823518623745,
-1.45296717977858));
#17518=CARTESIAN_POINT('Ctrl Pts',(0.917859913453974,-0.192480977588835,
-1.43904931717599));
#17519=CARTESIAN_POINT('Ctrl Pts',(0.940896403863072,-0.236152929235937,
-1.4243271592157));
#17520=CARTESIAN_POINT('Ctrl Pts',(0.990027513266106,-0.303141259068211,
-1.39055359345152));
#17521=CARTESIAN_POINT('Ctrl Pts',(1.02199477007745,-0.335108247315849,
-1.36743459453896));
#17522=CARTESIAN_POINT('Ctrl Pts',(1.07446535104584,-0.373243761060364,
-1.32643091652006));
#17523=CARTESIAN_POINT('Ctrl Pts',(1.10126842659597,-0.387888272594439,
-1.30441816675528));
#17524=CARTESIAN_POINT('Ctrl Pts',(1.15530234155453,-0.407041111792943,
-1.25681160160691));
#17525=CARTESIAN_POINT('Ctrl Pts',(1.18251418313119,-0.411552957311693,
-1.23119764287622));
#17526=CARTESIAN_POINT('Ctrl Pts',(1.23119764287622,-0.411552957311693,
-1.18251418313119));
#17527=CARTESIAN_POINT('Ctrl Pts',(1.25681160160691,-0.407041111792943,
-1.15530234155453));
#17528=CARTESIAN_POINT('Ctrl Pts',(1.30441816675528,-0.387888272594439,
-1.10126842659597));
#17529=CARTESIAN_POINT('Ctrl Pts',(1.32643091652006,-0.373243761060364,
-1.07446535104584));
#17530=CARTESIAN_POINT('Ctrl Pts',(1.36743459453896,-0.335108247315849,
-1.02199477007745));
#17531=CARTESIAN_POINT('Ctrl Pts',(1.39055359345152,-0.303141259068212,
-0.990027513266105));
#17532=CARTESIAN_POINT('Ctrl Pts',(1.4243271592157,-0.236152929235937,-0.940896403863071));
#17533=CARTESIAN_POINT('Ctrl Pts',(1.43904931717599,-0.192480977588835,
-0.917859913453974));
#17534=CARTESIAN_POINT('Ctrl Pts',(1.45296717977858,-0.123823518623745,
-0.895520212222106));
#17535=CARTESIAN_POINT('Ctrl Pts',(1.45630208793976,-0.101649918886749,
-0.890059788636852));
#17536=CARTESIAN_POINT('Ctrl Pts',(1.45861320581289,-0.0793800000000001,
-0.886256117232623));
#17537=CARTESIAN_POINT('',(1.65807299932179,-0.07938,-0.404717578595296));
#17538=CARTESIAN_POINT('Origin',(0.,-0.07938,0.));
#17539=CARTESIAN_POINT('',(1.65807299932179,-0.07938,0.404717578595296));
#17540=CARTESIAN_POINT('Ctrl Pts',(1.65807299932179,-0.0793800000000001,
-0.404717578595296));
#17541=CARTESIAN_POINT('Ctrl Pts',(1.65912839404491,-0.101649918886749,
-0.400393769631747));
#17542=CARTESIAN_POINT('Ctrl Pts',(1.66063136041479,-0.123823518623745,
-0.394174530911058));
#17543=CARTESIAN_POINT('Ctrl Pts',(1.66658649961961,-0.192480977588835,
-0.368536561654407));
#17544=CARTESIAN_POINT('Ctrl Pts',(1.67246562047521,-0.236152929235937,
-0.341837165343982));
#17545=CARTESIAN_POINT('Ctrl Pts',(1.68332504372461,-0.303141259068212,
-0.283214707341173));
#17546=CARTESIAN_POINT('Ctrl Pts',(1.68958170688653,-0.335108247315849,
-0.244262842368623));
#17547=CARTESIAN_POINT('Ctrl Pts',(1.69769003172132,-0.373243761060364,
-0.178166559972324));
#17548=CARTESIAN_POINT('Ctrl Pts',(1.70107730356824,-0.387888272594439,
-0.143648558862931));
#17549=CARTESIAN_POINT('Ctrl Pts',(1.70562212620408,-0.407041111792943,
-0.0717778861362655));
#17550=CARTESIAN_POINT('Ctrl Pts',(1.706752,-0.411552957311693,-0.0344244045173312));
#17551=CARTESIAN_POINT('Ctrl Pts',(1.706752,-0.411552957311693,0.0344244045173312));
#17552=CARTESIAN_POINT('Ctrl Pts',(1.70562212620408,-0.407041111792943,
0.0717778861362655));
#17553=CARTESIAN_POINT('Ctrl Pts',(1.70107730356824,-0.387888272594439,
0.143648558862931));
#17554=CARTESIAN_POINT('Ctrl Pts',(1.69769003172132,-0.373243761060364,
0.178166559972324));
#17555=CARTESIAN_POINT('Ctrl Pts',(1.68958170688653,-0.335108247315849,
0.244262842368623));
#17556=CARTESIAN_POINT('Ctrl Pts',(1.68332504372461,-0.303141259068212,
0.283214707341173));
#17557=CARTESIAN_POINT('Ctrl Pts',(1.67246562047521,-0.236152929235937,
0.341837165343982));
#17558=CARTESIAN_POINT('Ctrl Pts',(1.66658649961961,-0.192480977588835,
0.368536561654407));
#17559=CARTESIAN_POINT('Ctrl Pts',(1.66063136041479,-0.123823518623745,
0.394174530911058));
#17560=CARTESIAN_POINT('Ctrl Pts',(1.65912839404491,-0.101649918886749,
0.400393769631747));
#17561=CARTESIAN_POINT('Ctrl Pts',(1.65807299932179,-0.0793800000000001,
0.404717578595296));
#17562=CARTESIAN_POINT('Origin',(0.,-0.07938,0.));
#17563=CARTESIAN_POINT('Origin',(0.,-0.07938,0.));
#17564=CARTESIAN_POINT('',(0.397005914195118,-0.07938,1.59456899932179));
#17565=CARTESIAN_POINT('Origin',(0.,-0.07938,0.));
#17566=CARTESIAN_POINT('Origin',(-3.33066907387547E-16,-0.07938,1.675));
#17567=CARTESIAN_POINT('Origin',(-3.33066907387547E-16,0.,1.675));
#17568=CARTESIAN_POINT('',(-0.397005914195118,-0.07938,1.59456899932179));
#17569=CARTESIAN_POINT('Ctrl Pts',(-0.397005914195119,-0.0793800000000001,
1.59456899932179));
#17570=CARTESIAN_POINT('Ctrl Pts',(-0.3886265584581,-0.123401821157026,
1.59665523941937));
#17571=CARTESIAN_POINT('Ctrl Pts',(-0.373030350867485,-0.166543350814306,
1.60050712143809));
#17572=CARTESIAN_POINT('Ctrl Pts',(-0.333298652394954,-0.237231147975234,
1.60919314384089));
#17573=CARTESIAN_POINT('Ctrl Pts',(-0.311480544243687,-0.266264900654909,
1.61365775139403));
#17574=CARTESIAN_POINT('Ctrl Pts',(-0.261368388670537,-0.317195968905306,
1.62252828437015));
#17575=CARTESIAN_POINT('Ctrl Pts',(-0.233069203882014,-0.33909093068465,
1.62691869420078));
#17576=CARTESIAN_POINT('Ctrl Pts',(-0.174042761838764,-0.373586846396559,
1.63426473152765));
#17577=CARTESIAN_POINT('Ctrl Pts',(-0.14036578147155,-0.388086240756494,
1.63761964365402));
#17578=CARTESIAN_POINT('Ctrl Pts',(-0.0701778381840615,-0.407068917407805,
1.64212536811722));
#17579=CARTESIAN_POINT('Ctrl Pts',(-0.0336652739555918,-0.411552957311693,
1.643248));
#17580=CARTESIAN_POINT('Ctrl Pts',(0.0336652739555913,-0.411552957311693,
1.643248));
#17581=CARTESIAN_POINT('Ctrl Pts',(0.070177838184061,-0.407068917407805,
1.64212536811722));
#17582=CARTESIAN_POINT('Ctrl Pts',(0.140365781471549,-0.388086240756494,
1.63761964365402));
#17583=CARTESIAN_POINT('Ctrl Pts',(0.174042761838763,-0.373586846396559,
1.63426473152765));
#17584=CARTESIAN_POINT('Ctrl Pts',(0.233069203882014,-0.33909093068465,
1.62691869420078));
#17585=CARTESIAN_POINT('Ctrl Pts',(0.261368388670536,-0.317195968905306,
1.62252828437015));
#17586=CARTESIAN_POINT('Ctrl Pts',(0.311480544243686,-0.266264900654908,
1.61365775139403));
#17587=CARTESIAN_POINT('Ctrl Pts',(0.333298652394954,-0.237231147975234,
1.60919314384089));
#17588=CARTESIAN_POINT('Ctrl Pts',(0.373030350867484,-0.166543350814306,
1.60050712143809));
#17589=CARTESIAN_POINT('Ctrl Pts',(0.388626558458099,-0.123401821157026,
1.59665523941937));
#17590=CARTESIAN_POINT('Ctrl Pts',(0.397005914195118,-0.07938,1.59456899932179));
#17591=CARTESIAN_POINT('Origin',(-3.33066907387547E-16,-0.07938,1.675));
#17592=CARTESIAN_POINT('Origin',(0.,-0.07938,0.));
#17593=CARTESIAN_POINT('',(-0.846804978391754,-0.07938,1.40825612658882));
#17594=CARTESIAN_POINT('Origin',(0.,-0.07938,0.));
#17595=CARTESIAN_POINT('Origin',(-1.18440385848747,-0.07938,1.18440385848747));
#17596=CARTESIAN_POINT('Origin',(-1.18440385848747,0.,1.18440385848747));
#17597=CARTESIAN_POINT('',(-1.40825612658882,-0.07938,0.846804978391753));
#17598=CARTESIAN_POINT('Ctrl Pts',(-1.40825612658882,-0.0793800000000001,
0.846804978391753));
#17599=CARTESIAN_POINT('Ctrl Pts',(-1.40380622184538,-0.123401821157026,
0.854205272175555));
#17600=CARTESIAN_POINT('Ctrl Pts',(-1.39550172959303,-0.166543350814306,
0.867957148219442));
#17601=CARTESIAN_POINT('Ctrl Pts',(-1.3735491215176,-0.237231147975235,
0.902193646979983));
#17602=CARTESIAN_POINT('Ctrl Pts',(-1.36127834356734,-0.266264900654909,
0.920778333482565));
#17603=CARTESIAN_POINT('Ctrl Pts',(-1.33211611256184,-0.317195968905306,
0.962485392528369));
#17604=CARTESIAN_POINT('Ctrl Pts',(-1.31521005565926,-0.339090930684651,
0.985600426557816));
#17605=CARTESIAN_POINT('Ctrl Pts',(-1.27866649102984,-0.373586846396559,
1.03253285680459));
#17606=CARTESIAN_POINT('Ctrl Pts',(-1.25722555095714,-0.388086240756494,
1.05871835910697));
#17607=CARTESIAN_POINT('Ctrl Pts',(-1.2107812086231,-0.407068917407805,
1.11153475808518));
#17608=CARTESIAN_POINT('Ctrl Pts',(-1.18575674747573,-0.411552957311693,
1.13814686046673));
#17609=CARTESIAN_POINT('Ctrl Pts',(-1.13814686046673,-0.411552957311693,
1.18575674747573));
#17610=CARTESIAN_POINT('Ctrl Pts',(-1.11153475808518,-0.407068917407805,
1.2107812086231));
#17611=CARTESIAN_POINT('Ctrl Pts',(-1.05871835910697,-0.388086240756494,
1.25722555095714));
#17612=CARTESIAN_POINT('Ctrl Pts',(-1.03253285680459,-0.373586846396559,
1.27866649102984));
#17613=CARTESIAN_POINT('Ctrl Pts',(-0.985600426557816,-0.33909093068465,
1.31521005565926));
#17614=CARTESIAN_POINT('Ctrl Pts',(-0.962485392528369,-0.317195968905306,
1.33211611256184));
#17615=CARTESIAN_POINT('Ctrl Pts',(-0.920778333482565,-0.266264900654908,
1.36127834356734));
#17616=CARTESIAN_POINT('Ctrl Pts',(-0.902193646979983,-0.237231147975234,
1.3735491215176));
#17617=CARTESIAN_POINT('Ctrl Pts',(-0.867957148219442,-0.166543350814306,
1.39550172959303));
#17618=CARTESIAN_POINT('Ctrl Pts',(-0.854205272175555,-0.123401821157026,
1.40380622184538));
#17619=CARTESIAN_POINT('Ctrl Pts',(-0.846804978391753,-0.0793800000000001,
1.40825612658882));
#17620=CARTESIAN_POINT('Origin',(-1.18440385848747,-0.07938,1.18440385848747));
#17621=CARTESIAN_POINT('Origin',(0.,-0.07938,0.));
#17622=CARTESIAN_POINT('',(-1.59456899932179,-0.07938,0.397005914195118));
#17623=CARTESIAN_POINT('Origin',(0.,-0.07938,0.));
#17624=CARTESIAN_POINT('Origin',(-1.675,-0.07938,-2.22044604925031E-16));
#17625=CARTESIAN_POINT('Origin',(-1.675,0.,-2.22044604925031E-16));
#17626=CARTESIAN_POINT('',(-1.59456899932179,-0.07938,-0.397005914195118));
#17627=CARTESIAN_POINT('',(-1.643248,-0.411552957311693,3.47540551556327E-18));
#17628=CARTESIAN_POINT('Ctrl Pts',(-1.59456899932179,-0.0793800000000001,
-0.397005914195119));
#17629=CARTESIAN_POINT('Ctrl Pts',(-1.59665523941937,-0.123401821157026,
-0.388626558458099));
#17630=CARTESIAN_POINT('Ctrl Pts',(-1.60050712143809,-0.166543350814306,
-0.373030350867485));
#17631=CARTESIAN_POINT('Ctrl Pts',(-1.60919314384089,-0.237231147975234,
-0.333298652394954));
#17632=CARTESIAN_POINT('Ctrl Pts',(-1.61365775139403,-0.266264900654909,
-0.311480544243686));
#17633=CARTESIAN_POINT('Ctrl Pts',(-1.62252828437015,-0.317195968905306,
-0.261368388670537));
#17634=CARTESIAN_POINT('Ctrl Pts',(-1.62691869420078,-0.33909093068465,
-0.233069203882014));
#17635=CARTESIAN_POINT('Ctrl Pts',(-1.63426473152765,-0.373586846396559,
-0.174042761838764));
#17636=CARTESIAN_POINT('Ctrl Pts',(-1.63761964365402,-0.388086240756494,
-0.140365781471549));
#17637=CARTESIAN_POINT('Ctrl Pts',(-1.64212536811722,-0.407068917407805,
-0.0701778381840614));
#17638=CARTESIAN_POINT('Ctrl Pts',(-1.643248,-0.411552957311693,-0.0336652739555917));
#17639=CARTESIAN_POINT('Ctrl Pts',(-1.643248,-0.411552957311693,-2.0122792321331E-16));
#17640=CARTESIAN_POINT('Origin',(-1.675,-0.07938,-2.22044604925031E-16));
#17641=CARTESIAN_POINT('Ctrl Pts',(-1.643248,-0.411552957311693,-1.94289029309402E-16));
#17642=CARTESIAN_POINT('Ctrl Pts',(-1.643248,-0.411552957311693,0.0336652739555913));
#17643=CARTESIAN_POINT('Ctrl Pts',(-1.64212536811722,-0.407068917407805,
0.0701778381840609));
#17644=CARTESIAN_POINT('Ctrl Pts',(-1.63761964365402,-0.388086240756494,
0.140365781471549));
#17645=CARTESIAN_POINT('Ctrl Pts',(-1.63426473152765,-0.373586846396559,
0.174042761838763));
#17646=CARTESIAN_POINT('Ctrl Pts',(-1.62691869420078,-0.33909093068465,
0.233069203882014));
#17647=CARTESIAN_POINT('Ctrl Pts',(-1.62252828437015,-0.317195968905306,
0.261368388670536));
#17648=CARTESIAN_POINT('Ctrl Pts',(-1.61365775139403,-0.266264900654909,
0.311480544243686));
#17649=CARTESIAN_POINT('Ctrl Pts',(-1.60919314384089,-0.237231147975235,
0.333298652394954));
#17650=CARTESIAN_POINT('Ctrl Pts',(-1.60050712143809,-0.166543350814306,
0.373030350867484));
#17651=CARTESIAN_POINT('Ctrl Pts',(-1.59665523941937,-0.123401821157026,
0.388626558458099));
#17652=CARTESIAN_POINT('Ctrl Pts',(-1.59456899932179,-0.0793800000000001,
0.397005914195118));
#17653=CARTESIAN_POINT('Origin',(0.,-0.07938,0.));
#17654=CARTESIAN_POINT('',(-1.40825612658882,-0.07938,-0.846804978391753));
#17655=CARTESIAN_POINT('Origin',(0.,-0.07938,0.));
#17656=CARTESIAN_POINT('Origin',(-1.18440385848747,-0.07938,-1.18440385848747));
#17657=CARTESIAN_POINT('Origin',(-1.18440385848747,0.,-1.18440385848747));
#17658=CARTESIAN_POINT('',(-0.846804978391753,-0.07938,-1.40825612658882));
#17659=CARTESIAN_POINT('Ctrl Pts',(-0.846804978391753,-0.0793800000000001,
-1.40825612658882));
#17660=CARTESIAN_POINT('Ctrl Pts',(-0.854205272175555,-0.123401821157026,
-1.40380622184538));
#17661=CARTESIAN_POINT('Ctrl Pts',(-0.867957148219442,-0.166543350814306,
-1.39550172959303));
#17662=CARTESIAN_POINT('Ctrl Pts',(-0.902193646979982,-0.237231147975234,
-1.3735491215176));
#17663=CARTESIAN_POINT('Ctrl Pts',(-0.920778333482564,-0.266264900654908,
-1.36127834356734));
#17664=CARTESIAN_POINT('Ctrl Pts',(-0.962485392528368,-0.317195968905306,
-1.33211611256184));
#17665=CARTESIAN_POINT('Ctrl Pts',(-0.985600426557816,-0.33909093068465,
-1.31521005565926));
#17666=CARTESIAN_POINT('Ctrl Pts',(-1.03253285680459,-0.373586846396559,
-1.27866649102984));
#17667=CARTESIAN_POINT('Ctrl Pts',(-1.05871835910697,-0.388086240756494,
-1.25722555095714));
#17668=CARTESIAN_POINT('Ctrl Pts',(-1.11153475808518,-0.407068917407805,
-1.2107812086231));
#17669=CARTESIAN_POINT('Ctrl Pts',(-1.13814686046673,-0.411552957311693,
-1.18575674747573));
#17670=CARTESIAN_POINT('Ctrl Pts',(-1.18575674747573,-0.411552957311693,
-1.13814686046673));
#17671=CARTESIAN_POINT('Ctrl Pts',(-1.2107812086231,-0.407068917407805,
-1.11153475808518));
#17672=CARTESIAN_POINT('Ctrl Pts',(-1.25722555095714,-0.388086240756494,
-1.05871835910697));
#17673=CARTESIAN_POINT('Ctrl Pts',(-1.27866649102984,-0.373586846396559,
-1.03253285680459));
#17674=CARTESIAN_POINT('Ctrl Pts',(-1.31521005565926,-0.33909093068465,
-0.985600426557816));
#17675=CARTESIAN_POINT('Ctrl Pts',(-1.33211611256184,-0.317195968905306,
-0.962485392528369));
#17676=CARTESIAN_POINT('Ctrl Pts',(-1.36127834356734,-0.266264900654909,
-0.920778333482565));
#17677=CARTESIAN_POINT('Ctrl Pts',(-1.3735491215176,-0.237231147975234,
-0.902193646979983));
#17678=CARTESIAN_POINT('Ctrl Pts',(-1.39550172959303,-0.166543350814306,
-0.867957148219442));
#17679=CARTESIAN_POINT('Ctrl Pts',(-1.40380622184538,-0.123401821157026,
-0.854205272175555));
#17680=CARTESIAN_POINT('Ctrl Pts',(-1.40825612658882,-0.07938,-0.846804978391753));
#17681=CARTESIAN_POINT('Origin',(-1.18440385848747,-0.07938,-1.18440385848747));
#17682=CARTESIAN_POINT('Origin',(0.,-0.07938,0.));
#17683=CARTESIAN_POINT('',(-0.397005914195118,-0.07938,-1.59456899932179));
#17684=CARTESIAN_POINT('Origin',(0.,-0.07938,0.));
#17685=CARTESIAN_POINT('Origin',(1.11022302462516E-16,-0.07938,-1.675));
#17686=CARTESIAN_POINT('Origin',(1.11022302462516E-16,0.,-1.675));
#17687=CARTESIAN_POINT('',(0.397005914195118,-0.07938,-1.59456899932179));
#17688=CARTESIAN_POINT('Ctrl Pts',(0.397005914195119,-0.0793800000000001,
-1.59456899932179));
#17689=CARTESIAN_POINT('Ctrl Pts',(0.388626558458099,-0.123401821157026,
-1.59665523941937));
#17690=CARTESIAN_POINT('Ctrl Pts',(0.373030350867485,-0.166543350814306,
-1.60050712143809));
#17691=CARTESIAN_POINT('Ctrl Pts',(0.333298652394954,-0.237231147975234,
-1.60919314384089));
#17692=CARTESIAN_POINT('Ctrl Pts',(0.311480544243686,-0.266264900654909,
-1.61365775139403));
#17693=CARTESIAN_POINT('Ctrl Pts',(0.261368388670537,-0.317195968905306,
-1.62252828437015));
#17694=CARTESIAN_POINT('Ctrl Pts',(0.233069203882014,-0.33909093068465,
-1.62691869420078));
#17695=CARTESIAN_POINT('Ctrl Pts',(0.174042761838763,-0.373586846396559,
-1.63426473152765));
#17696=CARTESIAN_POINT('Ctrl Pts',(0.140365781471549,-0.388086240756494,
-1.63761964365402));
#17697=CARTESIAN_POINT('Ctrl Pts',(0.0701778381840612,-0.407068917407805,
-1.64212536811722));
#17698=CARTESIAN_POINT('Ctrl Pts',(0.0336652739555916,-0.411552957311693,
-1.643248));
#17699=CARTESIAN_POINT('Ctrl Pts',(-0.0336652739555915,-0.411552957311693,
-1.643248));
#17700=CARTESIAN_POINT('Ctrl Pts',(-0.0701778381840612,-0.407068917407805,
-1.64212536811722));
#17701=CARTESIAN_POINT('Ctrl Pts',(-0.140365781471549,-0.388086240756494,
-1.63761964365402));
#17702=CARTESIAN_POINT('Ctrl Pts',(-0.174042761838764,-0.373586846396559,
-1.63426473152765));
#17703=CARTESIAN_POINT('Ctrl Pts',(-0.233069203882014,-0.33909093068465,
-1.62691869420078));
#17704=CARTESIAN_POINT('Ctrl Pts',(-0.261368388670536,-0.317195968905306,
-1.62252828437015));
#17705=CARTESIAN_POINT('Ctrl Pts',(-0.311480544243686,-0.266264900654908,
-1.61365775139403));
#17706=CARTESIAN_POINT('Ctrl Pts',(-0.333298652394954,-0.237231147975234,
-1.60919314384089));
#17707=CARTESIAN_POINT('Ctrl Pts',(-0.373030350867485,-0.166543350814306,
-1.60050712143809));
#17708=CARTESIAN_POINT('Ctrl Pts',(-0.388626558458099,-0.123401821157026,
-1.59665523941937));
#17709=CARTESIAN_POINT('Ctrl Pts',(-0.397005914195118,-0.07938,-1.59456899932179));
#17710=CARTESIAN_POINT('Origin',(1.11022302462516E-16,-0.07938,-1.675));
#17711=CARTESIAN_POINT('Origin',(0.,-0.07938,0.));
#17712=CARTESIAN_POINT('',(0.846804978391753,-0.07938,-1.40825612658882));
#17713=CARTESIAN_POINT('Origin',(0.,-0.07938,0.));
#17714=CARTESIAN_POINT('Origin',(1.18440385848747,-0.07938,-1.18440385848747));
#17715=CARTESIAN_POINT('Origin',(1.18440385848747,0.,-1.18440385848747));
#17716=CARTESIAN_POINT('',(1.40825612658882,-0.07938,-0.846804978391753));
#17717=CARTESIAN_POINT('Ctrl Pts',(1.40825612658882,-0.0793800000000001,
-0.846804978391753));
#17718=CARTESIAN_POINT('Ctrl Pts',(1.40380622184538,-0.123401821157026,
-0.854205272175555));
#17719=CARTESIAN_POINT('Ctrl Pts',(1.39550172959303,-0.166543350814306,
-0.867957148219442));
#17720=CARTESIAN_POINT('Ctrl Pts',(1.3735491215176,-0.237231147975234,-0.902193646979983));
#17721=CARTESIAN_POINT('Ctrl Pts',(1.36127834356734,-0.266264900654908,
-0.920778333482565));
#17722=CARTESIAN_POINT('Ctrl Pts',(1.33211611256184,-0.317195968905306,
-0.962485392528369));
#17723=CARTESIAN_POINT('Ctrl Pts',(1.31521005565926,-0.33909093068465,-0.985600426557816));
#17724=CARTESIAN_POINT('Ctrl Pts',(1.27866649102984,-0.373586846396559,
-1.03253285680459));
#17725=CARTESIAN_POINT('Ctrl Pts',(1.25722555095714,-0.388086240756494,
-1.05871835910697));
#17726=CARTESIAN_POINT('Ctrl Pts',(1.2107812086231,-0.407068917407805,-1.11153475808518));
#17727=CARTESIAN_POINT('Ctrl Pts',(1.18575674747573,-0.411552957311693,
-1.13814686046673));
#17728=CARTESIAN_POINT('Ctrl Pts',(1.13814686046673,-0.411552957311693,
-1.18575674747573));
#17729=CARTESIAN_POINT('Ctrl Pts',(1.11153475808518,-0.407068917407805,
-1.2107812086231));
#17730=CARTESIAN_POINT('Ctrl Pts',(1.05871835910697,-0.388086240756494,
-1.25722555095714));
#17731=CARTESIAN_POINT('Ctrl Pts',(1.03253285680459,-0.373586846396559,
-1.27866649102984));
#17732=CARTESIAN_POINT('Ctrl Pts',(0.985600426557816,-0.33909093068465,
-1.31521005565926));
#17733=CARTESIAN_POINT('Ctrl Pts',(0.962485392528369,-0.317195968905306,
-1.33211611256184));
#17734=CARTESIAN_POINT('Ctrl Pts',(0.920778333482565,-0.266264900654909,
-1.36127834356734));
#17735=CARTESIAN_POINT('Ctrl Pts',(0.902193646979983,-0.237231147975234,
-1.3735491215176));
#17736=CARTESIAN_POINT('Ctrl Pts',(0.867957148219442,-0.166543350814306,
-1.39550172959303));
#17737=CARTESIAN_POINT('Ctrl Pts',(0.854205272175555,-0.123401821157026,
-1.40380622184538));
#17738=CARTESIAN_POINT('Ctrl Pts',(0.846804978391753,-0.0793800000000001,
-1.40825612658882));
#17739=CARTESIAN_POINT('Origin',(1.18440385848747,-0.07938,-1.18440385848747));
#17740=CARTESIAN_POINT('Origin',(0.,-0.27783,0.));
#17741=CARTESIAN_POINT('',(-1.643248,-0.47628,2.01239840340529E-16));
#17742=CARTESIAN_POINT('Origin',(0.,-0.47628,0.));
#17743=CARTESIAN_POINT('',(-1.643248,-0.27783,2.01239840340529E-16));
#17744=CARTESIAN_POINT('',(1.59456899932179,-0.07938,0.397005914195118));
#17745=CARTESIAN_POINT('Origin',(0.,-0.07938,0.));
#17746=CARTESIAN_POINT('',(1.59456899932179,-0.07938,-0.397005914195118));
#17747=CARTESIAN_POINT('Ctrl Pts',(1.59456899932179,-0.0793800000000001,
0.397005914195118));
#17748=CARTESIAN_POINT('Ctrl Pts',(1.59665523941937,-0.123401821157026,
0.388626558458099));
#17749=CARTESIAN_POINT('Ctrl Pts',(1.60050712143809,-0.166543350814306,
0.373030350867485));
#17750=CARTESIAN_POINT('Ctrl Pts',(1.60919314384089,-0.237231147975234,
0.333298652394954));
#17751=CARTESIAN_POINT('Ctrl Pts',(1.61365775139403,-0.266264900654909,
0.311480544243686));
#17752=CARTESIAN_POINT('Ctrl Pts',(1.62252828437015,-0.317195968905306,
0.261368388670537));
#17753=CARTESIAN_POINT('Ctrl Pts',(1.62691869420078,-0.33909093068465,0.233069203882014));
#17754=CARTESIAN_POINT('Ctrl Pts',(1.63426473152765,-0.373586846396559,
0.174042761838764));
#17755=CARTESIAN_POINT('Ctrl Pts',(1.63761964365402,-0.388086240756494,
0.140365781471549));
#17756=CARTESIAN_POINT('Ctrl Pts',(1.64212536811722,-0.407068917407805,
0.0701778381840612));
#17757=CARTESIAN_POINT('Ctrl Pts',(1.643248,-0.411552957311693,0.0336652739555916));
#17758=CARTESIAN_POINT('Ctrl Pts',(1.643248,-0.411552957311693,-0.0336652739555916));
#17759=CARTESIAN_POINT('Ctrl Pts',(1.64212536811722,-0.407068917407805,
-0.0701778381840612));
#17760=CARTESIAN_POINT('Ctrl Pts',(1.63761964365402,-0.388086240756494,
-0.140365781471549));
#17761=CARTESIAN_POINT('Ctrl Pts',(1.63426473152765,-0.373586846396559,
-0.174042761838764));
#17762=CARTESIAN_POINT('Ctrl Pts',(1.62691869420078,-0.33909093068465,-0.233069203882014));
#17763=CARTESIAN_POINT('Ctrl Pts',(1.62252828437015,-0.317195968905306,
-0.261368388670537));
#17764=CARTESIAN_POINT('Ctrl Pts',(1.61365775139403,-0.266264900654909,
-0.311480544243686));
#17765=CARTESIAN_POINT('Ctrl Pts',(1.60919314384089,-0.237231147975234,
-0.333298652394954));
#17766=CARTESIAN_POINT('Ctrl Pts',(1.60050712143809,-0.166543350814306,
-0.373030350867485));
#17767=CARTESIAN_POINT('Ctrl Pts',(1.59665523941937,-0.123401821157026,
-0.388626558458099));
#17768=CARTESIAN_POINT('Ctrl Pts',(1.59456899932179,-0.07938,-0.397005914195118));
#17769=CARTESIAN_POINT('Origin',(0.,-0.07938,0.));
#17770=CARTESIAN_POINT('Origin',(0.,-0.07938,0.));
#17771=CARTESIAN_POINT('Origin',(1.675,-0.07938,0.));
#17772=CARTESIAN_POINT('Origin',(1.675,0.,0.));
#17773=CARTESIAN_POINT('Origin',(1.675,-0.07938,0.));
#17774=CARTESIAN_POINT('Origin',(0.,-0.47628,0.));
#17775=CARTESIAN_POINT('Origin',(0.,-0.07938,0.));
#17776=CARTESIAN_POINT('',(0.,0.,0.));
#17777=CARTESIAN_POINT('Origin',(1.70469,0.695,0.));
#17778=CARTESIAN_POINT('',(-1.70469,0.695,-2.0876431520385E-16));
#17779=CARTESIAN_POINT('Origin',(0.,0.695,0.));
#17780=CARTESIAN_POINT('',(-1.65031,0.695,-2.02104685910087E-16));
#17781=CARTESIAN_POINT('Origin',(0.,0.695,0.));
#17782=CARTESIAN_POINT('Origin',(0.,0.6575,0.));
#17783=CARTESIAN_POINT('',(-1.70469,0.62,-2.0876431520385E-16));
#17784=CARTESIAN_POINT('Origin',(0.,0.62,0.));
#17785=CARTESIAN_POINT('',(-1.70469,0.6575,-2.0876431520385E-16));
#17786=CARTESIAN_POINT('Origin',(1.65031,0.62,0.));
#17787=CARTESIAN_POINT('',(-1.65031,0.62,-2.02104685910087E-16));
#17788=CARTESIAN_POINT('Origin',(0.,0.62,0.));
#17789=CARTESIAN_POINT('Origin',(0.,0.6575,0.));
#17790=CARTESIAN_POINT('',(-1.65031,0.6575,-2.02104685910087E-16));
#17791=CARTESIAN_POINT('Origin',(1.70469,-0.62,0.));
#17792=CARTESIAN_POINT('',(-1.70469,-0.62,-2.0876431520385E-16));
#17793=CARTESIAN_POINT('Origin',(0.,-0.62,0.));
#17794=CARTESIAN_POINT('',(-1.65031,-0.62,-2.02104685910087E-16));
#17795=CARTESIAN_POINT('Origin',(0.,-0.62,0.));
#17796=CARTESIAN_POINT('Origin',(0.,-0.6575,0.));
#17797=CARTESIAN_POINT('',(-1.70469,-0.695,-2.0876431520385E-16));
#17798=CARTESIAN_POINT('Origin',(0.,-0.695,0.));
#17799=CARTESIAN_POINT('',(-1.70469,-0.6575,-2.0876431520385E-16));
#17800=CARTESIAN_POINT('Origin',(1.65031,-0.695,0.));
#17801=CARTESIAN_POINT('',(-1.65031,-0.695,-2.02104685910087E-16));
#17802=CARTESIAN_POINT('Origin',(0.,-0.695,0.));
#17803=CARTESIAN_POINT('Origin',(0.,-0.6575,0.));
#17804=CARTESIAN_POINT('',(-1.65031,-0.6575,-2.02104685910087E-16));
#17805=CARTESIAN_POINT('',(0.,0.,0.));
#17806=CARTESIAN_POINT('',(0.,0.,0.));
#17807=CARTESIAN_POINT('',(0.,0.,0.));
#17808=CARTESIAN_POINT('',(0.,0.,0.));
#17809=CARTESIAN_POINT('',(0.,0.,0.));
#17810=CARTESIAN_POINT('',(0.,0.,0.));
#17811=CARTESIAN_POINT('Origin',(0.3,0.4,0.));
#17812=CARTESIAN_POINT('',(-0.3,0.4,-3.67394039744206E-17));
#17813=CARTESIAN_POINT('Origin',(0.,0.4,0.));
#17814=CARTESIAN_POINT('Origin',(0.,0.375,0.));
#17815=CARTESIAN_POINT('',(-0.35,0.35,-4.28626379701573E-17));
#17816=CARTESIAN_POINT('Origin',(0.,0.35,0.));
#17817=CARTESIAN_POINT('',(-0.325,0.375,-3.9801020972289E-17));
#17818=CARTESIAN_POINT('Origin',(0.,0.19,0.));
#17819=CARTESIAN_POINT('',(-0.35,0.03,-4.28626379701574E-17));
#17820=CARTESIAN_POINT('Origin',(0.,0.03,0.));
#17821=CARTESIAN_POINT('',(-0.35,0.19,-4.28626379701574E-17));
#17822=CARTESIAN_POINT('Origin',(0.,0.0149999999999999,0.));
#17823=CARTESIAN_POINT('',(-0.32,-3.29597460435593E-17,-3.91886975727153E-17));
#17824=CARTESIAN_POINT('Origin',(0.,0.,0.));
#17825=CARTESIAN_POINT('',(-0.335,0.0149999999999999,-4.10256677714363E-17));
#17826=CARTESIAN_POINT('Origin',(0.22,0.,0.));
#17827=CARTESIAN_POINT('',(-0.22,-6.93889390390723E-18,-2.69422295812418E-17));
#17828=CARTESIAN_POINT('Origin',(0.,0.,0.));
#17829=CARTESIAN_POINT('Origin',(0.,-0.02,0.));
#17830=CARTESIAN_POINT('',(-0.1954,-0.0492,2.39295984553393E-17));
#17831=CARTESIAN_POINT('Origin',(0.,-0.0492,0.));
#17832=CARTESIAN_POINT('',(-0.21,-0.02,-2.57175827820944E-17));
#17833=CARTESIAN_POINT('Origin',(0.,-0.8,0.));
#17834=CARTESIAN_POINT('',(-0.1954,-1.5646,2.39295984553393E-17));
#17835=CARTESIAN_POINT('Origin',(0.,-1.5646,0.));
#17836=CARTESIAN_POINT('',(-0.1954,-0.8,-2.39295984553393E-17));
#17837=CARTESIAN_POINT('Origin',(0.,-1.58,0.));
#17838=CARTESIAN_POINT('',(-0.16,-1.6,-1.95943487863577E-17));
#17839=CARTESIAN_POINT('Origin',(0.,-1.6,0.));
#17840=CARTESIAN_POINT('',(-0.18,-1.58,-2.20436423846524E-17));
#17841=CARTESIAN_POINT('Origin',(0.,-1.6,0.));
#17842=CARTESIAN_POINT('Origin',(0.0866025403784439,-0.4,-0.15));
#17843=CARTESIAN_POINT('',(0.173205080756888,-0.4,0.));
#17844=CARTESIAN_POINT('',(0.0866025403784439,-0.4,-0.15));
#17845=CARTESIAN_POINT('',(0.173205080756888,-0.4,0.));
#17846=CARTESIAN_POINT('',(0.0866025403784439,-0.64,-0.15));
#17847=CARTESIAN_POINT('',(0.0866025403784439,-0.4,-0.15));
#17848=CARTESIAN_POINT('',(0.173205080756888,-0.64,0.));
#17849=CARTESIAN_POINT('',(0.173205080756888,-0.64,0.));
#17850=CARTESIAN_POINT('',(0.173205080756888,-0.4,0.));
#17851=CARTESIAN_POINT('Origin',(-0.0866025403784438,-0.4,-0.15));
#17852=CARTESIAN_POINT('',(-0.0866025403784438,-0.4,-0.15));
#17853=CARTESIAN_POINT('',(0.0866025403784439,-0.4,-0.15));
#17854=CARTESIAN_POINT('',(-0.0866025403784438,-0.64,-0.15));
#17855=CARTESIAN_POINT('',(-0.0866025403784438,-0.4,-0.15));
#17856=CARTESIAN_POINT('',(0.0866025403784439,-0.64,-0.15));
#17857=CARTESIAN_POINT('Origin',(-0.173205080756888,-0.4,-2.77555756156289E-17));
#17858=CARTESIAN_POINT('',(-0.173205080756888,-0.4,-2.12115047744981E-17));
#17859=CARTESIAN_POINT('',(-0.0866025403784438,-0.4,-0.15));
#17860=CARTESIAN_POINT('',(-0.173205080756888,-0.64,-2.77555756156289E-17));
#17861=CARTESIAN_POINT('',(-0.173205080756888,-0.4,-2.12115047744981E-17));
#17862=CARTESIAN_POINT('',(-0.0866025403784438,-0.64,-0.15));
#17863=CARTESIAN_POINT('Origin',(-0.0866025403784439,-0.4,0.15));
#17864=CARTESIAN_POINT('',(-0.0866025403784439,-0.4,0.15));
#17865=CARTESIAN_POINT('',(-0.173205080756888,-0.4,-2.12115047744981E-17));
#17866=CARTESIAN_POINT('',(-0.0866025403784439,-0.64,0.15));
#17867=CARTESIAN_POINT('',(-0.0866025403784439,-0.4,0.15));
#17868=CARTESIAN_POINT('',(-0.173205080756888,-0.64,-2.12115047744981E-17));
#17869=CARTESIAN_POINT('Origin',(0.0866025403784439,-0.4,0.15));
#17870=CARTESIAN_POINT('',(0.0866025403784439,-0.4,0.15));
#17871=CARTESIAN_POINT('',(-0.0866025403784439,-0.4,0.15));
#17872=CARTESIAN_POINT('',(0.0866025403784439,-0.64,0.15));
#17873=CARTESIAN_POINT('',(0.0866025403784439,-0.4,0.15));
#17874=CARTESIAN_POINT('',(-0.0866025403784439,-0.64,0.15));
#17875=CARTESIAN_POINT('Origin',(0.173205080756888,-0.4,0.));
#17876=CARTESIAN_POINT('',(0.0866025403784439,-0.4,0.15));
#17877=CARTESIAN_POINT('',(0.0866025403784439,-0.64,0.15));
#17878=CARTESIAN_POINT('Origin',(0.,-0.4,-2.77555756156289E-17));
#17879=CARTESIAN_POINT('Origin',(0.,-0.64,-2.77555756156289E-17));
#17880=CARTESIAN_POINT('',(0.,0.,0.));
#17881=CARTESIAN_POINT('',(0.,0.,0.));
#17882=CARTESIAN_POINT('',(0.,0.,0.));
#17883=CARTESIAN_POINT('',(0.,0.,0.));
#17884=CARTESIAN_POINT('',(0.,0.,0.));
#17885=CARTESIAN_POINT('',(0.,0.,0.));
#17886=CARTESIAN_POINT('',(0.,0.,0.));
#17887=CARTESIAN_POINT('',(0.,0.,0.));
#17888=CARTESIAN_POINT('',(0.,0.,0.));
#17889=CARTESIAN_POINT('',(0.,0.,0.));
#17890=CARTESIAN_POINT('',(0.,0.,0.));
#17891=CARTESIAN_POINT('',(-2.,-3.9,2.));
#17892=CARTESIAN_POINT('',(-2.,3.9,2.));
#17893=CARTESIAN_POINT('',(-2.,-3.9,9.));
#17894=CARTESIAN_POINT('',(-2.,3.9,9.));
#17895=CARTESIAN_POINT('',(10.,-3.9,2.));
#17896=CARTESIAN_POINT('',(10.,3.9,2.));
#17897=CARTESIAN_POINT('',(10.,-3.9,9.));
#17898=CARTESIAN_POINT('',(10.,3.9,9.));
#17899=CARTESIAN_POINT('',(-2.,-3.5,-1.));
#17900=CARTESIAN_POINT('',(-2.,3.5,-1.));
#17901=CARTESIAN_POINT('',(10.,-3.5,-1.));
#17902=CARTESIAN_POINT('',(10.,3.5,-1.));
#17903=CARTESIAN_POINT('',(0.,-3.5,5.));
#17904=CARTESIAN_POINT('',(1.16341445918999E-16,-4.7,6.9));
#17905=CARTESIAN_POINT('',(-1.64544826719043,-4.7,4.05));
#17906=CARTESIAN_POINT('',(1.64544826719043,-4.7,4.05));
#17907=CARTESIAN_POINT('',(6.,-3.5,5.));
#17908=CARTESIAN_POINT('',(6.,-4.7,7.6));
#17909=CARTESIAN_POINT('',(3.74833395016046,-4.7,3.7));
#17910=CARTESIAN_POINT('',(8.25166604983954,-4.7,3.7));
#17911=CARTESIAN_POINT('',(0.,3.5,5.));
#17912=CARTESIAN_POINT('',(1.16341445918999E-16,4.7,6.9));
#17913=CARTESIAN_POINT('',(-1.64544826719043,4.7,4.05));
#17914=CARTESIAN_POINT('',(1.64544826719043,4.7,4.05));
#17915=CARTESIAN_POINT('',(6.,3.5,5.));
#17916=CARTESIAN_POINT('',(6.,4.7,7.6));
#17917=CARTESIAN_POINT('',(3.74833395016046,4.7,3.7));
#17918=CARTESIAN_POINT('',(8.25166604983954,4.7,3.7));
#17919=CARTESIAN_POINT('',(0.,0.,0.));
#17920=CARTESIAN_POINT('',(0.,0.,0.));
#17921=CARTESIAN_POINT('Origin',(-0.2,-0.9,-0.7));
#17922=CARTESIAN_POINT('',(-0.2,2.1,-0.565685424949238));
#17923=CARTESIAN_POINT('',(-0.2,-0.9,-0.565685424949238));
#17924=CARTESIAN_POINT('',(-0.2,-6.,-0.565685424949238));
#17925=CARTESIAN_POINT('',(-0.2,2.1,-0.35));
#17926=CARTESIAN_POINT('',(-0.2,2.1,-0.35));
#17927=CARTESIAN_POINT('',(-0.2,-0.9,-0.35));
#17928=CARTESIAN_POINT('',(-0.2,-0.9,-0.35));
#17929=CARTESIAN_POINT('',(-0.2,-0.9,-0.35));
#17930=CARTESIAN_POINT('Origin',(0.,-0.9,-0.525));
#17931=CARTESIAN_POINT('',(0.2,-0.9,-0.565685424949238));
#17932=CARTESIAN_POINT('Origin',(0.,-0.9,0.));
#17933=CARTESIAN_POINT('',(0.2,-0.9,-0.35));
#17934=CARTESIAN_POINT('',(0.2,-0.9,-0.35));
#17935=CARTESIAN_POINT('',(0.2,-0.9,-0.7));
#17936=CARTESIAN_POINT('Origin',(0.2,-0.9,-0.35));
#17937=CARTESIAN_POINT('',(0.2,2.1,-0.565685424949238));
#17938=CARTESIAN_POINT('',(0.2,-6.,-0.565685424949238));
#17939=CARTESIAN_POINT('',(0.2,2.1,-0.35));
#17940=CARTESIAN_POINT('',(0.2,-0.9,-0.35));
#17941=CARTESIAN_POINT('',(0.2,2.1,-0.7));
#17942=CARTESIAN_POINT('Origin',(-0.2,-0.9,-0.35));
#17943=CARTESIAN_POINT('',(0.2,2.1,-0.35));
#17944=CARTESIAN_POINT('Origin',(0.,2.1,-0.525));
#17945=CARTESIAN_POINT('Origin',(0.,2.1,0.));
#17946=CARTESIAN_POINT('Origin',(0.,-6.,0.));
#17947=CARTESIAN_POINT('',(-0.6,6.5,7.34788079488412E-17));
#17948=CARTESIAN_POINT('Origin',(0.,6.5,0.));
#17949=CARTESIAN_POINT('',(-0.6,-6.,7.34788079488412E-17));
#17950=CARTESIAN_POINT('',(-0.6,-6.,7.34788079488412E-17));
#17951=CARTESIAN_POINT('Origin',(0.,-6.,0.));
#17952=CARTESIAN_POINT('Origin',(0.,6.5,0.));
#17953=CARTESIAN_POINT('Origin',(0.,-6.,0.));
#17954=CARTESIAN_POINT('',(0.,0.,0.));
#17955=CARTESIAN_POINT('Origin',(0.,-3.,0.));
#17956=CARTESIAN_POINT('',(-0.61,-1.,7.47034547479885E-17));
#17957=CARTESIAN_POINT('Origin',(0.,-1.,0.));
#17958=CARTESIAN_POINT('',(-0.61,-3.,7.47034547479885E-17));
#17959=CARTESIAN_POINT('',(-0.61,-3.,7.47034547479885E-17));
#17960=CARTESIAN_POINT('Origin',(0.,-3.,0.));
#17961=CARTESIAN_POINT('Origin',(0.,-3.,0.));
#17962=CARTESIAN_POINT('',(-0.9,-1.,1.10218211923262E-16));
#17963=CARTESIAN_POINT('Origin',(0.,-1.,0.));
#17964=CARTESIAN_POINT('',(-0.9,-3.,1.10218211923262E-16));
#17965=CARTESIAN_POINT('',(-0.9,-3.,1.10218211923262E-16));
#17966=CARTESIAN_POINT('Origin',(0.,-3.,0.));
#17967=CARTESIAN_POINT('Origin',(0.,-1.,0.));
#17968=CARTESIAN_POINT('Origin',(0.,-3.,0.));
#17969=CARTESIAN_POINT('',(0.,0.,0.));
#17970=CARTESIAN_POINT('Origin',(0.,2.2,0.));
#17971=CARTESIAN_POINT('',(-0.61,3.,7.47034547479885E-17));
#17972=CARTESIAN_POINT('Origin',(0.,3.,0.));
#17973=CARTESIAN_POINT('',(-0.61,2.2,7.47034547479885E-17));
#17974=CARTESIAN_POINT('',(-0.61,2.2,7.47034547479885E-17));
#17975=CARTESIAN_POINT('Origin',(0.,2.2,0.));
#17976=CARTESIAN_POINT('Origin',(0.,2.2,0.));
#17977=CARTESIAN_POINT('',(-0.9,3.,1.10218211923262E-16));
#17978=CARTESIAN_POINT('Origin',(0.,3.,0.));
#17979=CARTESIAN_POINT('',(-0.9,2.2,1.10218211923262E-16));
#17980=CARTESIAN_POINT('',(-0.9,2.2,1.10218211923262E-16));
#17981=CARTESIAN_POINT('Origin',(0.,2.2,0.));
#17982=CARTESIAN_POINT('Origin',(0.,3.,0.));
#17983=CARTESIAN_POINT('Origin',(0.,2.2,0.));
#17984=CARTESIAN_POINT('',(0.,0.,0.));
#17985=CARTESIAN_POINT('Origin',(0.,-5.1,0.59));
#17986=CARTESIAN_POINT('',(0.133884278389959,-5.26178689687363,0.59));
#17987=CARTESIAN_POINT('',(0.133884278389959,-4.93821310312637,0.59));
#17988=CARTESIAN_POINT('',(0.133884278389959,-5.5,0.59));
#17989=CARTESIAN_POINT('Origin',(0.,-5.1,0.59));
#17990=CARTESIAN_POINT('Origin',(0.,-5.1,0.59));
#17991=CARTESIAN_POINT('',(-0.133884278389959,-5.26178689687363,0.59));
#17992=CARTESIAN_POINT('Ctrl Pts',(-0.133884278389959,-5.26178689687363,
0.59));
#17993=CARTESIAN_POINT('Ctrl Pts',(-0.118254395260804,-5.27472116821763,
0.59354677224418));
#17994=CARTESIAN_POINT('Ctrl Pts',(-0.1001097876823,-5.28579931658744,0.596982247899573));
#17995=CARTESIAN_POINT('Ctrl Pts',(-0.0548298721325195,-5.30463856105443,
0.603074162899704));
#17996=CARTESIAN_POINT('Ctrl Pts',(-0.0266020595922903,-5.31,0.605));
#17997=CARTESIAN_POINT('Ctrl Pts',(0.0266020595922903,-5.31,0.605));
#17998=CARTESIAN_POINT('Ctrl Pts',(0.0548298721325197,-5.30463856105443,
0.603074162899704));
#17999=CARTESIAN_POINT('Ctrl Pts',(0.100109787682301,-5.28579931658744,
0.596982247899573));
#18000=CARTESIAN_POINT('Ctrl Pts',(0.118254395260804,-5.27472116821763,
0.59354677224418));
#18001=CARTESIAN_POINT('Ctrl Pts',(0.133884278389959,-5.26178689687363,
0.59));
#18002=CARTESIAN_POINT('',(-0.21,-5.1,0.59));
#18003=CARTESIAN_POINT('Origin',(0.,-5.1,0.59));
#18004=CARTESIAN_POINT('',(-0.21,-5.1,1.07976849370594));
#18005=CARTESIAN_POINT('',(-0.21,-5.1,0.59));
#18006=CARTESIAN_POINT('',(0.21,-5.1,1.07976849370594));
#18007=CARTESIAN_POINT('Ctrl Pts',(0.21,-5.1,1.07976849370594));
#18008=CARTESIAN_POINT('Ctrl Pts',(0.21,-5.12643858813051,1.07976849370594));
#18009=CARTESIAN_POINT('Ctrl Pts',(0.204702922670977,-5.15459378125493,
1.08084015664674));
#18010=CARTESIAN_POINT('Ctrl Pts',(0.183251796806355,-5.20631344554134,
1.08468313707126));
#18011=CARTESIAN_POINT('Ctrl Pts',(0.167101177357215,-5.22988367074114,
1.08739593054622));
#18012=CARTESIAN_POINT('Ctrl Pts',(0.129884533480965,-5.26710031461738,
1.09246633289124));
#18013=CARTESIAN_POINT('Ctrl Pts',(0.106313940757289,-5.28325161016341,
1.09515738895358));
#18014=CARTESIAN_POINT('Ctrl Pts',(0.0545930033295209,-5.30470322656974,
1.09895039220591));
#18015=CARTESIAN_POINT('Ctrl Pts',(0.0264373623835353,-5.31,1.1));
#18016=CARTESIAN_POINT('Ctrl Pts',(-0.0264373623835352,-5.31,1.1));
#18017=CARTESIAN_POINT('Ctrl Pts',(-0.0545930033295208,-5.30470322656974,
1.09895039220591));
#18018=CARTESIAN_POINT('Ctrl Pts',(-0.106313940757289,-5.28325161016341,
1.09515738895358));
#18019=CARTESIAN_POINT('Ctrl Pts',(-0.129884533480965,-5.26710031461738,
1.09246633289124));
#18020=CARTESIAN_POINT('Ctrl Pts',(-0.167101177357215,-5.22988367074114,
1.08739593054622));
#18021=CARTESIAN_POINT('Ctrl Pts',(-0.183251796806354,-5.20631344554134,
1.08468313707126));
#18022=CARTESIAN_POINT('Ctrl Pts',(-0.204702922670976,-5.15459378125493,
1.08084015664674));
#18023=CARTESIAN_POINT('Ctrl Pts',(-0.21,-5.12643858813051,1.07976849370594));
#18024=CARTESIAN_POINT('Ctrl Pts',(-0.21,-5.1,1.07976849370594));
#18025=CARTESIAN_POINT('Ctrl Pts',(-0.21,-5.1,1.07976849370594));
#18026=CARTESIAN_POINT('Ctrl Pts',(-0.21,-5.07356141186949,1.07976849370594));
#18027=CARTESIAN_POINT('Ctrl Pts',(-0.204702922670977,-5.04540621874507,
1.08084015664674));
#18028=CARTESIAN_POINT('Ctrl Pts',(-0.183251796806355,-4.99368655445866,
1.08468313707126));
#18029=CARTESIAN_POINT('Ctrl Pts',(-0.167101177357215,-4.97011632925886,
1.08739593054622));
#18030=CARTESIAN_POINT('Ctrl Pts',(-0.129884533480965,-4.93289968538261,
1.09246633289124));
#18031=CARTESIAN_POINT('Ctrl Pts',(-0.106313940757289,-4.91674838983659,
1.09515738895358));
#18032=CARTESIAN_POINT('Ctrl Pts',(-0.0545930033295209,-4.89529677343026,
1.09895039220591));
#18033=CARTESIAN_POINT('Ctrl Pts',(-0.0264373623835353,-4.89,1.1));
#18034=CARTESIAN_POINT('Ctrl Pts',(0.0264373623835353,-4.89,1.1));
#18035=CARTESIAN_POINT('Ctrl Pts',(0.0545930033295197,-4.89529677343026,
1.09895039220591));
#18036=CARTESIAN_POINT('Ctrl Pts',(0.106313940757288,-4.91674838983659,
1.09515738895358));
#18037=CARTESIAN_POINT('Ctrl Pts',(0.129884533480965,-4.93289968538261,
1.09246633289124));
#18038=CARTESIAN_POINT('Ctrl Pts',(0.167101177357214,-4.97011632925886,
1.08739593054622));
#18039=CARTESIAN_POINT('Ctrl Pts',(0.183251796806355,-4.99368655445866,
1.08468313707126));
#18040=CARTESIAN_POINT('Ctrl Pts',(0.204702922670977,-5.04540621874507,
1.08084015664674));
#18041=CARTESIAN_POINT('Ctrl Pts',(0.21,-5.07356141186949,1.07976849370594));
#18042=CARTESIAN_POINT('Ctrl Pts',(0.21,-5.1,1.07976849370594));
#18043=CARTESIAN_POINT('',(-0.133884278389959,-4.93821310312637,0.59));
#18044=CARTESIAN_POINT('Origin',(0.,-5.1,0.59));
#18045=CARTESIAN_POINT('Ctrl Pts',(0.133884278389959,-4.93821310312637,
0.59));
#18046=CARTESIAN_POINT('Ctrl Pts',(0.118254395260804,-4.92527883178237,
0.59354677224418));
#18047=CARTESIAN_POINT('Ctrl Pts',(0.1001097876823,-4.91420068341256,0.596982247899573));
#18048=CARTESIAN_POINT('Ctrl Pts',(0.0548298721325194,-4.89536143894557,
0.603074162899704));
#18049=CARTESIAN_POINT('Ctrl Pts',(0.0266020595922903,-4.89,0.605));
#18050=CARTESIAN_POINT('Ctrl Pts',(-0.0266020595922903,-4.89,0.605));
#18051=CARTESIAN_POINT('Ctrl Pts',(-0.0548298721325194,-4.89536143894557,
0.603074162899704));
#18052=CARTESIAN_POINT('Ctrl Pts',(-0.1001097876823,-4.91420068341256,0.596982247899573));
#18053=CARTESIAN_POINT('Ctrl Pts',(-0.118254395260804,-4.92527883178237,
0.59354677224418));
#18054=CARTESIAN_POINT('Ctrl Pts',(-0.133884278389959,-4.93821310312636,
0.59));
#18055=CARTESIAN_POINT('Origin',(0.,-5.1,0.59));
#18056=CARTESIAN_POINT('',(-0.133884278389959,-5.5,0.59));
#18057=CARTESIAN_POINT('Origin',(0.,-5.5,0.));
#18058=CARTESIAN_POINT('',(-0.605,-4.7,7.40911313484149E-17));
#18059=CARTESIAN_POINT('Origin',(0.,-4.7,0.));
#18060=CARTESIAN_POINT('',(-0.605,-5.5,7.40911313484149E-17));
#18061=CARTESIAN_POINT('',(-0.605,-5.5,7.40911313484149E-17));
#18062=CARTESIAN_POINT('Origin',(0.,-5.5,0.));
#18063=CARTESIAN_POINT('Origin',(0.,-5.5,0.));
#18064=CARTESIAN_POINT('',(-1.1,-4.7,1.34711147906209E-16));
#18065=CARTESIAN_POINT('Origin',(0.,-4.7,0.));
#18066=CARTESIAN_POINT('',(-1.1,-5.5,1.34711147906209E-16));
#18067=CARTESIAN_POINT('',(-1.1,-5.5,1.34711147906209E-16));
#18068=CARTESIAN_POINT('Origin',(0.,-5.5,0.));
#18069=CARTESIAN_POINT('Origin',(0.,-4.7,0.));
#18070=CARTESIAN_POINT('Origin',(0.,-5.5,0.));
#18071=CARTESIAN_POINT('',(0.,0.,0.));
#18072=CARTESIAN_POINT('Origin',(0.,-4.7,0.));
#18073=CARTESIAN_POINT('',(-0.61,-4.,7.47034547479885E-17));
#18074=CARTESIAN_POINT('Origin',(0.,-4.,0.));
#18075=CARTESIAN_POINT('',(-0.61,-4.7,7.47034547479885E-17));
#18076=CARTESIAN_POINT('',(-0.61,-4.7,7.47034547479885E-17));
#18077=CARTESIAN_POINT('Origin',(0.,-4.7,0.));
#18078=CARTESIAN_POINT('Origin',(0.,-4.7,0.));
#18079=CARTESIAN_POINT('',(-0.9,-4.,1.10218211923262E-16));
#18080=CARTESIAN_POINT('Origin',(0.,-4.,0.));
#18081=CARTESIAN_POINT('',(-0.9,-4.7,1.10218211923262E-16));
#18082=CARTESIAN_POINT('',(-0.9,-4.7,1.10218211923262E-16));
#18083=CARTESIAN_POINT('Origin',(0.,-4.7,0.));
#18084=CARTESIAN_POINT('Origin',(0.,-4.,0.));
#18085=CARTESIAN_POINT('Origin',(0.,-4.7,0.));
#18086=CARTESIAN_POINT('',(0.,0.,0.));
#18087=CARTESIAN_POINT('Origin',(0.,5.1,0.59));
#18088=CARTESIAN_POINT('',(0.133884278389959,4.93821310312637,0.59));
#18089=CARTESIAN_POINT('',(0.133884278389959,5.26178689687363,0.59));
#18090=CARTESIAN_POINT('',(0.133884278389959,4.7,0.59));
#18091=CARTESIAN_POINT('Origin',(0.,5.1,0.59));
#18092=CARTESIAN_POINT('Origin',(0.,5.1,0.59));
#18093=CARTESIAN_POINT('',(-0.133884278389959,4.93821310312637,0.59));
#18094=CARTESIAN_POINT('Ctrl Pts',(-0.133884278389959,4.93821310312636,
0.59));
#18095=CARTESIAN_POINT('Ctrl Pts',(-0.118254395260804,4.92527883178237,
0.59354677224418));
#18096=CARTESIAN_POINT('Ctrl Pts',(-0.1001097876823,4.91420068341256,0.596982247899573));
#18097=CARTESIAN_POINT('Ctrl Pts',(-0.0548298721325195,4.89536143894557,
0.603074162899704));
#18098=CARTESIAN_POINT('Ctrl Pts',(-0.0266020595922903,4.89,0.605));
#18099=CARTESIAN_POINT('Ctrl Pts',(0.0266020595922903,4.89,0.605));
#18100=CARTESIAN_POINT('Ctrl Pts',(0.0548298721325186,4.89536143894557,
0.603074162899704));
#18101=CARTESIAN_POINT('Ctrl Pts',(0.1001097876823,4.91420068341256,0.596982247899573));
#18102=CARTESIAN_POINT('Ctrl Pts',(0.118254395260804,4.92527883178237,0.59354677224418));
#18103=CARTESIAN_POINT('Ctrl Pts',(0.133884278389959,4.93821310312637,0.59));
#18104=CARTESIAN_POINT('',(-0.21,5.1,0.59));
#18105=CARTESIAN_POINT('Origin',(0.,5.1,0.59));
#18106=CARTESIAN_POINT('',(-0.21,5.1,1.07976849370594));
#18107=CARTESIAN_POINT('',(-0.21,5.1,0.59));
#18108=CARTESIAN_POINT('',(0.21,5.1,1.07976849370594));
#18109=CARTESIAN_POINT('Ctrl Pts',(0.21,5.1,1.07976849370594));
#18110=CARTESIAN_POINT('Ctrl Pts',(0.21,5.07356141186949,1.07976849370594));
#18111=CARTESIAN_POINT('Ctrl Pts',(0.204702922670977,5.04540621874507,1.08084015664674));
#18112=CARTESIAN_POINT('Ctrl Pts',(0.183251796806355,4.99368655445866,1.08468313707126));
#18113=CARTESIAN_POINT('Ctrl Pts',(0.167101177357215,4.97011632925886,1.08739593054622));
#18114=CARTESIAN_POINT('Ctrl Pts',(0.129884533480965,4.93289968538261,1.09246633289124));
#18115=CARTESIAN_POINT('Ctrl Pts',(0.106313940757289,4.91674838983659,1.09515738895358));
#18116=CARTESIAN_POINT('Ctrl Pts',(0.0545930033295209,4.89529677343026,
1.09895039220591));
#18117=CARTESIAN_POINT('Ctrl Pts',(0.0264373623835353,4.89,1.1));
#18118=CARTESIAN_POINT('Ctrl Pts',(-0.0264373623835352,4.89,1.1));
#18119=CARTESIAN_POINT('Ctrl Pts',(-0.0545930033295208,4.89529677343026,
1.09895039220591));
#18120=CARTESIAN_POINT('Ctrl Pts',(-0.106313940757289,4.91674838983659,
1.09515738895358));
#18121=CARTESIAN_POINT('Ctrl Pts',(-0.129884533480965,4.93289968538261,
1.09246633289124));
#18122=CARTESIAN_POINT('Ctrl Pts',(-0.167101177357215,4.97011632925886,
1.08739593054622));
#18123=CARTESIAN_POINT('Ctrl Pts',(-0.183251796806354,4.99368655445866,
1.08468313707126));
#18124=CARTESIAN_POINT('Ctrl Pts',(-0.204702922670976,5.04540621874507,
1.08084015664674));
#18125=CARTESIAN_POINT('Ctrl Pts',(-0.21,5.07356141186949,1.07976849370594));
#18126=CARTESIAN_POINT('Ctrl Pts',(-0.21,5.1,1.07976849370594));
#18127=CARTESIAN_POINT('Ctrl Pts',(-0.21,5.1,1.07976849370594));
#18128=CARTESIAN_POINT('Ctrl Pts',(-0.21,5.12643858813051,1.07976849370594));
#18129=CARTESIAN_POINT('Ctrl Pts',(-0.204702922670977,5.15459378125493,
1.08084015664674));
#18130=CARTESIAN_POINT('Ctrl Pts',(-0.183251796806355,5.20631344554134,
1.08468313707126));
#18131=CARTESIAN_POINT('Ctrl Pts',(-0.167101177357215,5.22988367074114,
1.08739593054622));
#18132=CARTESIAN_POINT('Ctrl Pts',(-0.129884533480965,5.26710031461738,
1.09246633289124));
#18133=CARTESIAN_POINT('Ctrl Pts',(-0.106313940757289,5.28325161016341,
1.09515738895358));
#18134=CARTESIAN_POINT('Ctrl Pts',(-0.0545930033295209,5.30470322656974,
1.09895039220591));
#18135=CARTESIAN_POINT('Ctrl Pts',(-0.0264373623835353,5.31,1.1));
#18136=CARTESIAN_POINT('Ctrl Pts',(0.0264373623835353,5.31,1.1));
#18137=CARTESIAN_POINT('Ctrl Pts',(0.0545930033295212,5.30470322656974,
1.09895039220591));
#18138=CARTESIAN_POINT('Ctrl Pts',(0.106313940757289,5.28325161016341,1.09515738895358));
#18139=CARTESIAN_POINT('Ctrl Pts',(0.129884533480965,5.26710031461738,1.09246633289124));
#18140=CARTESIAN_POINT('Ctrl Pts',(0.167101177357214,5.22988367074114,1.08739593054622));
#18141=CARTESIAN_POINT('Ctrl Pts',(0.183251796806355,5.20631344554134,1.08468313707126));
#18142=CARTESIAN_POINT('Ctrl Pts',(0.204702922670977,5.15459378125493,1.08084015664674));
#18143=CARTESIAN_POINT('Ctrl Pts',(0.21,5.12643858813051,1.07976849370594));
#18144=CARTESIAN_POINT('Ctrl Pts',(0.21,5.1,1.07976849370594));
#18145=CARTESIAN_POINT('',(-0.133884278389959,5.26178689687363,0.59));
#18146=CARTESIAN_POINT('Origin',(0.,5.1,0.59));
#18147=CARTESIAN_POINT('Ctrl Pts',(0.133884278389959,5.26178689687363,0.59));
#18148=CARTESIAN_POINT('Ctrl Pts',(0.118254395260804,5.27472116821763,0.59354677224418));
#18149=CARTESIAN_POINT('Ctrl Pts',(0.1001097876823,5.28579931658744,0.596982247899573));
#18150=CARTESIAN_POINT('Ctrl Pts',(0.0548298721325194,5.30463856105443,
0.603074162899704));
#18151=CARTESIAN_POINT('Ctrl Pts',(0.0266020595922903,5.31,0.605));
#18152=CARTESIAN_POINT('Ctrl Pts',(-0.0266020595922903,5.31,0.605));
#18153=CARTESIAN_POINT('Ctrl Pts',(-0.0548298721325194,5.30463856105443,
0.603074162899704));
#18154=CARTESIAN_POINT('Ctrl Pts',(-0.1001097876823,5.28579931658744,0.596982247899573));
#18155=CARTESIAN_POINT('Ctrl Pts',(-0.118254395260804,5.27472116821763,
0.59354677224418));
#18156=CARTESIAN_POINT('Ctrl Pts',(-0.133884278389958,5.26178689687363,
0.59));
#18157=CARTESIAN_POINT('Origin',(0.,5.1,0.59));
#18158=CARTESIAN_POINT('',(-0.133884278389959,4.7,0.59));
#18159=CARTESIAN_POINT('Origin',(0.,4.7,0.));
#18160=CARTESIAN_POINT('',(-0.605,5.5,7.40911313484149E-17));
#18161=CARTESIAN_POINT('Origin',(0.,5.5,0.));
#18162=CARTESIAN_POINT('',(-0.605,4.7,7.40911313484149E-17));
#18163=CARTESIAN_POINT('',(-0.605,4.7,7.40911313484149E-17));
#18164=CARTESIAN_POINT('Origin',(0.,4.7,0.));
#18165=CARTESIAN_POINT('Origin',(0.,4.7,0.));
#18166=CARTESIAN_POINT('',(-1.1,5.5,1.34711147906209E-16));
#18167=CARTESIAN_POINT('Origin',(0.,5.5,0.));
#18168=CARTESIAN_POINT('',(-1.1,4.7,1.34711147906209E-16));
#18169=CARTESIAN_POINT('',(-1.1,4.7,1.34711147906209E-16));
#18170=CARTESIAN_POINT('Origin',(0.,4.7,0.));
#18171=CARTESIAN_POINT('Origin',(0.,5.5,0.));
#18172=CARTESIAN_POINT('Origin',(0.,4.7,0.));
#18173=CARTESIAN_POINT('',(0.,0.,0.));
#18174=CARTESIAN_POINT('Origin',(0.,4.,0.));
#18175=CARTESIAN_POINT('',(-0.61,4.7,7.47034547479885E-17));
#18176=CARTESIAN_POINT('Origin',(0.,4.7,0.));
#18177=CARTESIAN_POINT('',(-0.61,4.,7.47034547479885E-17));
#18178=CARTESIAN_POINT('',(-0.61,4.,7.47034547479885E-17));
#18179=CARTESIAN_POINT('Origin',(0.,4.,0.));
#18180=CARTESIAN_POINT('Origin',(0.,4.,0.));
#18181=CARTESIAN_POINT('',(-0.9,4.7,1.10218211923262E-16));
#18182=CARTESIAN_POINT('Origin',(0.,4.7,0.));
#18183=CARTESIAN_POINT('',(-0.9,4.,1.10218211923262E-16));
#18184=CARTESIAN_POINT('',(-0.9,4.,1.10218211923262E-16));
#18185=CARTESIAN_POINT('Origin',(0.,4.,0.));
#18186=CARTESIAN_POINT('Origin',(0.,4.7,0.));
#18187=CARTESIAN_POINT('Origin',(0.,4.,0.));
#18188=CARTESIAN_POINT('',(0.,0.,0.));
#18189=CARTESIAN_POINT('Origin',(0.2,0.,0.));
#18190=CARTESIAN_POINT('',(0.2,2.2,-0.78));
#18191=CARTESIAN_POINT('',(0.2,2.2,-0.565685424949238));
#18192=CARTESIAN_POINT('',(0.2,2.2,0.));
#18193=CARTESIAN_POINT('',(0.2,-1.,-0.78));
#18194=CARTESIAN_POINT('',(0.2,0.,-0.78));
#18195=CARTESIAN_POINT('',(0.2,-1.,-0.565685424949238));
#18196=CARTESIAN_POINT('',(0.2,-1.,0.));
#18197=CARTESIAN_POINT('',(0.2,0.,-0.565685424949238));
#18198=CARTESIAN_POINT('Origin',(0.2,0.,-0.78));
#18199=CARTESIAN_POINT('',(-0.2,2.2,-0.78));
#18200=CARTESIAN_POINT('',(0.1,2.2,-0.78));
#18201=CARTESIAN_POINT('',(-0.2,-1.,-0.78));
#18202=CARTESIAN_POINT('',(-0.2,0.,-0.78));
#18203=CARTESIAN_POINT('',(0.1,-1.,-0.78));
#18204=CARTESIAN_POINT('Origin',(-0.2,0.,-0.78));
#18205=CARTESIAN_POINT('',(-0.2,2.2,-0.565685424949238));
#18206=CARTESIAN_POINT('',(-0.2,2.2,-0.39));
#18207=CARTESIAN_POINT('',(-0.2,-1.,-0.565685424949238));
#18208=CARTESIAN_POINT('',(-0.2,0.,-0.565685424949238));
#18209=CARTESIAN_POINT('',(-0.2,-1.,-0.39));
#18210=CARTESIAN_POINT('Origin',(0.,-1.,0.));
#18211=CARTESIAN_POINT('',(1.60662857109684,-1.,0.693717979106306));
#18212=CARTESIAN_POINT('',(1.5055822144029,-1.,0.892032620296856));
#18213=CARTESIAN_POINT('Origin',(0.,-1.,0.));
#18214=CARTESIAN_POINT('',(1.81978687191668,-1.,1.23627494547115));
#18215=CARTESIAN_POINT('Ctrl Pts',(1.5055822144029,-1.,0.892032620296856));
#18216=CARTESIAN_POINT('Ctrl Pts',(1.50980486806688,-1.,0.894452006964544));
#18217=CARTESIAN_POINT('Ctrl Pts',(1.51805569590094,-1.,0.899185047483511));
#18218=CARTESIAN_POINT('Ctrl Pts',(1.52984849887993,-1.,0.905967409625651));
#18219=CARTESIAN_POINT('Ctrl Pts',(1.54440491149498,-1.,0.914375919026456));
#18220=CARTESIAN_POINT('Ctrl Pts',(1.56065988578893,-1.,0.923832188944341));
#18221=CARTESIAN_POINT('Ctrl Pts',(1.57499388382243,-1.,0.932246680108685));
#18222=CARTESIAN_POINT('Ctrl Pts',(1.58744937487176,-1.,0.939646377893399));
#18223=CARTESIAN_POINT('Ctrl Pts',(1.59810042043673,-1.,0.946078063315257));
#18224=CARTESIAN_POINT('Ctrl Pts',(1.60706069896936,-1.,0.951613284356035));
#18225=CARTESIAN_POINT('Ctrl Pts',(1.61449324337085,-1.,0.956354422920671));
#18226=CARTESIAN_POINT('Ctrl Pts',(1.62061638140221,-1.,0.960438326101729));
#18227=CARTESIAN_POINT('Ctrl Pts',(1.62571930670187,-1.,0.964046107040536));
#18228=CARTESIAN_POINT('Ctrl Pts',(1.63013849959461,-1.,0.967387853230345));
#18229=CARTESIAN_POINT('Ctrl Pts',(1.63420665729798,-1.,0.970669715997509));
#18230=CARTESIAN_POINT('Ctrl Pts',(1.63820952658144,-1.,0.974066058287419));
#18231=CARTESIAN_POINT('Ctrl Pts',(1.64233990826687,-1.,0.977689794119417));
#18232=CARTESIAN_POINT('Ctrl Pts',(1.64665139190656,-1.,0.981562530939489));
#18233=CARTESIAN_POINT('Ctrl Pts',(1.65110016612638,-1.,0.985642622920821));
#18234=CARTESIAN_POINT('Ctrl Pts',(1.65559044289699,-1.,0.989855627854165));
#18235=CARTESIAN_POINT('Ctrl Pts',(1.66001553809947,-1.,0.994121836661306));
#18236=CARTESIAN_POINT('Ctrl Pts',(1.66430758030376,-1.,0.998389654952758));
#18237=CARTESIAN_POINT('Ctrl Pts',(1.66846059277303,-1.,1.00265091003727));
#18238=CARTESIAN_POINT('Ctrl Pts',(1.67250335383293,-1.,1.00692206696414));
#18239=CARTESIAN_POINT('Ctrl Pts',(1.67648246776464,-1.,1.01123236493511));
#18240=CARTESIAN_POINT('Ctrl Pts',(1.68044289894798,-1.,1.01561026162773));
#18241=CARTESIAN_POINT('Ctrl Pts',(1.68440578021706,-1.,1.02006795074201));
#18242=CARTESIAN_POINT('Ctrl Pts',(1.68836910178447,-1.,1.02460180535255));
#18243=CARTESIAN_POINT('Ctrl Pts',(1.69231840863458,-1.,1.02919977579147));
#18244=CARTESIAN_POINT('Ctrl Pts',(1.69623414782771,-1.,1.03384646003588));
#18245=CARTESIAN_POINT('Ctrl Pts',(1.70010052930962,-1.,1.03852922490789));
#18246=CARTESIAN_POINT('Ctrl Pts',(1.70391338707982,-1.,1.04324363334554));
#18247=CARTESIAN_POINT('Ctrl Pts',(1.70767646263649,-1.,1.04799085404995));
#18248=CARTESIAN_POINT('Ctrl Pts',(1.71139783543989,-1.,1.05277517202855));
#18249=CARTESIAN_POINT('Ctrl Pts',(1.7150865442702,-1.,1.05760163192479));
#18250=CARTESIAN_POINT('Ctrl Pts',(1.71874858456904,-1.,1.06247324680647));
#18251=CARTESIAN_POINT('Ctrl Pts',(1.72238500928453,-1.,1.06738966975462));
#18252=CARTESIAN_POINT('Ctrl Pts',(1.72599406198488,-1.,1.07234866990252));
#18253=CARTESIAN_POINT('Ctrl Pts',(1.72957248977424,-1.,1.0773470373727));
#18254=CARTESIAN_POINT('Ctrl Pts',(1.73311705663407,-1.,1.08238162784749));
#18255=CARTESIAN_POINT('Ctrl Pts',(1.73662628326091,-1.,1.08745056285427));
#18256=CARTESIAN_POINT('Ctrl Pts',(1.74010053962247,-1.,1.09255329056493));
#18257=CARTESIAN_POINT('Ctrl Pts',(1.74354119236208,-1.,1.09768999241226));
#18258=CARTESIAN_POINT('Ctrl Pts',(1.74695004214923,-1.,1.10286118991143));
#18259=CARTESIAN_POINT('Ctrl Pts',(1.7503286607592,-1.,1.10806728183007));
#18260=CARTESIAN_POINT('Ctrl Pts',(1.7536777209463,-1.,1.11330807582551));
#18261=CARTESIAN_POINT('Ctrl Pts',(1.75699720772105,-1.,1.11858293216763));
#18262=CARTESIAN_POINT('Ctrl Pts',(1.76028671825096,-1.,1.12389096855086));
#18263=CARTESIAN_POINT('Ctrl Pts',(1.7635457196617,-1.,1.12923123555075));
#18264=CARTESIAN_POINT('Ctrl Pts',(1.76677384551862,-1.,1.1346029180462));
#18265=CARTESIAN_POINT('Ctrl Pts',(1.76997111386769,-1.,1.14000548336975));
#18266=CARTESIAN_POINT('Ctrl Pts',(1.77313777896194,-1.,1.1454385822692));
#18267=CARTESIAN_POINT('Ctrl Pts',(1.7762742255701,-1.,1.15090197841515));
#18268=CARTESIAN_POINT('Ctrl Pts',(1.77938085564275,-1.,1.15639547194698));
#18269=CARTESIAN_POINT('Ctrl Pts',(1.78245795881009,-1.,1.16191881298499));
#18270=CARTESIAN_POINT('Ctrl Pts',(1.78550566040443,-1.,1.16747166312303));
#18271=CARTESIAN_POINT('Ctrl Pts',(1.78852398877616,-1.,1.17305363177328));
#18272=CARTESIAN_POINT('Ctrl Pts',(1.79151291552689,-1.,1.17866429440809));
#18273=CARTESIAN_POINT('Ctrl Pts',(1.79447240321515,-1.,1.18430321697432));
#18274=CARTESIAN_POINT('Ctrl Pts',(1.79740245923478,-1.,1.18996997934445));
#18275=CARTESIAN_POINT('Ctrl Pts',(1.80030314369879,-1.,1.19566418930242));
#18276=CARTESIAN_POINT('Ctrl Pts',(1.80317454838603,-1.,1.20138548938974));
#18277=CARTESIAN_POINT('Ctrl Pts',(1.80601678480707,-1.,1.20713356605475));
#18278=CARTESIAN_POINT('Ctrl Pts',(1.80882996917129,-1.,1.21290815708314));
#18279=CARTESIAN_POINT('Ctrl Pts',(1.81161420806656,-1.,1.21870906103557));
#18280=CARTESIAN_POINT('Ctrl Pts',(1.81436959210434,-1.,1.2245361330495));
#18281=CARTESIAN_POINT('Ctrl Pts',(1.8165508718364,-1.,1.2292186489137));
#18282=CARTESIAN_POINT('Ctrl Pts',(1.81817389921279,-1.,1.2327422452705));
#18283=CARTESIAN_POINT('Ctrl Pts',(1.81925017193666,-1.,1.23509651170476));
#18284=CARTESIAN_POINT('Ctrl Pts',(1.81978687191668,-1.,1.23627494547115));
#18285=CARTESIAN_POINT('',(1.73811241238545,-1.,1.34869019493419));
#18286=CARTESIAN_POINT('',(1.81978687191668,-1.,1.23627494547115));
#18287=CARTESIAN_POINT('',(1.31362392696032,-1.,1.15624053661742));
#18288=CARTESIAN_POINT('Ctrl Pts',(1.73811241238545,-1.,1.34869019493419));
#18289=CARTESIAN_POINT('Ctrl Pts',(1.73682580585691,-1.,1.34854391898045));
#18290=CARTESIAN_POINT('Ctrl Pts',(1.73425417885907,-1.,1.34824783112887));
#18291=CARTESIAN_POINT('Ctrl Pts',(1.7304014965394,-1.,1.34779309152035));
#18292=CARTESIAN_POINT('Ctrl Pts',(1.72527410680674,-1.,1.34716554819527));
#18293=CARTESIAN_POINT('Ctrl Pts',(1.7188807715049,-1.,1.34634568653227));
#18294=CARTESIAN_POINT('Ctrl Pts',(1.71250340686822,-1.,1.34549029589416));
#18295=CARTESIAN_POINT('Ctrl Pts',(1.70614212266738,-1.,1.34459924533831));
#18296=CARTESIAN_POINT('Ctrl Pts',(1.69979707754427,-1.,1.34367237124483));
#18297=CARTESIAN_POINT('Ctrl Pts',(1.6934684849687,-1.,1.34270948206319));
#18298=CARTESIAN_POINT('Ctrl Pts',(1.68715660868764,-1.,1.341710374848));
#18299=CARTESIAN_POINT('Ctrl Pts',(1.68086176030362,-1.,1.34067485185203));
#18300=CARTESIAN_POINT('Ctrl Pts',(1.67458429426086,-1.,1.3396027347034));
#18301=CARTESIAN_POINT('Ctrl Pts',(1.66832460783989,-1.,1.33849388654388));
#18302=CARTESIAN_POINT('Ctrl Pts',(1.66208312541983,-1.,1.33734820885262));
#18303=CARTESIAN_POINT('Ctrl Pts',(1.65586025952593,-1.,1.33616559745172));
#18304=CARTESIAN_POINT('Ctrl Pts',(1.6496563728683,-1.,1.33494590467993));
#18305=CARTESIAN_POINT('Ctrl Pts',(1.6434717485603,-1.,1.33368890676572));
#18306=CARTESIAN_POINT('Ctrl Pts',(1.63730653475089,-1.,1.33239425103724));
#18307=CARTESIAN_POINT('Ctrl Pts',(1.63116079730923,-1.,1.33106149345645));
#18308=CARTESIAN_POINT('Ctrl Pts',(1.62503464209797,-1.,1.3296901950568));
#18309=CARTESIAN_POINT('Ctrl Pts',(1.61892832270724,-1.,1.32828000610449));
#18310=CARTESIAN_POINT('Ctrl Pts',(1.6128423401575,-1.,1.32683074483356));
#18311=CARTESIAN_POINT('Ctrl Pts',(1.60677758290954,-1.,1.32534250785782));
#18312=CARTESIAN_POINT('Ctrl Pts',(1.60073511858687,-1.,1.32381550858256));
#18313=CARTESIAN_POINT('Ctrl Pts',(1.59471591079403,-1.,1.32224985747682));
#18314=CARTESIAN_POINT('Ctrl Pts',(1.58872057258245,-1.,1.32064537110892));
#18315=CARTESIAN_POINT('Ctrl Pts',(1.58274907898834,-1.,1.31900135021432));
#18316=CARTESIAN_POINT('Ctrl Pts',(1.5768005650559,-1.,1.31731642317187));
#18317=CARTESIAN_POINT('Ctrl Pts',(1.57087397835723,-1.,1.31558903860016));
#18318=CARTESIAN_POINT('Ctrl Pts',(1.56496872402353,-1.,1.31381795281002));
#18319=CARTESIAN_POINT('Ctrl Pts',(1.55908521254821,-1.,1.31200264341696));
#18320=CARTESIAN_POINT('Ctrl Pts',(1.55322568759481,-1.,1.31014393684222));
#18321=CARTESIAN_POINT('Ctrl Pts',(1.54739413957185,-1.,1.30824393907473));
#18322=CARTESIAN_POINT('Ctrl Pts',(1.54159462645432,-1.,1.30630475189556));
#18323=CARTESIAN_POINT('Ctrl Pts',(1.53582981268977,-1.,1.30432735639489));
#18324=CARTESIAN_POINT('Ctrl Pts',(1.53009970283891,-1.,1.30231064395568));
#18325=CARTESIAN_POINT('Ctrl Pts',(1.52439957861062,-1.,1.30024984366328));
#18326=CARTESIAN_POINT('Ctrl Pts',(1.51872184912724,-1.,1.29813791800747));
#18327=CARTESIAN_POINT('Ctrl Pts',(1.51305994241402,-1.,1.29596850710509));
#18328=CARTESIAN_POINT('Ctrl Pts',(1.50741159078365,-1.,1.29373841372842));
#18329=CARTESIAN_POINT('Ctrl Pts',(1.50178230149776,-1.,1.29145022885181));
#18330=CARTESIAN_POINT('Ctrl Pts',(1.49618896881754,-1.,1.28911506584254));
#18331=CARTESIAN_POINT('Ctrl Pts',(1.4906522831278,-1.,1.2867467611644));
#18332=CARTESIAN_POINT('Ctrl Pts',(1.4851881711891,-1.,1.28435533880201));
#18333=CARTESIAN_POINT('Ctrl Pts',(1.47980070347095,-1.,1.28194158939517));
#18334=CARTESIAN_POINT('Ctrl Pts',(1.4744717526707,-1.,1.2794891824849));
#18335=CARTESIAN_POINT('Ctrl Pts',(1.46916035917133,-1.,1.2769641483109));
#18336=CARTESIAN_POINT('Ctrl Pts',(1.46382431332476,-1.,1.27433119897822));
#18337=CARTESIAN_POINT('Ctrl Pts',(1.45843906294697,-1.,1.27156805265289));
#18338=CARTESIAN_POINT('Ctrl Pts',(1.45301422764247,-1.,1.2686778680489));
#18339=CARTESIAN_POINT('Ctrl Pts',(1.44761985001662,-1.,1.26570925118868));
#18340=CARTESIAN_POINT('Ctrl Pts',(1.44236470511303,-1.,1.26273903323859));
#18341=CARTESIAN_POINT('Ctrl Pts',(1.43734919180847,-1.,1.25983531012005));
#18342=CARTESIAN_POINT('Ctrl Pts',(1.43262645609691,-1.,1.25702687965755));
#18343=CARTESIAN_POINT('Ctrl Pts',(1.42815938799387,-1.,1.25426945222639));
#18344=CARTESIAN_POINT('Ctrl Pts',(1.42378102115575,-1.,1.2514145557001));
#18345=CARTESIAN_POINT('Ctrl Pts',(1.41923722596025,-1.,1.24824430986571));
#18346=CARTESIAN_POINT('Ctrl Pts',(1.41422913175179,-1.,1.24450600513056));
#18347=CARTESIAN_POINT('Ctrl Pts',(1.40845295531283,-1.,1.23994455029534));
#18348=CARTESIAN_POINT('Ctrl Pts',(1.40164708206106,-1.,1.23434087290423));
#18349=CARTESIAN_POINT('Ctrl Pts',(1.39361389568796,-1.,1.22752961899387));
#18350=CARTESIAN_POINT('Ctrl Pts',(1.38420564527715,-1.,1.21938737280852));
#18351=CARTESIAN_POINT('Ctrl Pts',(1.37331915607905,-1.,1.20982812925645));
#18352=CARTESIAN_POINT('Ctrl Pts',(1.36088705043885,-1.,1.1987959077932));
#18353=CARTESIAN_POINT('Ctrl Pts',(1.34687054001093,-1.,1.18625865667441));
#18354=CARTESIAN_POINT('Ctrl Pts',(1.33437539347008,-1.,1.17501305789857));
#18355=CARTESIAN_POINT('Ctrl Pts',(1.32428080721772,-1.,1.16589330093588));
#18356=CARTESIAN_POINT('Ctrl Pts',(1.31722977216397,-1.,1.15950888730809));
#18357=CARTESIAN_POINT('Ctrl Pts',(1.31362392696032,-1.,1.15624053661742));
#18358=CARTESIAN_POINT('',(1.15624053661742,-1.,1.31362392696033));
#18359=CARTESIAN_POINT('Origin',(0.,-1.,0.));
#18360=CARTESIAN_POINT('',(1.34869019493419,-1.,1.73811241238545));
#18361=CARTESIAN_POINT('Ctrl Pts',(1.15624053661742,-1.,1.31362392696033));
#18362=CARTESIAN_POINT('Ctrl Pts',(1.15950888730433,-1.,1.3172297721596));
#18363=CARTESIAN_POINT('Ctrl Pts',(1.16589330092532,-1.,1.32428080720544));
#18364=CARTESIAN_POINT('Ctrl Pts',(1.17501305787994,-1.,1.33437539344842));
#18365=CARTESIAN_POINT('Ctrl Pts',(1.18625865664915,-1.,1.34687053998157));
#18366=CARTESIAN_POINT('Ctrl Pts',(1.1987959077656,-1.,1.36088705040677));
#18367=CARTESIAN_POINT('Ctrl Pts',(1.20982812923113,-1.,1.37331915604962));
#18368=CARTESIAN_POINT('Ctrl Pts',(1.21938737278853,-1.,1.38420564525391));
#18369=CARTESIAN_POINT('Ctrl Pts',(1.22752961898063,-1.,1.39361389567257));
#18370=CARTESIAN_POINT('Ctrl Pts',(1.23434087289768,-1.,1.40164708205345));
#18371=CARTESIAN_POINT('Ctrl Pts',(1.23994455029421,-1.,1.40845295531151));
#18372=CARTESIAN_POINT('Ctrl Pts',(1.24450600513278,-1.,1.41422913175437));
#18373=CARTESIAN_POINT('Ctrl Pts',(1.24824430986911,-1.,1.41923722596421));
#18374=CARTESIAN_POINT('Ctrl Pts',(1.25141455570299,-1.,1.42378102115911));
#18375=CARTESIAN_POINT('Ctrl Pts',(1.25426945222783,-1.,1.42815938799555));
#18376=CARTESIAN_POINT('Ctrl Pts',(1.25702687965744,-1.,1.43262645609679));
#18377=CARTESIAN_POINT('Ctrl Pts',(1.25983531011894,-1.,1.43734919180719));
#18378=CARTESIAN_POINT('Ctrl Pts',(1.26273903323723,-1.,1.44236470511145));
#18379=CARTESIAN_POINT('Ctrl Pts',(1.26570925118767,-1.,1.44761985001544));
#18380=CARTESIAN_POINT('Ctrl Pts',(1.26867786804854,-1.,1.45301422764205));
#18381=CARTESIAN_POINT('Ctrl Pts',(1.27156805265312,-1.,1.45843906294725));
#18382=CARTESIAN_POINT('Ctrl Pts',(1.27433119897877,-1.,1.4638243133254));
#18383=CARTESIAN_POINT('Ctrl Pts',(1.27696414831144,-1.,1.46916035917197));
#18384=CARTESIAN_POINT('Ctrl Pts',(1.27948918248524,-1.,1.4744717526711));
#18385=CARTESIAN_POINT('Ctrl Pts',(1.28194158939522,-1.,1.47980070347102));
#18386=CARTESIAN_POINT('Ctrl Pts',(1.28435533880184,-1.,1.48518817118891));
#18387=CARTESIAN_POINT('Ctrl Pts',(1.28674676116415,-1.,1.4906522831275));
#18388=CARTESIAN_POINT('Ctrl Pts',(1.28911506584232,-1.,1.49618896881729));
#18389=CARTESIAN_POINT('Ctrl Pts',(1.29145022885171,-1.,1.50178230149764));
#18390=CARTESIAN_POINT('Ctrl Pts',(1.29373841372843,-1.,1.50741159078367));
#18391=CARTESIAN_POINT('Ctrl Pts',(1.29596850710518,-1.,1.51305994241412));
#18392=CARTESIAN_POINT('Ctrl Pts',(1.29813791800757,-1.,1.51872184912735));
#18393=CARTESIAN_POINT('Ctrl Pts',(1.30024984366334,-1.,1.5243995786107));
#18394=CARTESIAN_POINT('Ctrl Pts',(1.3023106439557,-1.,1.53009970283893));
#18395=CARTESIAN_POINT('Ctrl Pts',(1.30432735639487,-1.,1.53582981268976));
#18396=CARTESIAN_POINT('Ctrl Pts',(1.30630475189553,-1.,1.54159462645428));
#18397=CARTESIAN_POINT('Ctrl Pts',(1.30824393907471,-1.,1.54739413957183));
#18398=CARTESIAN_POINT('Ctrl Pts',(1.31014393684221,-1.,1.55322568759481));
#18399=CARTESIAN_POINT('Ctrl Pts',(1.31200264341696,-1.,1.55908521254822));
#18400=CARTESIAN_POINT('Ctrl Pts',(1.31381795281002,-1.,1.56496872402352));
#18401=CARTESIAN_POINT('Ctrl Pts',(1.31558903860015,-1.,1.57087397835721));
#18402=CARTESIAN_POINT('Ctrl Pts',(1.31731642317183,-1.,1.57680056505585));
#18403=CARTESIAN_POINT('Ctrl Pts',(1.31900135021428,-1.,1.58274907898829));
#18404=CARTESIAN_POINT('Ctrl Pts',(1.32064537110891,-1.,1.58872057258244));
#18405=CARTESIAN_POINT('Ctrl Pts',(1.32224985747686,-1.,1.59471591079408));
#18406=CARTESIAN_POINT('Ctrl Pts',(1.32381550858266,-1.,1.600735118587));
#18407=CARTESIAN_POINT('Ctrl Pts',(1.32534250785794,-1.,1.6067775829097));
#18408=CARTESIAN_POINT('Ctrl Pts',(1.32683074483365,-1.,1.61284234015762));
#18409=CARTESIAN_POINT('Ctrl Pts',(1.32828000610448,-1.,1.61892832270723));
#18410=CARTESIAN_POINT('Ctrl Pts',(1.32969019505665,-1.,1.62503464209777));
#18411=CARTESIAN_POINT('Ctrl Pts',(1.33106149345618,-1.,1.63116079730887));
#18412=CARTESIAN_POINT('Ctrl Pts',(1.33239425103694,-1.,1.6373065347505));
#18413=CARTESIAN_POINT('Ctrl Pts',(1.33368890676554,-1.,1.64347174856007));
#18414=CARTESIAN_POINT('Ctrl Pts',(1.33494590468003,-1.,1.64965637286843));
#18415=CARTESIAN_POINT('Ctrl Pts',(1.33616559745217,-1.,1.65586025952651));
#18416=CARTESIAN_POINT('Ctrl Pts',(1.33734820885331,-1.,1.66208312542073));
#18417=CARTESIAN_POINT('Ctrl Pts',(1.33849388654458,-1.,1.66832460784078));
#18418=CARTESIAN_POINT('Ctrl Pts',(1.33960273470372,-1.,1.67458429426126));
#18419=CARTESIAN_POINT('Ctrl Pts',(1.3406748518516,-1.,1.68086176030308));
#18420=CARTESIAN_POINT('Ctrl Pts',(1.34171037484673,-1.,1.68715660868602));
#18421=CARTESIAN_POINT('Ctrl Pts',(1.34270948206139,-1.,1.6934684849664));
#18422=CARTESIAN_POINT('Ctrl Pts',(1.34367237124322,-1.,1.69979707754221));
#18423=CARTESIAN_POINT('Ctrl Pts',(1.34459924533783,-1.,1.70614212266676));
#18424=CARTESIAN_POINT('Ctrl Pts',(1.34549029589563,-1.,1.71250340687011));
#18425=CARTESIAN_POINT('Ctrl Pts',(1.34634568653586,-1.,1.7188807715095));
#18426=CARTESIAN_POINT('Ctrl Pts',(1.34716554820013,-1.,1.72527410681298));
#18427=CARTESIAN_POINT('Ctrl Pts',(1.3477930915247,-1.,1.73040149654497));
#18428=CARTESIAN_POINT('Ctrl Pts',(1.34824783113158,-1.,1.73425417886255));
#18429=CARTESIAN_POINT('Ctrl Pts',(1.34854391898145,-1.,1.73682580585819));
#18430=CARTESIAN_POINT('Ctrl Pts',(1.34869019493419,-1.,1.73811241238545));
#18431=CARTESIAN_POINT('',(1.23627494547115,-1.,1.81978687191668));
#18432=CARTESIAN_POINT('',(1.34869019493419,-1.,1.73811241238545));
#18433=CARTESIAN_POINT('',(0.892032620296855,-1.,1.5055822144029));
#18434=CARTESIAN_POINT('Ctrl Pts',(1.23627494547115,-1.,1.81978687191668));
#18435=CARTESIAN_POINT('Ctrl Pts',(1.23509651170384,-1.,1.81925017193531));
#18436=CARTESIAN_POINT('Ctrl Pts',(1.23274224526804,-1.,1.81817389920914));
#18437=CARTESIAN_POINT('Ctrl Pts',(1.22921864890975,-1.,1.81655087183054));
#18438=CARTESIAN_POINT('Ctrl Pts',(1.22453613304507,-1.,1.81436959209778));
#18439=CARTESIAN_POINT('Ctrl Pts',(1.2187090610323,-1.,1.81161420806172));
#18440=CARTESIAN_POINT('Ctrl Pts',(1.2129081570818,-1.,1.80882996916931));
#18441=CARTESIAN_POINT('Ctrl Pts',(1.20713356605519,-1.,1.80601678480772));
#18442=CARTESIAN_POINT('Ctrl Pts',(1.2013854893912,-1.,1.8031745483882));
#18443=CARTESIAN_POINT('Ctrl Pts',(1.19566418930405,-1.,1.80030314370121));
#18444=CARTESIAN_POINT('Ctrl Pts',(1.1899699793456,-1.,1.79740245923649));
#18445=CARTESIAN_POINT('Ctrl Pts',(1.18430321697471,-1.,1.79447240321572));
#18446=CARTESIAN_POINT('Ctrl Pts',(1.17866429440781,-1.,1.79151291552646));
#18447=CARTESIAN_POINT('Ctrl Pts',(1.17305363177265,-1.,1.78852398877523));
#18448=CARTESIAN_POINT('Ctrl Pts',(1.16747166312239,-1.,1.78550566040349));
#18449=CARTESIAN_POINT('Ctrl Pts',(1.16191881298458,-1.,1.78245795880949));
#18450=CARTESIAN_POINT('Ctrl Pts',(1.15639547194689,-1.,1.77938085564261));
#18451=CARTESIAN_POINT('Ctrl Pts',(1.15090197841531,-1.,1.77627422557034));
#18452=CARTESIAN_POINT('Ctrl Pts',(1.14543858226948,-1.,1.77313777896234));
#18453=CARTESIAN_POINT('Ctrl Pts',(1.14000548337,-1.,1.76997111386806));
#18454=CARTESIAN_POINT('Ctrl Pts',(1.13460291804634,-1.,1.76677384551883));
#18455=CARTESIAN_POINT('Ctrl Pts',(1.12923123555076,-1.,1.76354571966171));
#18456=CARTESIAN_POINT('Ctrl Pts',(1.12389096855078,-1.,1.76028671825084));
#18457=CARTESIAN_POINT('Ctrl Pts',(1.11858293216752,-1.,1.75699720772089));
#18458=CARTESIAN_POINT('Ctrl Pts',(1.11330807582542,-1.,1.75367772094617));
#18459=CARTESIAN_POINT('Ctrl Pts',(1.10806728183003,-1.,1.75032866075914));
#18460=CARTESIAN_POINT('Ctrl Pts',(1.10286118991144,-1.,1.74695004214924));
#18461=CARTESIAN_POINT('Ctrl Pts',(1.09768999241229,-1.,1.74354119236212));
#18462=CARTESIAN_POINT('Ctrl Pts',(1.09255329056496,-1.,1.74010053962252));
#18463=CARTESIAN_POINT('Ctrl Pts',(1.08745056285429,-1.,1.73662628326093));
#18464=CARTESIAN_POINT('Ctrl Pts',(1.08238162784749,-1.,1.73311705663407));
#18465=CARTESIAN_POINT('Ctrl Pts',(1.0773470373727,-1.,1.72957248977424));
#18466=CARTESIAN_POINT('Ctrl Pts',(1.07234866990252,-1.,1.72599406198489));
#18467=CARTESIAN_POINT('Ctrl Pts',(1.06738966975463,-1.,1.72238500928456));
#18468=CARTESIAN_POINT('Ctrl Pts',(1.06247324680649,-1.,1.71874858456908));
#18469=CARTESIAN_POINT('Ctrl Pts',(1.05760163192481,-1.,1.71508654427022));
#18470=CARTESIAN_POINT('Ctrl Pts',(1.05277517202853,-1.,1.71139783543986));
#18471=CARTESIAN_POINT('Ctrl Pts',(1.0479908540499,-1.,1.70767646263641));
#18472=CARTESIAN_POINT('Ctrl Pts',(1.04324363334546,-1.,1.70391338707969));
#18473=CARTESIAN_POINT('Ctrl Pts',(1.03852922490782,-1.,1.70010052930951));
#18474=CARTESIAN_POINT('Ctrl Pts',(1.03384646003587,-1.,1.69623414782769));
#18475=CARTESIAN_POINT('Ctrl Pts',(1.02919977579155,-1.,1.69231840863471));
#18476=CARTESIAN_POINT('Ctrl Pts',(1.02460180535272,-1.,1.68836910178475));
#18477=CARTESIAN_POINT('Ctrl Pts',(1.02006795074222,-1.,1.68440578021739));
#18478=CARTESIAN_POINT('Ctrl Pts',(1.01561026162786,-1.,1.6804428989482));
#18479=CARTESIAN_POINT('Ctrl Pts',(1.01123236493507,-1.,1.67648246776457));
#18480=CARTESIAN_POINT('Ctrl Pts',(1.00692206696387,-1.,1.67250335383248));
#18481=CARTESIAN_POINT('Ctrl Pts',(1.00265091003682,-1.,1.66846059277231));
#18482=CARTESIAN_POINT('Ctrl Pts',(0.998389654952317,-1.,1.66430758030304));
#18483=CARTESIAN_POINT('Ctrl Pts',(0.994121836661115,-1.,1.66001553809916));
#18484=CARTESIAN_POINT('Ctrl Pts',(0.98985562785445,-1.,1.65559044289746));
#18485=CARTESIAN_POINT('Ctrl Pts',(0.985642622921626,-1.,1.6511001661277));
#18486=CARTESIAN_POINT('Ctrl Pts',(0.981562530940574,-1.,1.64665139190834));
#18487=CARTESIAN_POINT('Ctrl Pts',(0.977689794120296,-1.,1.64233990826831));
#18488=CARTESIAN_POINT('Ctrl Pts',(0.974066058287501,-1.,1.63820952658157));
#18489=CARTESIAN_POINT('Ctrl Pts',(0.970669715996356,-1.,1.63420665729609));
#18490=CARTESIAN_POINT('Ctrl Pts',(0.967387853228041,-1.,1.63013849959083));
#18491=CARTESIAN_POINT('Ctrl Pts',(0.964046107037821,-1.,1.6257193066974));
#18492=CARTESIAN_POINT('Ctrl Pts',(0.960438326099958,-1.,1.62061638139929));
#18493=CARTESIAN_POINT('Ctrl Pts',(0.956354422921572,-1.,1.61449324337233));
#18494=CARTESIAN_POINT('Ctrl Pts',(0.951613284361247,-1.,1.60706069897794));
#18495=CARTESIAN_POINT('Ctrl Pts',(0.946078063325795,-1.,1.59810042045408));
#18496=CARTESIAN_POINT('Ctrl Pts',(0.939646377909319,-1.,1.58744937489796));
#18497=CARTESIAN_POINT('Ctrl Pts',(0.932246680128848,-1.,1.57499388385561));
#18498=CARTESIAN_POINT('Ctrl Pts',(0.923832188966322,-1.,1.56065988582509));
#18499=CARTESIAN_POINT('Ctrl Pts',(0.914375919046579,-1.,1.54440491152808));
#18500=CARTESIAN_POINT('Ctrl Pts',(0.905967409640498,-1.,1.52984849890434));
#18501=CARTESIAN_POINT('Ctrl Pts',(0.89918504749193,-1.,1.51805569591479));
#18502=CARTESIAN_POINT('Ctrl Pts',(0.894452006967538,-1.,1.50980486807181));
#18503=CARTESIAN_POINT('Ctrl Pts',(0.892032620296855,-1.,1.5055822144029));
#18504=CARTESIAN_POINT('',(0.693717979106305,-1.,1.60662857109684));
#18505=CARTESIAN_POINT('Origin',(0.,-1.,0.));
#18506=CARTESIAN_POINT('',(0.7455743247944,-1.,2.0698113262342));
#18507=CARTESIAN_POINT('Ctrl Pts',(0.693717979106305,-1.,1.60662857109684));
#18508=CARTESIAN_POINT('Ctrl Pts',(0.69571209787897,-1.,1.61106790957619));
#18509=CARTESIAN_POINT('Ctrl Pts',(0.699605146398836,-1.,1.61974673471117));
#18510=CARTESIAN_POINT('Ctrl Pts',(0.705159151977294,-1.,1.6321654166204));
#18511=CARTESIAN_POINT('Ctrl Pts',(0.711993139340447,-1.,1.64752408828442));
#18512=CARTESIAN_POINT('Ctrl Pts',(0.719585433787949,-1.,1.66472880551777));
#18513=CARTESIAN_POINT('Ctrl Pts',(0.726235967982445,-1.,1.67996158451922));
#18514=CARTESIAN_POINT('Ctrl Pts',(0.731963238685357,-1.,1.69326921972915));
#18515=CARTESIAN_POINT('Ctrl Pts',(0.736799665716932,-1.,1.70473309004249));
#18516=CARTESIAN_POINT('Ctrl Pts',(0.74079516202821,-1.,1.71447789751001));
#18517=CARTESIAN_POINT('Ctrl Pts',(0.744021445433093,-1.,1.72268229916769));
#18518=CARTESIAN_POINT('Ctrl Pts',(0.746574710097752,-1.,1.72958533647714));
#18519=CARTESIAN_POINT('Ctrl Pts',(0.74858246295687,-1.,1.7355035168033));
#18520=CARTESIAN_POINT('Ctrl Pts',(0.750193435981249,-1.,1.74080458267114));
#18521=CARTESIAN_POINT('Ctrl Pts',(0.751555614164482,-1.,1.74585086852502));
#18522=CARTESIAN_POINT('Ctrl Pts',(0.752797683531314,-1.,1.75095139468794));
#18523=CARTESIAN_POINT('Ctrl Pts',(0.754009254027828,-1.,1.75631083600019));
#18524=CARTESIAN_POINT('Ctrl Pts',(0.755220979974461,-1.,1.76197817240128));
#18525=CARTESIAN_POINT('Ctrl Pts',(0.75642189602781,-1.,1.76789396002998));
#18526=CARTESIAN_POINT('Ctrl Pts',(0.757578264077028,-1.,1.77394167108292));
#18527=CARTESIAN_POINT('Ctrl Pts',(0.758650626677518,-1.,1.77999411220945));
#18528=CARTESIAN_POINT('Ctrl Pts',(0.759614401110189,-1.,1.78596964884604));
#18529=CARTESIAN_POINT('Ctrl Pts',(0.760469555880749,-1.,1.7918581561088));
#18530=CARTESIAN_POINT('Ctrl Pts',(0.761229695230558,-1.,1.79768986997783));
#18531=CARTESIAN_POINT('Ctrl Pts',(0.761915336443547,-1.,1.80351583877342));
#18532=CARTESIAN_POINT('Ctrl Pts',(0.762546129463938,-1.,1.80938551463965));
#18533=CARTESIAN_POINT('Ctrl Pts',(0.763132003836634,-1.,1.8153211840553));
#18534=CARTESIAN_POINT('Ctrl Pts',(0.763673465462726,-1.,1.82131873145266));
#18535=CARTESIAN_POINT('Ctrl Pts',(0.764165902605995,-1.,1.82735991200065));
#18536=CARTESIAN_POINT('Ctrl Pts',(0.764602549687853,-1.,1.83342077227142));
#18537=CARTESIAN_POINT('Ctrl Pts',(0.764978057881737,-1.,1.83948181064835));
#18538=CARTESIAN_POINT('Ctrl Pts',(0.765291664862029,-1.,1.84553698875924));
#18539=CARTESIAN_POINT('Ctrl Pts',(0.765545710619062,-1.,1.85158945130063));
#18540=CARTESIAN_POINT('Ctrl Pts',(0.765744212909318,-1.,1.85764741390394));
#18541=CARTESIAN_POINT('Ctrl Pts',(0.765891519092547,-1.,1.86372027063312));
#18542=CARTESIAN_POINT('Ctrl Pts',(0.765990708546091,-1.,1.86981398314341));
#18543=CARTESIAN_POINT('Ctrl Pts',(0.766042837036744,-1.,1.87592888967883));
#18544=CARTESIAN_POINT('Ctrl Pts',(0.766047794851864,-1.,1.88206215302561));
#18545=CARTESIAN_POINT('Ctrl Pts',(0.766004837062091,-1.,1.88820926433409));
#18546=CARTESIAN_POINT('Ctrl Pts',(0.765913193856978,-1.,1.89436577771388));
#18547=CARTESIAN_POINT('Ctrl Pts',(0.765772772593386,-1.,1.90052930393596));
#18548=CARTESIAN_POINT('Ctrl Pts',(0.765584196937919,-1.,1.90669961402356));
#18549=CARTESIAN_POINT('Ctrl Pts',(0.765348465884722,-1.,1.91287765805169));
#18550=CARTESIAN_POINT('Ctrl Pts',(0.765066729667088,-1.,1.91906491634196));
#18551=CARTESIAN_POINT('Ctrl Pts',(0.764740025488211,-1.,1.92526263537048));
#18552=CARTESIAN_POINT('Ctrl Pts',(0.76436901067394,-1.,1.93147105496382));
#18553=CARTESIAN_POINT('Ctrl Pts',(0.763954049121458,-1.,1.93768964875886));
#18554=CARTESIAN_POINT('Ctrl Pts',(0.763495333538629,-1.,1.9439174661764));
#18555=CARTESIAN_POINT('Ctrl Pts',(0.762992990878769,-1.,1.95015342590024));
#18556=CARTESIAN_POINT('Ctrl Pts',(0.762447203806178,-1.,1.95639665309869));
#18557=CARTESIAN_POINT('Ctrl Pts',(0.761858300014423,-1.,1.96264672744186));
#18558=CARTESIAN_POINT('Ctrl Pts',(0.76122669048382,-1.,1.96890351582499));
#18559=CARTESIAN_POINT('Ctrl Pts',(0.760552825409757,-1.,1.97516705321494));
#18560=CARTESIAN_POINT('Ctrl Pts',(0.75983714745219,-1.,1.98143741418172));
#18561=CARTESIAN_POINT('Ctrl Pts',(0.759080037802488,-1.,1.98771456680874));
#18562=CARTESIAN_POINT('Ctrl Pts',(0.758281796766761,-1.,1.99399831098817));
#18563=CARTESIAN_POINT('Ctrl Pts',(0.757442676862724,-1.,2.00028834739178));
#18564=CARTESIAN_POINT('Ctrl Pts',(0.75656290464667,-1.,2.0065843158773));
#18565=CARTESIAN_POINT('Ctrl Pts',(0.755642704957865,-1.,2.01288584328084));
#18566=CARTESIAN_POINT('Ctrl Pts',(0.754682330722816,-1.,2.01919259405809));
#18567=CARTESIAN_POINT('Ctrl Pts',(0.753682061112768,-1.,2.02550428623313));
#18568=CARTESIAN_POINT('Ctrl Pts',(0.75264218048721,-1.,2.03182068456221));
#18569=CARTESIAN_POINT('Ctrl Pts',(0.751562963361115,-1.,2.03814160092099));
#18570=CARTESIAN_POINT('Ctrl Pts',(0.750444657875575,-1.,2.04446689147979));
#18571=CARTESIAN_POINT('Ctrl Pts',(0.749287468665046,-1.,2.05079645592154));
#18572=CARTESIAN_POINT('Ctrl Pts',(0.748091554183802,-1.,2.05713023031007));
#18573=CARTESIAN_POINT('Ctrl Pts',(0.747103932787919,-1.,2.06220058927826));
#18574=CARTESIAN_POINT('Ctrl Pts',(0.7463458715442,-1.,2.06600523016815));
#18575=CARTESIAN_POINT('Ctrl Pts',(0.745832791378367,-1.,2.06854248895728));
#18576=CARTESIAN_POINT('Ctrl Pts',(0.7455743247944,-1.,2.0698113262342));
#18577=CARTESIAN_POINT('',(0.61342227326009,-1.,2.11275013067528));
#18578=CARTESIAN_POINT('',(0.7455743247944,-1.,2.0698113262342));
#18579=CARTESIAN_POINT('',(0.383122945602004,-1.,1.7075470150345));
#18580=CARTESIAN_POINT('Ctrl Pts',(0.61342227326009,-1.,2.11275013067528));
#18581=CARTESIAN_POINT('Ctrl Pts',(0.6124673655618,-1.,2.11187554259986));
#18582=CARTESIAN_POINT('Ctrl Pts',(0.610560911689898,-1.,2.11012443807238));
#18583=CARTESIAN_POINT('Ctrl Pts',(0.607711315454876,-1.,2.1074919961518));
#18584=CARTESIAN_POINT('Ctrl Pts',(0.60393203073603,-1.,2.10397049886949));
#18585=CARTESIAN_POINT('Ctrl Pts',(0.599241616420533,-1.,2.0995493086477));
#18586=CARTESIAN_POINT('Ctrl Pts',(0.594585006052162,-1.,2.0951087622027));
#18587=CARTESIAN_POINT('Ctrl Pts',(0.589962365403406,-1.,2.09064881812129));
#18588=CARTESIAN_POINT('Ctrl Pts',(0.585373918991617,-1.,2.08616943727951));
#18589=CARTESIAN_POINT('Ctrl Pts',(0.580819952108063,-1.,2.08167059018418));
#18590=CARTESIAN_POINT('Ctrl Pts',(0.576300797416844,-1.,2.07715226767559));
#18591=CARTESIAN_POINT('Ctrl Pts',(0.571816823242602,-1.,2.07261449292824));
#18592=CARTESIAN_POINT('Ctrl Pts',(0.567368421181087,-1.,2.06805732997334));
#18593=CARTESIAN_POINT('Ctrl Pts',(0.562955993082261,-1.,2.06348090160589));
#18594=CARTESIAN_POINT('Ctrl Pts',(0.558579940185151,-1.,2.05888537756462));
#18595=CARTESIAN_POINT('Ctrl Pts',(0.554240657463906,-1.,2.05427091604413));
#18596=CARTESIAN_POINT('Ctrl Pts',(0.549938525150295,-1.,2.04963761077958));
#18597=CARTESIAN_POINT('Ctrl Pts',(0.54567390381743,-1.,2.04498544714588));
#18598=CARTESIAN_POINT('Ctrl Pts',(0.541447120615659,-1.,2.04031422690527));
#18599=CARTESIAN_POINT('Ctrl Pts',(0.537258489833262,-1.,2.03562362954037));
#18600=CARTESIAN_POINT('Ctrl Pts',(0.533108355132976,-1.,2.03091336214426));
#18601=CARTESIAN_POINT('Ctrl Pts',(0.528997127241914,-1.,2.0261832908329));
#18602=CARTESIAN_POINT('Ctrl Pts',(0.524925318333476,-1.,2.02143356304698));
#18603=CARTESIAN_POINT('Ctrl Pts',(0.52089359039937,-1.,2.01666477917286));
#18604=CARTESIAN_POINT('Ctrl Pts',(0.516902681728687,-1.,2.01187773939242));
#18605=CARTESIAN_POINT('Ctrl Pts',(0.512953306961792,-1.,2.00707309946949));
#18606=CARTESIAN_POINT('Ctrl Pts',(0.509046069886157,-1.,2.00225107134734));
#18607=CARTESIAN_POINT('Ctrl Pts',(0.505181361323026,-1.,1.99741107463572));
#18608=CARTESIAN_POINT('Ctrl Pts',(0.501359287727146,-1.,1.99255149126155));
#18609=CARTESIAN_POINT('Ctrl Pts',(0.497579909545574,-1.,1.98767044752932));
#18610=CARTESIAN_POINT('Ctrl Pts',(0.493843476541494,-1.,1.98276658761821));
#18611=CARTESIAN_POINT('Ctrl Pts',(0.490150627860952,-1.,1.97783973019229));
#18612=CARTESIAN_POINT('Ctrl Pts',(0.486502692907658,-1.,1.97289186263272));
#18613=CARTESIAN_POINT('Ctrl Pts',(0.48290166212069,-1.,1.96792703422362));
#18614=CARTESIAN_POINT('Ctrl Pts',(0.479349583074855,-1.,1.96294933055943));
#18615=CARTESIAN_POINT('Ctrl Pts',(0.475848034683176,-1.,1.95796111148177));
#18616=CARTESIAN_POINT('Ctrl Pts',(0.472397672264072,-1.,1.95296148278133));
#18617=CARTESIAN_POINT('Ctrl Pts',(0.468997482913135,-1.,1.94794381136514));
#18618=CARTESIAN_POINT('Ctrl Pts',(0.46564546202603,-1.,1.9428979419619));
#18619=CARTESIAN_POINT('Ctrl Pts',(0.462340031009056,-1.,1.93781486640821));
#18620=CARTESIAN_POINT('Ctrl Pts',(0.459081234547926,-1.,1.93269066517934));
#18621=CARTESIAN_POINT('Ctrl Pts',(0.45587200517437,-1.,1.92753067150476));
#18622=CARTESIAN_POINT('Ctrl Pts',(0.452719478359432,-1.,1.92235380648502));
#18623=CARTESIAN_POINT('Ctrl Pts',(0.449632260106662,-1.,1.91718342555755));
#18624=CARTESIAN_POINT('Ctrl Pts',(0.446617343485711,-1.,1.9120369998112));
#18625=CARTESIAN_POINT('Ctrl Pts',(0.44367755684915,-1.,1.90691756144898));
#18626=CARTESIAN_POINT('Ctrl Pts',(0.440807833704038,-1.,1.90180124389086));
#18627=CARTESIAN_POINT('Ctrl Pts',(0.437995003948244,-1.,1.89663648956466));
#18628=CARTESIAN_POINT('Ctrl Pts',(0.435225660963383,-1.,1.89136993975504));
#18629=CARTESIAN_POINT('Ctrl Pts',(0.432493038548748,-1.,1.88596913666793));
#18630=CARTESIAN_POINT('Ctrl Pts',(0.429803062482344,-1.,1.88044229001832));
#18631=CARTESIAN_POINT('Ctrl Pts',(0.427183828519102,-1.,1.87486989291484));
#18632=CARTESIAN_POINT('Ctrl Pts',(0.424678177291358,-1.,1.86937803944323));
#18633=CARTESIAN_POINT('Ctrl Pts',(0.422327307418275,-1.,1.86408083334028));
#18634=CARTESIAN_POINT('Ctrl Pts',(0.420157287975619,-1.,1.85903281096686));
#18635=CARTESIAN_POINT('Ctrl Pts',(0.418164129143534,-1.,1.85417632856234));
#18636=CARTESIAN_POINT('Ctrl Pts',(0.416300022038864,-1.,1.84929312929882));
#18637=CARTESIAN_POINT('Ctrl Pts',(0.41448743825434,-1.,1.8440575707371));
#18638=CARTESIAN_POINT('Ctrl Pts',(0.412633125322161,-1.,1.83808953475839));
#18639=CARTESIAN_POINT('Ctrl Pts',(0.410641256301674,-1.,1.83100408895216));
#18640=CARTESIAN_POINT('Ctrl Pts',(0.408428948108533,-1.,1.8224702267854));
#18641=CARTESIAN_POINT('Ctrl Pts',(0.405933518411838,-1.,1.81223801813988));
#18642=CARTESIAN_POINT('Ctrl Pts',(0.403107976170441,-1.,1.80012077176221));
#18643=CARTESIAN_POINT('Ctrl Pts',(0.39991940378308,-1.,1.78598826347533));
#18644=CARTESIAN_POINT('Ctrl Pts',(0.39634619612042,-1.,1.7697556004756));
#18645=CARTESIAN_POINT('Ctrl Pts',(0.392375812294307,-1.,1.75137405313962));
#18646=CARTESIAN_POINT('Ctrl Pts',(0.388877023509191,-1.,1.7349317097561));
#18647=CARTESIAN_POINT('Ctrl Pts',(0.38607079032701,-1.,1.72162022246158));
#18648=CARTESIAN_POINT('Ctrl Pts',(0.384119047315541,-1.,1.71231062891958));
#18649=CARTESIAN_POINT('Ctrl Pts',(0.383122945602004,-1.,1.7075470150345));
#18650=CARTESIAN_POINT('',(0.163289472382896,-1.,1.74236521665491));
#18651=CARTESIAN_POINT('Origin',(0.,-1.,0.));
#18652=CARTESIAN_POINT('',(0.0694764450219578,-1.,2.19890268624765));
#18653=CARTESIAN_POINT('Ctrl Pts',(0.163289472382896,-1.,1.74236521665491));
#18654=CARTESIAN_POINT('Ctrl Pts',(0.163814161002002,-1.,1.7472034950333));
#18655=CARTESIAN_POINT('Ctrl Pts',(0.164834765707158,-1.,1.75666056638427));
#18656=CARTESIAN_POINT('Ctrl Pts',(0.1662793551464,-1.,1.77018771684844));
#18657=CARTESIAN_POINT('Ctrl Pts',(0.168032772805197,-1.,1.7869064998507));
#18658=CARTESIAN_POINT('Ctrl Pts',(0.169936923904608,-1.,1.80561530629706));
#18659=CARTESIAN_POINT('Ctrl Pts',(0.171554770204119,-1.,1.82215766811545));
#18660=CARTESIAN_POINT('Ctrl Pts',(0.1728894428919,-1.,1.83658380527692));
#18661=CARTESIAN_POINT('Ctrl Pts',(0.173946627587731,-1.,1.8489811319852));
#18662=CARTESIAN_POINT('Ctrl Pts',(0.17473525927603,-1.,1.85948367088837));
#18663=CARTESIAN_POINT('Ctrl Pts',(0.175268337590757,-1.,1.86828349694799));
#18664=CARTESIAN_POINT('Ctrl Pts',(0.175563480746485,-1.,1.87563767773588));
#18665=CARTESIAN_POINT('Ctrl Pts',(0.175644148889698,-1.,1.88188663145367));
#18666=CARTESIAN_POINT('Ctrl Pts',(0.175538155840648,-1.,1.88742606273259));
#18667=CARTESIAN_POINT('Ctrl Pts',(0.175274276190844,-1.,1.892646301985));
#18668=CARTESIAN_POINT('Ctrl Pts',(0.174879405091263,-1.,1.89788101117132));
#18669=CARTESIAN_POINT('Ctrl Pts',(0.174375518661085,-1.,1.90335253862834));
#18670=CARTESIAN_POINT('Ctrl Pts',(0.173776635257816,-1.,1.90911693975267));
#18671=CARTESIAN_POINT('Ctrl Pts',(0.173090695383496,-1.,1.91511429159527));
#18672=CARTESIAN_POINT('Ctrl Pts',(0.172321621259513,-1.,1.9212233439798));
#18673=CARTESIAN_POINT('Ctrl Pts',(0.171471191532988,-1.,1.92731093582036));
#18674=CARTESIAN_POINT('Ctrl Pts',(0.170541253116201,-1.,1.93329183155539));
#18675=CARTESIAN_POINT('Ctrl Pts',(0.16953490481749,-1.,1.93915639211581));
#18676=CARTESIAN_POINT('Ctrl Pts',(0.168455741607556,-1.,1.94493757756931));
#18677=CARTESIAN_POINT('Ctrl Pts',(0.167307501784475,-1.,1.95069027794294));
#18678=CARTESIAN_POINT('Ctrl Pts',(0.166093592002812,-1.,1.9564675971873));
#18679=CARTESIAN_POINT('Ctrl Pts',(0.164816568920269,-1.,1.96229379940136));
#18680=CARTESIAN_POINT('Ctrl Pts',(0.163478185457734,-1.,1.96816512677967));
#18681=CARTESIAN_POINT('Ctrl Pts',(0.162079693556288,-1.,1.97406280235188));
#18682=CARTESIAN_POINT('Ctrl Pts',(0.160622060784611,-1.,1.97996195437559));
#18683=CARTESIAN_POINT('Ctrl Pts',(0.159106226437299,-1.,1.98584238283292));
#18684=CARTESIAN_POINT('Ctrl Pts',(0.157533331459227,-1.,1.99169810931908));
#18685=CARTESIAN_POINT('Ctrl Pts',(0.155904629548783,-1.,1.99753284771497));
#18686=CARTESIAN_POINT('Ctrl Pts',(0.154221403049722,-1.,2.00335565310543));
#18687=CARTESIAN_POINT('Ctrl Pts',(0.152484883621449,-1.,2.00917680318424));
#18688=CARTESIAN_POINT('Ctrl Pts',(0.150696157673078,-1.,2.01500291940238));
#18689=CARTESIAN_POINT('Ctrl Pts',(0.148856124775337,-1.,2.02083464969894));
#18690=CARTESIAN_POINT('Ctrl Pts',(0.146965557332583,-1.,2.02666926182017));
#18691=CARTESIAN_POINT('Ctrl Pts',(0.145025140186057,-1.,2.03250223739942));
#18692=CARTESIAN_POINT('Ctrl Pts',(0.143035515058208,-1.,2.03832911025912));
#18693=CARTESIAN_POINT('Ctrl Pts',(0.140997332152546,-1.,2.04414757947916));
#18694=CARTESIAN_POINT('Ctrl Pts',(0.138911255368966,-1.,2.04995762001328));
#18695=CARTESIAN_POINT('Ctrl Pts',(0.136777941218043,-1.,2.05576044414264));
#18696=CARTESIAN_POINT('Ctrl Pts',(0.134598026192106,-1.,2.06155781517842));
#18697=CARTESIAN_POINT('Ctrl Pts',(0.13237211154771,-1.,2.06735123910326));
#18698=CARTESIAN_POINT('Ctrl Pts',(0.130100748328403,-1.,2.07314114713063));
#18699=CARTESIAN_POINT('Ctrl Pts',(0.12778444527612,-1.,2.07892715110987));
#18700=CARTESIAN_POINT('Ctrl Pts',(0.125423679412061,-1.,2.08470840653643));
#18701=CARTESIAN_POINT('Ctrl Pts',(0.123018905621083,-1.,2.09048392424825));
#18702=CARTESIAN_POINT('Ctrl Pts',(0.120570567965122,-1.,2.0962529286773));
#18703=CARTESIAN_POINT('Ctrl Pts',(0.118079107988355,-1.,2.102015121329));
#18704=CARTESIAN_POINT('Ctrl Pts',(0.115544957687926,-1.,2.10777050261309));
#18705=CARTESIAN_POINT('Ctrl Pts',(0.112968534419737,-1.,2.11351924490306));
#18706=CARTESIAN_POINT('Ctrl Pts',(0.110350236135025,-1.,2.11926155590865));
#18707=CARTESIAN_POINT('Ctrl Pts',(0.10769043523109,-1.,2.12499752307));
#18708=CARTESIAN_POINT('Ctrl Pts',(0.104989479152739,-1.,2.13072704887293));
#18709=CARTESIAN_POINT('Ctrl Pts',(0.1022477005561,-1.,2.13644992667165));
#18710=CARTESIAN_POINT('Ctrl Pts',(0.0994654261990913,-1.,2.14216588396025));
#18711=CARTESIAN_POINT('Ctrl Pts',(0.0966429852305456,-1.,2.14787463531795));
#18712=CARTESIAN_POINT('Ctrl Pts',(0.0937807218867641,-1.,2.1535759397817));
#18713=CARTESIAN_POINT('Ctrl Pts',(0.0908789888107263,-1.,2.15926961544516));
#18714=CARTESIAN_POINT('Ctrl Pts',(0.087938129138692,-1.,2.16495552645014));
#18715=CARTESIAN_POINT('Ctrl Pts',(0.084958462083537,-1.,2.17063357870952));
#18716=CARTESIAN_POINT('Ctrl Pts',(0.0819402680872763,-1.,2.176303712113));
#18717=CARTESIAN_POINT('Ctrl Pts',(0.078883772768524,-1.,2.18196589448887));
#18718=CARTESIAN_POINT('Ctrl Pts',(0.0757891465836145,-1.,2.1876201139953));
#18719=CARTESIAN_POINT('Ctrl Pts',(0.0732830357306722,-1.,2.19213712013662));
#18720=CARTESIAN_POINT('Ctrl Pts',(0.0713863779526151,-1.,2.19552129484002));
#18721=CARTESIAN_POINT('Ctrl Pts',(0.0701143536325487,-1.,2.19777582085423));
#18722=CARTESIAN_POINT('Ctrl Pts',(0.0694764450219578,-1.,2.19890268624765));
#18723=CARTESIAN_POINT('',(-0.0694764450219586,-1.,2.19890268624765));
#18724=CARTESIAN_POINT('',(0.0694764450219578,-1.,2.19890268624765));
#18725=CARTESIAN_POINT('',(-0.163289472382896,-1.,1.74236521665491));
#18726=CARTESIAN_POINT('Ctrl Pts',(-0.0694764450219586,-1.,2.19890268624765));
#18727=CARTESIAN_POINT('Ctrl Pts',(-0.0701143536324929,-1.,2.19777582085261));
#18728=CARTESIAN_POINT('Ctrl Pts',(-0.071386377952463,-1.,2.19552129483562));
#18729=CARTESIAN_POINT('Ctrl Pts',(-0.0732830357304279,-1.,2.19213712012956));
#18730=CARTESIAN_POINT('Ctrl Pts',(-0.0757891465833414,-1.,2.1876201139874));
#18731=CARTESIAN_POINT('Ctrl Pts',(-0.078883772768323,-1.,2.18196589448304));
#18732=CARTESIAN_POINT('Ctrl Pts',(-0.0819402680871942,-1.,2.1763037121106));
#18733=CARTESIAN_POINT('Ctrl Pts',(-0.0849584620835646,-1.,2.17063357871031));
#18734=CARTESIAN_POINT('Ctrl Pts',(-0.0879381291387825,-1.,2.16495552645275));
#18735=CARTESIAN_POINT('Ctrl Pts',(-0.0908789888108269,-1.,2.15926961544808));
#18736=CARTESIAN_POINT('Ctrl Pts',(-0.0937807218868348,-1.,2.15357593978377));
#18737=CARTESIAN_POINT('Ctrl Pts',(-0.0966429852305691,-1.,2.14787463531864));
#18738=CARTESIAN_POINT('Ctrl Pts',(-0.0994654261990745,-1.,2.14216588395974));
#18739=CARTESIAN_POINT('Ctrl Pts',(-0.102247700556064,-1.,2.13644992667052));
#18740=CARTESIAN_POINT('Ctrl Pts',(-0.104989479152703,-1.,2.1307270488718));
#18741=CARTESIAN_POINT('Ctrl Pts',(-0.107690435231068,-1.,2.12499752306927));
#18742=CARTESIAN_POINT('Ctrl Pts',(-0.11035023613502,-1.,2.11926155590849));
#18743=CARTESIAN_POINT('Ctrl Pts',(-0.112968534419746,-1.,2.11351924490335));
#18744=CARTESIAN_POINT('Ctrl Pts',(-0.115544957687941,-1.,2.10777050261359));
#18745=CARTESIAN_POINT('Ctrl Pts',(-0.118079107988368,-1.,2.10201512132945));
#18746=CARTESIAN_POINT('Ctrl Pts',(-0.120570567965129,-1.,2.09625292867756));
#18747=CARTESIAN_POINT('Ctrl Pts',(-0.123018905621083,-1.,2.09048392424826));
#18748=CARTESIAN_POINT('Ctrl Pts',(-0.125423679412058,-1.,2.08470840653628));
#18749=CARTESIAN_POINT('Ctrl Pts',(-0.127784445276116,-1.,2.07892715110967));
#18750=CARTESIAN_POINT('Ctrl Pts',(-0.130100748328401,-1.,2.07314114713047));
#18751=CARTESIAN_POINT('Ctrl Pts',(-0.13237211154771,-1.,2.06735123910319));
#18752=CARTESIAN_POINT('Ctrl Pts',(-0.134598026192107,-1.,2.06155781517844));
#18753=CARTESIAN_POINT('Ctrl Pts',(-0.136777941218044,-1.,2.0557604441427));
#18754=CARTESIAN_POINT('Ctrl Pts',(-0.138911255368966,-1.,2.04995762001333));
#18755=CARTESIAN_POINT('Ctrl Pts',(-0.140997332152546,-1.,2.04414757947919));
#18756=CARTESIAN_POINT('Ctrl Pts',(-0.143035515058208,-1.,2.03832911025913));
#18757=CARTESIAN_POINT('Ctrl Pts',(-0.145025140186058,-1.,2.03250223739941));
#18758=CARTESIAN_POINT('Ctrl Pts',(-0.146965557332586,-1.,2.02666926182017));
#18759=CARTESIAN_POINT('Ctrl Pts',(-0.148856124775343,-1.,2.02083464969897));
#18760=CARTESIAN_POINT('Ctrl Pts',(-0.150696157673084,-1.,2.01500291940243));
#18761=CARTESIAN_POINT('Ctrl Pts',(-0.152484883621452,-1.,2.00917680318426));
#18762=CARTESIAN_POINT('Ctrl Pts',(-0.154221403049719,-1.,2.00335565310539));
#18763=CARTESIAN_POINT('Ctrl Pts',(-0.155904629548775,-1.,1.99753284771487));
#18764=CARTESIAN_POINT('Ctrl Pts',(-0.157533331459215,-1.,1.99169810931893));
#18765=CARTESIAN_POINT('Ctrl Pts',(-0.159106226437289,-1.,1.98584238283279));
#18766=CARTESIAN_POINT('Ctrl Pts',(-0.16062206078461,-1.,1.97996195437557));
#18767=CARTESIAN_POINT('Ctrl Pts',(-0.162079693556302,-1.,1.97406280235204));
#18768=CARTESIAN_POINT('Ctrl Pts',(-0.16347818545776,-1.,1.96816512678));
#18769=CARTESIAN_POINT('Ctrl Pts',(-0.1648165689203,-1.,1.96229379940174));
#18770=CARTESIAN_POINT('Ctrl Pts',(-0.166093592002833,-1.,1.95646759718755));
#18771=CARTESIAN_POINT('Ctrl Pts',(-0.167307501784469,-1.,1.95069027794286));
#18772=CARTESIAN_POINT('Ctrl Pts',(-0.168455741607516,-1.,1.94493757756879));
#18773=CARTESIAN_POINT('Ctrl Pts',(-0.169534904817425,-1.,1.93915639211497));
#18774=CARTESIAN_POINT('Ctrl Pts',(-0.170541253116136,-1.,1.93329183155455));
#18775=CARTESIAN_POINT('Ctrl Pts',(-0.17147119153296,-1.,1.92731093582));
#18776=CARTESIAN_POINT('Ctrl Pts',(-0.172321621259557,-1.,1.92122334398034));
#18777=CARTESIAN_POINT('Ctrl Pts',(-0.173090695383619,-1.,1.91511429159681));
#18778=CARTESIAN_POINT('Ctrl Pts',(-0.173776635257984,-1.,1.90911693975475));
#18779=CARTESIAN_POINT('Ctrl Pts',(-0.174375518661222,-1.,1.90335253863003));
#18780=CARTESIAN_POINT('Ctrl Pts',(-0.174879405091277,-1.,1.89788101117148));
#18781=CARTESIAN_POINT('Ctrl Pts',(-0.175274276190664,-1.,1.89264630198279));
#18782=CARTESIAN_POINT('Ctrl Pts',(-0.175538155840286,-1.,1.88742606272818));
#18783=CARTESIAN_POINT('Ctrl Pts',(-0.175644148889271,-1.,1.88188663144846));
#18784=CARTESIAN_POINT('Ctrl Pts',(-0.175563480746206,-1.,1.87563767773249));
#18785=CARTESIAN_POINT('Ctrl Pts',(-0.175268337590901,-1.,1.86828349694972));
#18786=CARTESIAN_POINT('Ctrl Pts',(-0.174735259276856,-1.,1.85948367089838));
#18787=CARTESIAN_POINT('Ctrl Pts',(-0.173946627589401,-1.,1.84898113200543));
#18788=CARTESIAN_POINT('Ctrl Pts',(-0.17288944289442,-1.,1.83658380530747));
#18789=CARTESIAN_POINT('Ctrl Pts',(-0.171554770207306,-1.,1.82215766815414));
#18790=CARTESIAN_POINT('Ctrl Pts',(-0.169936923908078,-1.,1.80561530633924));
#18791=CARTESIAN_POINT('Ctrl Pts',(-0.16803277280837,-1.,1.78690649988931));
#18792=CARTESIAN_POINT('Ctrl Pts',(-0.166279355148738,-1.,1.77018771687692));
#18793=CARTESIAN_POINT('Ctrl Pts',(-0.164834765708484,-1.,1.75666056640041));
#18794=CARTESIAN_POINT('Ctrl Pts',(-0.163814161002474,-1.,1.74720349503904));
#18795=CARTESIAN_POINT('Ctrl Pts',(-0.163289472382896,-1.,1.74236521665491));
#18796=CARTESIAN_POINT('',(-0.383122945602004,-1.,1.7075470150345));
#18797=CARTESIAN_POINT('Origin',(0.,-1.,0.));
#18798=CARTESIAN_POINT('',(-0.61342227326009,-1.,2.11275013067528));
#18799=CARTESIAN_POINT('Ctrl Pts',(-0.383122945602004,-1.,1.7075470150345));
#18800=CARTESIAN_POINT('Ctrl Pts',(-0.384119047314215,-1.,1.71231062891398));
#18801=CARTESIAN_POINT('Ctrl Pts',(-0.386070790323281,-1.,1.72162022244582));
#18802=CARTESIAN_POINT('Ctrl Pts',(-0.388877023502615,-1.,1.73493170972829));
#18803=CARTESIAN_POINT('Ctrl Pts',(-0.392375812285395,-1.,1.75137405310193));
#18804=CARTESIAN_POINT('Ctrl Pts',(-0.396346196110688,-1.,1.76975560043442));
#18805=CARTESIAN_POINT('Ctrl Pts',(-0.399919403774155,-1.,1.78598826343754));
#18806=CARTESIAN_POINT('Ctrl Pts',(-0.403107976163396,-1.,1.80012077173238));
#18807=CARTESIAN_POINT('Ctrl Pts',(-0.405933518407175,-1.,1.81223801812013));
#18808=CARTESIAN_POINT('Ctrl Pts',(-0.408428948106227,-1.,1.82247022677562));
#18809=CARTESIAN_POINT('Ctrl Pts',(-0.410641256301276,-1.,1.83100408895047));
#18810=CARTESIAN_POINT('Ctrl Pts',(-0.412633125322945,-1.,1.8380895347617));
#18811=CARTESIAN_POINT('Ctrl Pts',(-0.414487438255542,-1.,1.84405757074218));
#18812=CARTESIAN_POINT('Ctrl Pts',(-0.416300022039885,-1.,1.84929312930314));
#18813=CARTESIAN_POINT('Ctrl Pts',(-0.418164129144045,-1.,1.8541763285645));
#18814=CARTESIAN_POINT('Ctrl Pts',(-0.420157287975583,-1.,1.8590328109667));
#18815=CARTESIAN_POINT('Ctrl Pts',(-0.422327307417885,-1.,1.86408083333863));
#18816=CARTESIAN_POINT('Ctrl Pts',(-0.424678177290876,-1.,1.8693780394412));
#18817=CARTESIAN_POINT('Ctrl Pts',(-0.427183828518743,-1.,1.87486989291333));
#18818=CARTESIAN_POINT('Ctrl Pts',(-0.429803062482217,-1.,1.88044229001778));
#18819=CARTESIAN_POINT('Ctrl Pts',(-0.432493038548833,-1.,1.88596913666828));
#18820=CARTESIAN_POINT('Ctrl Pts',(-0.43522566096358,-1.,1.89136993975585));
#18821=CARTESIAN_POINT('Ctrl Pts',(-0.437995003948443,-1.,1.89663648956549));
#18822=CARTESIAN_POINT('Ctrl Pts',(-0.440807833704161,-1.,1.90180124389137));
#18823=CARTESIAN_POINT('Ctrl Pts',(-0.44367755684917,-1.,1.90691756144906));
#18824=CARTESIAN_POINT('Ctrl Pts',(-0.446617343485651,-1.,1.91203699981095));
#18825=CARTESIAN_POINT('Ctrl Pts',(-0.449632260106572,-1.,1.91718342555717));
#18826=CARTESIAN_POINT('Ctrl Pts',(-0.452719478359356,-1.,1.9223538064847));
#18827=CARTESIAN_POINT('Ctrl Pts',(-0.455872005174335,-1.,1.92753067150461));
#18828=CARTESIAN_POINT('Ctrl Pts',(-0.459081234547931,-1.,1.93269066517936));
#18829=CARTESIAN_POINT('Ctrl Pts',(-0.462340031009087,-1.,1.93781486640834));
#18830=CARTESIAN_POINT('Ctrl Pts',(-0.465645462026065,-1.,1.94289794196205));
#18831=CARTESIAN_POINT('Ctrl Pts',(-0.468997482913158,-1.,1.94794381136524));
#18832=CARTESIAN_POINT('Ctrl Pts',(-0.47239767226408,-1.,1.95296148278136));
#18833=CARTESIAN_POINT('Ctrl Pts',(-0.475848034683172,-1.,1.95796111148175));
#18834=CARTESIAN_POINT('Ctrl Pts',(-0.479349583074846,-1.,1.96294933055938));
#18835=CARTESIAN_POINT('Ctrl Pts',(-0.482901662120687,-1.,1.96792703422358));
#18836=CARTESIAN_POINT('Ctrl Pts',(-0.486502692907661,-1.,1.97289186263272));
#18837=CARTESIAN_POINT('Ctrl Pts',(-0.490150627860955,-1.,1.97783973019229));
#18838=CARTESIAN_POINT('Ctrl Pts',(-0.493843476541492,-1.,1.9827665876182));
#18839=CARTESIAN_POINT('Ctrl Pts',(-0.497579909545564,-1.,1.98767044752929));
#18840=CARTESIAN_POINT('Ctrl Pts',(-0.501359287727129,-1.,1.9925514912615));
#18841=CARTESIAN_POINT('Ctrl Pts',(-0.505181361323011,-1.,1.99741107463567));
#18842=CARTESIAN_POINT('Ctrl Pts',(-0.509046069886152,-1.,2.00225107134733));
#18843=CARTESIAN_POINT('Ctrl Pts',(-0.512953306961814,-1.,2.00707309946955));
#18844=CARTESIAN_POINT('Ctrl Pts',(-0.516902681728733,-1.,2.01187773939257));
#18845=CARTESIAN_POINT('Ctrl Pts',(-0.520893590399428,-1.,2.01666477917305));
#18846=CARTESIAN_POINT('Ctrl Pts',(-0.524925318333518,-1.,2.02143356304712));
#18847=CARTESIAN_POINT('Ctrl Pts',(-0.528997127241911,-1.,2.02618329083289));
#18848=CARTESIAN_POINT('Ctrl Pts',(-0.533108355132905,-1.,2.03091336214401));
#18849=CARTESIAN_POINT('Ctrl Pts',(-0.537258489833134,-1.,2.03562362953993));
#18850=CARTESIAN_POINT('Ctrl Pts',(-0.54144712061552,-1.,2.0403142269048));
#18851=CARTESIAN_POINT('Ctrl Pts',(-0.545673903817348,-1.,2.0449854471456));
#18852=CARTESIAN_POINT('Ctrl Pts',(-0.549938525150342,-1.,2.04963761077974));
#18853=CARTESIAN_POINT('Ctrl Pts',(-0.55424065746411,-1.,2.05427091604482));
#18854=CARTESIAN_POINT('Ctrl Pts',(-0.558579940185467,-1.,2.05888537756571));
#18855=CARTESIAN_POINT('Ctrl Pts',(-0.562955993082574,-1.,2.06348090160697));
#18856=CARTESIAN_POINT('Ctrl Pts',(-0.567368421181229,-1.,2.06805732997383));
#18857=CARTESIAN_POINT('Ctrl Pts',(-0.571816823242411,-1.,2.07261449292757));
#18858=CARTESIAN_POINT('Ctrl Pts',(-0.576300797416275,-1.,2.07715226767361));
#18859=CARTESIAN_POINT('Ctrl Pts',(-0.580819952107257,-1.,2.08167059018138));
#18860=CARTESIAN_POINT('Ctrl Pts',(-0.585373918990895,-1.,2.086169437277));
#18861=CARTESIAN_POINT('Ctrl Pts',(-0.589962365403189,-1.,2.09064881812053));
#18862=CARTESIAN_POINT('Ctrl Pts',(-0.594585006052824,-1.,2.09510876220501));
#18863=CARTESIAN_POINT('Ctrl Pts',(-0.599241616422144,-1.,2.09954930865331));
#18864=CARTESIAN_POINT('Ctrl Pts',(-0.603932030738212,-1.,2.10397049887709));
#18865=CARTESIAN_POINT('Ctrl Pts',(-0.607711315456826,-1.,2.10749199615859));
#18866=CARTESIAN_POINT('Ctrl Pts',(-0.610560911691113,-1.,2.11012443807661));
#18867=CARTESIAN_POINT('Ctrl Pts',(-0.61246736556225,-1.,2.11187554260142));
#18868=CARTESIAN_POINT('Ctrl Pts',(-0.61342227326009,-1.,2.11275013067528));
#18869=CARTESIAN_POINT('',(-0.745574324794401,-1.,2.0698113262342));
#18870=CARTESIAN_POINT('',(-0.61342227326009,-1.,2.11275013067528));
#18871=CARTESIAN_POINT('',(-0.693717979106306,-1.,1.60662857109684));
#18872=CARTESIAN_POINT('Ctrl Pts',(-0.745574324794401,-1.,2.0698113262342));
#18873=CARTESIAN_POINT('Ctrl Pts',(-0.74583279137781,-1.,2.06854248895575));
#18874=CARTESIAN_POINT('Ctrl Pts',(-0.746345871542696,-1.,2.06600523016401));
#18875=CARTESIAN_POINT('Ctrl Pts',(-0.747103932785504,-1.,2.06220058927162));
#18876=CARTESIAN_POINT('Ctrl Pts',(-0.748091554181101,-1.,2.05713023030263));
#18877=CARTESIAN_POINT('Ctrl Pts',(-0.749287468663053,-1.,2.05079645591606));
#18878=CARTESIAN_POINT('Ctrl Pts',(-0.750444657874758,-1.,2.04446689147754));
#18879=CARTESIAN_POINT('Ctrl Pts',(-0.751562963361384,-1.,2.03814160092173));
#18880=CARTESIAN_POINT('Ctrl Pts',(-0.752642180488104,-1.,2.03182068456467));
#18881=CARTESIAN_POINT('Ctrl Pts',(-0.753682061113766,-1.,2.02550428623587));
#18882=CARTESIAN_POINT('Ctrl Pts',(-0.75468233072352,-1.,2.01919259406003));
#18883=CARTESIAN_POINT('Ctrl Pts',(-0.7556427049581,-1.,2.01288584328149));
#18884=CARTESIAN_POINT('Ctrl Pts',(-0.756562904646496,-1.,2.00658431587682));
#18885=CARTESIAN_POINT('Ctrl Pts',(-0.757442676862341,-1.,2.00028834739072));
#18886=CARTESIAN_POINT('Ctrl Pts',(-0.758281796766377,-1.,1.9939983109871));
#18887=CARTESIAN_POINT('Ctrl Pts',(-0.759080037802243,-1.,1.98771456680806));
#18888=CARTESIAN_POINT('Ctrl Pts',(-0.759837147452135,-1.,1.98143741418156));
#18889=CARTESIAN_POINT('Ctrl Pts',(-0.760552825409855,-1.,1.97516705321521));
#18890=CARTESIAN_POINT('Ctrl Pts',(-0.761226690483986,-1.,1.96890351582545));
#18891=CARTESIAN_POINT('Ctrl Pts',(-0.761858300014575,-1.,1.96264672744229));
#18892=CARTESIAN_POINT('Ctrl Pts',(-0.762447203806263,-1.,1.95639665309893));
#18893=CARTESIAN_POINT('Ctrl Pts',(-0.762992990878774,-1.,1.95015342590025));
#18894=CARTESIAN_POINT('Ctrl Pts',(-0.76349533353858,-1.,1.94391746617626));
#18895=CARTESIAN_POINT('Ctrl Pts',(-0.763954049121393,-1.,1.93768964875867));
#18896=CARTESIAN_POINT('Ctrl Pts',(-0.764369010673889,-1.,1.93147105496367));
#18897=CARTESIAN_POINT('Ctrl Pts',(-0.764740025488189,-1.,1.92526263537041));
#18898=CARTESIAN_POINT('Ctrl Pts',(-0.765066729667095,-1.,1.91906491634197));
#18899=CARTESIAN_POINT('Ctrl Pts',(-0.765348465884739,-1.,1.91287765805174));
#18900=CARTESIAN_POINT('Ctrl Pts',(-0.765584196937936,-1.,1.90669961402362));
#18901=CARTESIAN_POINT('Ctrl Pts',(-0.765772772593395,-1.,1.90052930393599));
#18902=CARTESIAN_POINT('Ctrl Pts',(-0.765913193856979,-1.,1.89436577771389));
#18903=CARTESIAN_POINT('Ctrl Pts',(-0.76600483706209,-1.,1.88820926433409));
#18904=CARTESIAN_POINT('Ctrl Pts',(-0.766047794851869,-1.,1.88206215302561));
#18905=CARTESIAN_POINT('Ctrl Pts',(-0.766042837036759,-1.,1.87592888967886));
#18906=CARTESIAN_POINT('Ctrl Pts',(-0.765990708546111,-1.,1.86981398314345));
#18907=CARTESIAN_POINT('Ctrl Pts',(-0.765891519092557,-1.,1.86372027063314));
#18908=CARTESIAN_POINT('Ctrl Pts',(-0.765744212909305,-1.,1.85764741390391));
#18909=CARTESIAN_POINT('Ctrl Pts',(-0.765545710619023,-1.,1.85158945130054));
#18910=CARTESIAN_POINT('Ctrl Pts',(-0.765291664861971,-1.,1.8455369887591));
#18911=CARTESIAN_POINT('Ctrl Pts',(-0.764978057881687,-1.,1.83948181064823));
#18912=CARTESIAN_POINT('Ctrl Pts',(-0.764602549687845,-1.,1.8334207722714));
#18913=CARTESIAN_POINT('Ctrl Pts',(-0.764165902606055,-1.,1.8273599120008));
#18914=CARTESIAN_POINT('Ctrl Pts',(-0.763673465462854,-1.,1.82131873145297));
#18915=CARTESIAN_POINT('Ctrl Pts',(-0.763132003836783,-1.,1.81532118405566));
#18916=CARTESIAN_POINT('Ctrl Pts',(-0.762546129464036,-1.,1.80938551463989));
#18917=CARTESIAN_POINT('Ctrl Pts',(-0.761915336443516,-1.,1.80351583877334));
#18918=CARTESIAN_POINT('Ctrl Pts',(-0.761229695230359,-1.,1.79768986997735));
#18919=CARTESIAN_POINT('Ctrl Pts',(-0.760469555880425,-1.,1.79185815610802));
#18920=CARTESIAN_POINT('Ctrl Pts',(-0.759614401109868,-1.,1.78596964884526));
#18921=CARTESIAN_POINT('Ctrl Pts',(-0.75865062667738,-1.,1.77999411220912));
#18922=CARTESIAN_POINT('Ctrl Pts',(-0.757578264077238,-1.,1.77394167108342));
#18923=CARTESIAN_POINT('Ctrl Pts',(-0.756421896028403,-1.,1.76789396003141));
#18924=CARTESIAN_POINT('Ctrl Pts',(-0.755220979975262,-1.,1.7619781724032));
#18925=CARTESIAN_POINT('Ctrl Pts',(-0.75400925402848,-1.,1.75631083600175));
#18926=CARTESIAN_POINT('Ctrl Pts',(-0.752797683531377,-1.,1.75095139468809));
#18927=CARTESIAN_POINT('Ctrl Pts',(-0.751555614163629,-1.,1.74585086852298));
#18928=CARTESIAN_POINT('Ctrl Pts',(-0.75019343597954,-1.,1.74080458266705));
#18929=CARTESIAN_POINT('Ctrl Pts',(-0.748582462954855,-1.,1.73550351679848));
#18930=CARTESIAN_POINT('Ctrl Pts',(-0.746574710096436,-1.,1.72958533647399));
#18931=CARTESIAN_POINT('Ctrl Pts',(-0.744021445433764,-1.,1.7226822991693));
#18932=CARTESIAN_POINT('Ctrl Pts',(-0.740795162032088,-1.,1.71447789751927));
#18933=CARTESIAN_POINT('Ctrl Pts',(-0.736799665724771,-1.,1.70473309006121));
#18934=CARTESIAN_POINT('Ctrl Pts',(-0.731963238697195,-1.,1.69326921975743));
#18935=CARTESIAN_POINT('Ctrl Pts',(-0.726235967997433,-1.,1.67996158455503));
#18936=CARTESIAN_POINT('Ctrl Pts',(-0.719585433804282,-1.,1.6647288055568));
#18937=CARTESIAN_POINT('Ctrl Pts',(-0.711993139355394,-1.,1.64752408832016));
#18938=CARTESIAN_POINT('Ctrl Pts',(-0.705159151988319,-1.,1.63216541664676));
#18939=CARTESIAN_POINT('Ctrl Pts',(-0.699605146405088,-1.,1.61974673472612));
#18940=CARTESIAN_POINT('Ctrl Pts',(-0.695712097881194,-1.,1.61106790958151));
#18941=CARTESIAN_POINT('Ctrl Pts',(-0.693717979106306,-1.,1.60662857109684));
#18942=CARTESIAN_POINT('',(-0.892032620296855,-1.,1.5055822144029));
#18943=CARTESIAN_POINT('Origin',(0.,-1.,0.));
#18944=CARTESIAN_POINT('',(-1.23627494547115,-1.,1.81978687191668));
#18945=CARTESIAN_POINT('Ctrl Pts',(-0.892032620296855,-1.,1.5055822144029));
#18946=CARTESIAN_POINT('Ctrl Pts',(-0.894452006964543,-1.,1.50980486806688));
#18947=CARTESIAN_POINT('Ctrl Pts',(-0.899185047483511,-1.,1.51805569590094));
#18948=CARTESIAN_POINT('Ctrl Pts',(-0.905967409625651,-1.,1.52984849887993));
#18949=CARTESIAN_POINT('Ctrl Pts',(-0.914375919026456,-1.,1.54440491149498));
#18950=CARTESIAN_POINT('Ctrl Pts',(-0.923832188944341,-1.,1.56065988578893));
#18951=CARTESIAN_POINT('Ctrl Pts',(-0.932246680108685,-1.,1.57499388382243));
#18952=CARTESIAN_POINT('Ctrl Pts',(-0.939646377893399,-1.,1.58744937487176));
#18953=CARTESIAN_POINT('Ctrl Pts',(-0.946078063315257,-1.,1.59810042043673));
#18954=CARTESIAN_POINT('Ctrl Pts',(-0.951613284356035,-1.,1.60706069896936));
#18955=CARTESIAN_POINT('Ctrl Pts',(-0.956354422920671,-1.,1.61449324337085));
#18956=CARTESIAN_POINT('Ctrl Pts',(-0.960438326101729,-1.,1.62061638140221));
#18957=CARTESIAN_POINT('Ctrl Pts',(-0.964046107040536,-1.,1.62571930670187));
#18958=CARTESIAN_POINT('Ctrl Pts',(-0.967387853230345,-1.,1.63013849959461));
#18959=CARTESIAN_POINT('Ctrl Pts',(-0.970669715997509,-1.,1.63420665729798));
#18960=CARTESIAN_POINT('Ctrl Pts',(-0.974066058287418,-1.,1.63820952658144));
#18961=CARTESIAN_POINT('Ctrl Pts',(-0.977689794119416,-1.,1.64233990826687));
#18962=CARTESIAN_POINT('Ctrl Pts',(-0.981562530939489,-1.,1.64665139190656));
#18963=CARTESIAN_POINT('Ctrl Pts',(-0.985642622920821,-1.,1.65110016612638));
#18964=CARTESIAN_POINT('Ctrl Pts',(-0.989855627854165,-1.,1.65559044289699));
#18965=CARTESIAN_POINT('Ctrl Pts',(-0.994121836661306,-1.,1.66001553809947));
#18966=CARTESIAN_POINT('Ctrl Pts',(-0.998389654952758,-1.,1.66430758030376));
#18967=CARTESIAN_POINT('Ctrl Pts',(-1.00265091003727,-1.,1.66846059277303));
#18968=CARTESIAN_POINT('Ctrl Pts',(-1.00692206696414,-1.,1.67250335383293));
#18969=CARTESIAN_POINT('Ctrl Pts',(-1.01123236493511,-1.,1.67648246776464));
#18970=CARTESIAN_POINT('Ctrl Pts',(-1.01561026162773,-1.,1.68044289894798));
#18971=CARTESIAN_POINT('Ctrl Pts',(-1.02006795074201,-1.,1.68440578021706));
#18972=CARTESIAN_POINT('Ctrl Pts',(-1.02460180535255,-1.,1.68836910178447));
#18973=CARTESIAN_POINT('Ctrl Pts',(-1.02919977579147,-1.,1.69231840863458));
#18974=CARTESIAN_POINT('Ctrl Pts',(-1.03384646003588,-1.,1.69623414782771));
#18975=CARTESIAN_POINT('Ctrl Pts',(-1.03852922490789,-1.,1.70010052930962));
#18976=CARTESIAN_POINT('Ctrl Pts',(-1.04324363334554,-1.,1.70391338707982));
#18977=CARTESIAN_POINT('Ctrl Pts',(-1.04799085404995,-1.,1.70767646263649));
#18978=CARTESIAN_POINT('Ctrl Pts',(-1.05277517202855,-1.,1.71139783543989));
#18979=CARTESIAN_POINT('Ctrl Pts',(-1.05760163192479,-1.,1.7150865442702));
#18980=CARTESIAN_POINT('Ctrl Pts',(-1.06247324680647,-1.,1.71874858456904));
#18981=CARTESIAN_POINT('Ctrl Pts',(-1.06738966975462,-1.,1.72238500928453));
#18982=CARTESIAN_POINT('Ctrl Pts',(-1.07234866990252,-1.,1.72599406198488));
#18983=CARTESIAN_POINT('Ctrl Pts',(-1.0773470373727,-1.,1.72957248977424));
#18984=CARTESIAN_POINT('Ctrl Pts',(-1.08238162784749,-1.,1.73311705663407));
#18985=CARTESIAN_POINT('Ctrl Pts',(-1.08745056285427,-1.,1.73662628326091));
#18986=CARTESIAN_POINT('Ctrl Pts',(-1.09255329056493,-1.,1.74010053962247));
#18987=CARTESIAN_POINT('Ctrl Pts',(-1.09768999241225,-1.,1.74354119236208));
#18988=CARTESIAN_POINT('Ctrl Pts',(-1.10286118991143,-1.,1.74695004214923));
#18989=CARTESIAN_POINT('Ctrl Pts',(-1.10806728183007,-1.,1.7503286607592));
#18990=CARTESIAN_POINT('Ctrl Pts',(-1.11330807582551,-1.,1.7536777209463));
#18991=CARTESIAN_POINT('Ctrl Pts',(-1.11858293216763,-1.,1.75699720772105));
#18992=CARTESIAN_POINT('Ctrl Pts',(-1.12389096855086,-1.,1.76028671825096));
#18993=CARTESIAN_POINT('Ctrl Pts',(-1.12923123555075,-1.,1.7635457196617));
#18994=CARTESIAN_POINT('Ctrl Pts',(-1.1346029180462,-1.,1.76677384551862));
#18995=CARTESIAN_POINT('Ctrl Pts',(-1.14000548336975,-1.,1.76997111386769));
#18996=CARTESIAN_POINT('Ctrl Pts',(-1.1454385822692,-1.,1.77313777896194));
#18997=CARTESIAN_POINT('Ctrl Pts',(-1.15090197841515,-1.,1.7762742255701));
#18998=CARTESIAN_POINT('Ctrl Pts',(-1.15639547194698,-1.,1.77938085564275));
#18999=CARTESIAN_POINT('Ctrl Pts',(-1.16191881298499,-1.,1.78245795881009));
#19000=CARTESIAN_POINT('Ctrl Pts',(-1.16747166312303,-1.,1.78550566040443));
#19001=CARTESIAN_POINT('Ctrl Pts',(-1.17305363177328,-1.,1.78852398877616));
#19002=CARTESIAN_POINT('Ctrl Pts',(-1.17866429440809,-1.,1.79151291552689));
#19003=CARTESIAN_POINT('Ctrl Pts',(-1.18430321697432,-1.,1.79447240321515));
#19004=CARTESIAN_POINT('Ctrl Pts',(-1.18996997934445,-1.,1.79740245923478));
#19005=CARTESIAN_POINT('Ctrl Pts',(-1.19566418930242,-1.,1.80030314369879));
#19006=CARTESIAN_POINT('Ctrl Pts',(-1.20138548938974,-1.,1.80317454838603));
#19007=CARTESIAN_POINT('Ctrl Pts',(-1.20713356605475,-1.,1.80601678480707));
#19008=CARTESIAN_POINT('Ctrl Pts',(-1.21290815708314,-1.,1.80882996917129));
#19009=CARTESIAN_POINT('Ctrl Pts',(-1.21870906103557,-1.,1.81161420806656));
#19010=CARTESIAN_POINT('Ctrl Pts',(-1.2245361330495,-1.,1.81436959210434));
#19011=CARTESIAN_POINT('Ctrl Pts',(-1.2292186489137,-1.,1.8165508718364));
#19012=CARTESIAN_POINT('Ctrl Pts',(-1.2327422452705,-1.,1.81817389921279));
#19013=CARTESIAN_POINT('Ctrl Pts',(-1.23509651170476,-1.,1.81925017193666));
#19014=CARTESIAN_POINT('Ctrl Pts',(-1.23627494547115,-1.,1.81978687191668));
#19015=CARTESIAN_POINT('',(-1.34869019493419,-1.,1.73811241238545));
#19016=CARTESIAN_POINT('',(-1.23627494547115,-1.,1.81978687191668));
#19017=CARTESIAN_POINT('',(-1.15624053661742,-1.,1.31362392696032));
#19018=CARTESIAN_POINT('Ctrl Pts',(-1.34869019493419,-1.,1.73811241238545));
#19019=CARTESIAN_POINT('Ctrl Pts',(-1.34854391898045,-1.,1.73682580585691));
#19020=CARTESIAN_POINT('Ctrl Pts',(-1.34824783112887,-1.,1.73425417885907));
#19021=CARTESIAN_POINT('Ctrl Pts',(-1.34779309152035,-1.,1.7304014965394));
#19022=CARTESIAN_POINT('Ctrl Pts',(-1.34716554819527,-1.,1.72527410680674));
#19023=CARTESIAN_POINT('Ctrl Pts',(-1.34634568653227,-1.,1.7188807715049));
#19024=CARTESIAN_POINT('Ctrl Pts',(-1.34549029589416,-1.,1.71250340686822));
#19025=CARTESIAN_POINT('Ctrl Pts',(-1.34459924533831,-1.,1.70614212266738));
#19026=CARTESIAN_POINT('Ctrl Pts',(-1.34367237124483,-1.,1.69979707754427));
#19027=CARTESIAN_POINT('Ctrl Pts',(-1.34270948206319,-1.,1.6934684849687));
#19028=CARTESIAN_POINT('Ctrl Pts',(-1.341710374848,-1.,1.68715660868764));
#19029=CARTESIAN_POINT('Ctrl Pts',(-1.34067485185203,-1.,1.68086176030362));
#19030=CARTESIAN_POINT('Ctrl Pts',(-1.3396027347034,-1.,1.67458429426086));
#19031=CARTESIAN_POINT('Ctrl Pts',(-1.33849388654388,-1.,1.66832460783989));
#19032=CARTESIAN_POINT('Ctrl Pts',(-1.33734820885262,-1.,1.66208312541983));
#19033=CARTESIAN_POINT('Ctrl Pts',(-1.33616559745172,-1.,1.65586025952593));
#19034=CARTESIAN_POINT('Ctrl Pts',(-1.33494590467993,-1.,1.6496563728683));
#19035=CARTESIAN_POINT('Ctrl Pts',(-1.33368890676572,-1.,1.6434717485603));
#19036=CARTESIAN_POINT('Ctrl Pts',(-1.33239425103724,-1.,1.63730653475089));
#19037=CARTESIAN_POINT('Ctrl Pts',(-1.33106149345645,-1.,1.63116079730923));
#19038=CARTESIAN_POINT('Ctrl Pts',(-1.3296901950568,-1.,1.62503464209797));
#19039=CARTESIAN_POINT('Ctrl Pts',(-1.32828000610449,-1.,1.61892832270724));
#19040=CARTESIAN_POINT('Ctrl Pts',(-1.32683074483356,-1.,1.6128423401575));
#19041=CARTESIAN_POINT('Ctrl Pts',(-1.32534250785782,-1.,1.60677758290954));
#19042=CARTESIAN_POINT('Ctrl Pts',(-1.32381550858256,-1.,1.60073511858687));
#19043=CARTESIAN_POINT('Ctrl Pts',(-1.32224985747682,-1.,1.59471591079403));
#19044=CARTESIAN_POINT('Ctrl Pts',(-1.32064537110892,-1.,1.58872057258245));
#19045=CARTESIAN_POINT('Ctrl Pts',(-1.31900135021432,-1.,1.58274907898834));
#19046=CARTESIAN_POINT('Ctrl Pts',(-1.31731642317187,-1.,1.5768005650559));
#19047=CARTESIAN_POINT('Ctrl Pts',(-1.31558903860016,-1.,1.57087397835723));
#19048=CARTESIAN_POINT('Ctrl Pts',(-1.31381795281002,-1.,1.56496872402353));
#19049=CARTESIAN_POINT('Ctrl Pts',(-1.31200264341696,-1.,1.55908521254821));
#19050=CARTESIAN_POINT('Ctrl Pts',(-1.31014393684222,-1.,1.55322568759481));
#19051=CARTESIAN_POINT('Ctrl Pts',(-1.30824393907473,-1.,1.54739413957185));
#19052=CARTESIAN_POINT('Ctrl Pts',(-1.30630475189556,-1.,1.54159462645432));
#19053=CARTESIAN_POINT('Ctrl Pts',(-1.30432735639489,-1.,1.53582981268977));
#19054=CARTESIAN_POINT('Ctrl Pts',(-1.30231064395568,-1.,1.53009970283891));
#19055=CARTESIAN_POINT('Ctrl Pts',(-1.30024984366328,-1.,1.52439957861062));
#19056=CARTESIAN_POINT('Ctrl Pts',(-1.29813791800747,-1.,1.51872184912724));
#19057=CARTESIAN_POINT('Ctrl Pts',(-1.29596850710509,-1.,1.51305994241402));
#19058=CARTESIAN_POINT('Ctrl Pts',(-1.29373841372842,-1.,1.50741159078365));
#19059=CARTESIAN_POINT('Ctrl Pts',(-1.29145022885181,-1.,1.50178230149776));
#19060=CARTESIAN_POINT('Ctrl Pts',(-1.28911506584254,-1.,1.49618896881754));
#19061=CARTESIAN_POINT('Ctrl Pts',(-1.2867467611644,-1.,1.4906522831278));
#19062=CARTESIAN_POINT('Ctrl Pts',(-1.28435533880201,-1.,1.4851881711891));
#19063=CARTESIAN_POINT('Ctrl Pts',(-1.28194158939517,-1.,1.47980070347095));
#19064=CARTESIAN_POINT('Ctrl Pts',(-1.2794891824849,-1.,1.4744717526707));
#19065=CARTESIAN_POINT('Ctrl Pts',(-1.27696414831089,-1.,1.46916035917133));
#19066=CARTESIAN_POINT('Ctrl Pts',(-1.27433119897822,-1.,1.46382431332476));
#19067=CARTESIAN_POINT('Ctrl Pts',(-1.27156805265289,-1.,1.45843906294697));
#19068=CARTESIAN_POINT('Ctrl Pts',(-1.2686778680489,-1.,1.45301422764247));
#19069=CARTESIAN_POINT('Ctrl Pts',(-1.26570925118868,-1.,1.44761985001662));
#19070=CARTESIAN_POINT('Ctrl Pts',(-1.26273903323859,-1.,1.44236470511303));
#19071=CARTESIAN_POINT('Ctrl Pts',(-1.25983531012005,-1.,1.43734919180848));
#19072=CARTESIAN_POINT('Ctrl Pts',(-1.25702687965755,-1.,1.43262645609691));
#19073=CARTESIAN_POINT('Ctrl Pts',(-1.25426945222639,-1.,1.42815938799387));
#19074=CARTESIAN_POINT('Ctrl Pts',(-1.2514145557001,-1.,1.42378102115575));
#19075=CARTESIAN_POINT('Ctrl Pts',(-1.24824430986571,-1.,1.41923722596025));
#19076=CARTESIAN_POINT('Ctrl Pts',(-1.24450600513056,-1.,1.41422913175179));
#19077=CARTESIAN_POINT('Ctrl Pts',(-1.23994455029534,-1.,1.40845295531283));
#19078=CARTESIAN_POINT('Ctrl Pts',(-1.23434087290423,-1.,1.40164708206106));
#19079=CARTESIAN_POINT('Ctrl Pts',(-1.22752961899387,-1.,1.39361389568796));
#19080=CARTESIAN_POINT('Ctrl Pts',(-1.21938737280852,-1.,1.38420564527715));
#19081=CARTESIAN_POINT('Ctrl Pts',(-1.20982812925645,-1.,1.37331915607905));
#19082=CARTESIAN_POINT('Ctrl Pts',(-1.1987959077932,-1.,1.36088705043885));
#19083=CARTESIAN_POINT('Ctrl Pts',(-1.18625865667441,-1.,1.34687054001093));
#19084=CARTESIAN_POINT('Ctrl Pts',(-1.17501305789857,-1.,1.33437539347008));
#19085=CARTESIAN_POINT('Ctrl Pts',(-1.16589330093588,-1.,1.32428080721772));
#19086=CARTESIAN_POINT('Ctrl Pts',(-1.15950888730809,-1.,1.31722977216397));
#19087=CARTESIAN_POINT('Ctrl Pts',(-1.15624053661742,-1.,1.31362392696032));
#19088=CARTESIAN_POINT('',(-1.31362392696033,-1.,1.15624053661742));
#19089=CARTESIAN_POINT('Origin',(0.,-1.,0.));
#19090=CARTESIAN_POINT('',(-1.73811241238545,-1.,1.34869019493419));
#19091=CARTESIAN_POINT('Ctrl Pts',(-1.31362392696033,-1.,1.15624053661742));
#19092=CARTESIAN_POINT('Ctrl Pts',(-1.3172297721596,-1.,1.15950888730433));
#19093=CARTESIAN_POINT('Ctrl Pts',(-1.32428080720544,-1.,1.16589330092532));
#19094=CARTESIAN_POINT('Ctrl Pts',(-1.33437539344842,-1.,1.17501305787994));
#19095=CARTESIAN_POINT('Ctrl Pts',(-1.34687053998157,-1.,1.18625865664915));
#19096=CARTESIAN_POINT('Ctrl Pts',(-1.36088705040677,-1.,1.1987959077656));
#19097=CARTESIAN_POINT('Ctrl Pts',(-1.37331915604962,-1.,1.20982812923113));
#19098=CARTESIAN_POINT('Ctrl Pts',(-1.38420564525391,-1.,1.21938737278853));
#19099=CARTESIAN_POINT('Ctrl Pts',(-1.39361389567257,-1.,1.22752961898063));
#19100=CARTESIAN_POINT('Ctrl Pts',(-1.40164708205345,-1.,1.23434087289768));
#19101=CARTESIAN_POINT('Ctrl Pts',(-1.40845295531151,-1.,1.23994455029421));
#19102=CARTESIAN_POINT('Ctrl Pts',(-1.41422913175437,-1.,1.24450600513278));
#19103=CARTESIAN_POINT('Ctrl Pts',(-1.41923722596421,-1.,1.24824430986911));
#19104=CARTESIAN_POINT('Ctrl Pts',(-1.42378102115911,-1.,1.25141455570299));
#19105=CARTESIAN_POINT('Ctrl Pts',(-1.42815938799555,-1.,1.25426945222783));
#19106=CARTESIAN_POINT('Ctrl Pts',(-1.43262645609679,-1.,1.25702687965744));
#19107=CARTESIAN_POINT('Ctrl Pts',(-1.43734919180719,-1.,1.25983531011894));
#19108=CARTESIAN_POINT('Ctrl Pts',(-1.44236470511145,-1.,1.26273903323723));
#19109=CARTESIAN_POINT('Ctrl Pts',(-1.44761985001544,-1.,1.26570925118767));
#19110=CARTESIAN_POINT('Ctrl Pts',(-1.45301422764205,-1.,1.26867786804854));
#19111=CARTESIAN_POINT('Ctrl Pts',(-1.45843906294725,-1.,1.27156805265312));
#19112=CARTESIAN_POINT('Ctrl Pts',(-1.4638243133254,-1.,1.27433119897877));
#19113=CARTESIAN_POINT('Ctrl Pts',(-1.46916035917197,-1.,1.27696414831144));
#19114=CARTESIAN_POINT('Ctrl Pts',(-1.4744717526711,-1.,1.27948918248524));
#19115=CARTESIAN_POINT('Ctrl Pts',(-1.47980070347102,-1.,1.28194158939522));
#19116=CARTESIAN_POINT('Ctrl Pts',(-1.48518817118891,-1.,1.28435533880184));
#19117=CARTESIAN_POINT('Ctrl Pts',(-1.4906522831275,-1.,1.28674676116415));
#19118=CARTESIAN_POINT('Ctrl Pts',(-1.49618896881729,-1.,1.28911506584232));
#19119=CARTESIAN_POINT('Ctrl Pts',(-1.50178230149764,-1.,1.29145022885171));
#19120=CARTESIAN_POINT('Ctrl Pts',(-1.50741159078367,-1.,1.29373841372843));
#19121=CARTESIAN_POINT('Ctrl Pts',(-1.51305994241412,-1.,1.29596850710518));
#19122=CARTESIAN_POINT('Ctrl Pts',(-1.51872184912735,-1.,1.29813791800757));
#19123=CARTESIAN_POINT('Ctrl Pts',(-1.5243995786107,-1.,1.30024984366334));
#19124=CARTESIAN_POINT('Ctrl Pts',(-1.53009970283893,-1.,1.3023106439557));
#19125=CARTESIAN_POINT('Ctrl Pts',(-1.53582981268976,-1.,1.30432735639487));
#19126=CARTESIAN_POINT('Ctrl Pts',(-1.54159462645428,-1.,1.30630475189553));
#19127=CARTESIAN_POINT('Ctrl Pts',(-1.54739413957183,-1.,1.30824393907471));
#19128=CARTESIAN_POINT('Ctrl Pts',(-1.55322568759481,-1.,1.31014393684221));
#19129=CARTESIAN_POINT('Ctrl Pts',(-1.55908521254822,-1.,1.31200264341696));
#19130=CARTESIAN_POINT('Ctrl Pts',(-1.56496872402352,-1.,1.31381795281002));
#19131=CARTESIAN_POINT('Ctrl Pts',(-1.57087397835721,-1.,1.31558903860015));
#19132=CARTESIAN_POINT('Ctrl Pts',(-1.57680056505585,-1.,1.31731642317183));
#19133=CARTESIAN_POINT('Ctrl Pts',(-1.58274907898829,-1.,1.31900135021428));
#19134=CARTESIAN_POINT('Ctrl Pts',(-1.58872057258244,-1.,1.32064537110891));
#19135=CARTESIAN_POINT('Ctrl Pts',(-1.59471591079408,-1.,1.32224985747686));
#19136=CARTESIAN_POINT('Ctrl Pts',(-1.600735118587,-1.,1.32381550858266));
#19137=CARTESIAN_POINT('Ctrl Pts',(-1.6067775829097,-1.,1.32534250785794));
#19138=CARTESIAN_POINT('Ctrl Pts',(-1.61284234015762,-1.,1.32683074483365));
#19139=CARTESIAN_POINT('Ctrl Pts',(-1.61892832270723,-1.,1.32828000610448));
#19140=CARTESIAN_POINT('Ctrl Pts',(-1.62503464209777,-1.,1.32969019505665));
#19141=CARTESIAN_POINT('Ctrl Pts',(-1.63116079730887,-1.,1.33106149345618));
#19142=CARTESIAN_POINT('Ctrl Pts',(-1.6373065347505,-1.,1.33239425103694));
#19143=CARTESIAN_POINT('Ctrl Pts',(-1.64347174856007,-1.,1.33368890676554));
#19144=CARTESIAN_POINT('Ctrl Pts',(-1.64965637286843,-1.,1.33494590468003));
#19145=CARTESIAN_POINT('Ctrl Pts',(-1.65586025952651,-1.,1.33616559745217));
#19146=CARTESIAN_POINT('Ctrl Pts',(-1.66208312542073,-1.,1.33734820885331));
#19147=CARTESIAN_POINT('Ctrl Pts',(-1.66832460784078,-1.,1.33849388654458));
#19148=CARTESIAN_POINT('Ctrl Pts',(-1.67458429426126,-1.,1.33960273470372));
#19149=CARTESIAN_POINT('Ctrl Pts',(-1.68086176030308,-1.,1.3406748518516));
#19150=CARTESIAN_POINT('Ctrl Pts',(-1.68715660868602,-1.,1.34171037484673));
#19151=CARTESIAN_POINT('Ctrl Pts',(-1.6934684849664,-1.,1.34270948206139));
#19152=CARTESIAN_POINT('Ctrl Pts',(-1.69979707754221,-1.,1.34367237124322));
#19153=CARTESIAN_POINT('Ctrl Pts',(-1.70614212266676,-1.,1.34459924533783));
#19154=CARTESIAN_POINT('Ctrl Pts',(-1.71250340687011,-1.,1.34549029589563));
#19155=CARTESIAN_POINT('Ctrl Pts',(-1.7188807715095,-1.,1.34634568653586));
#19156=CARTESIAN_POINT('Ctrl Pts',(-1.72527410681298,-1.,1.34716554820013));
#19157=CARTESIAN_POINT('Ctrl Pts',(-1.73040149654497,-1.,1.3477930915247));
#19158=CARTESIAN_POINT('Ctrl Pts',(-1.73425417886255,-1.,1.34824783113158));
#19159=CARTESIAN_POINT('Ctrl Pts',(-1.73682580585819,-1.,1.34854391898145));
#19160=CARTESIAN_POINT('Ctrl Pts',(-1.73811241238545,-1.,1.34869019493419));
#19161=CARTESIAN_POINT('',(-1.81978687191668,-1.,1.23627494547115));
#19162=CARTESIAN_POINT('',(-1.73811241238545,-1.,1.34869019493419));
#19163=CARTESIAN_POINT('',(-1.5055822144029,-1.,0.892032620296855));
#19164=CARTESIAN_POINT('Ctrl Pts',(-1.81978687191668,-1.,1.23627494547115));
#19165=CARTESIAN_POINT('Ctrl Pts',(-1.81925017193531,-1.,1.23509651170384));
#19166=CARTESIAN_POINT('Ctrl Pts',(-1.81817389920914,-1.,1.23274224526804));
#19167=CARTESIAN_POINT('Ctrl Pts',(-1.81655087183054,-1.,1.22921864890975));
#19168=CARTESIAN_POINT('Ctrl Pts',(-1.81436959209778,-1.,1.22453613304507));
#19169=CARTESIAN_POINT('Ctrl Pts',(-1.81161420806172,-1.,1.2187090610323));
#19170=CARTESIAN_POINT('Ctrl Pts',(-1.80882996916931,-1.,1.2129081570818));
#19171=CARTESIAN_POINT('Ctrl Pts',(-1.80601678480772,-1.,1.20713356605519));
#19172=CARTESIAN_POINT('Ctrl Pts',(-1.8031745483882,-1.,1.2013854893912));
#19173=CARTESIAN_POINT('Ctrl Pts',(-1.80030314370121,-1.,1.19566418930405));
#19174=CARTESIAN_POINT('Ctrl Pts',(-1.79740245923649,-1.,1.1899699793456));
#19175=CARTESIAN_POINT('Ctrl Pts',(-1.79447240321572,-1.,1.18430321697471));
#19176=CARTESIAN_POINT('Ctrl Pts',(-1.79151291552646,-1.,1.17866429440781));
#19177=CARTESIAN_POINT('Ctrl Pts',(-1.78852398877523,-1.,1.17305363177265));
#19178=CARTESIAN_POINT('Ctrl Pts',(-1.78550566040349,-1.,1.16747166312239));
#19179=CARTESIAN_POINT('Ctrl Pts',(-1.78245795880949,-1.,1.16191881298458));
#19180=CARTESIAN_POINT('Ctrl Pts',(-1.77938085564261,-1.,1.15639547194689));
#19181=CARTESIAN_POINT('Ctrl Pts',(-1.77627422557034,-1.,1.15090197841531));
#19182=CARTESIAN_POINT('Ctrl Pts',(-1.77313777896234,-1.,1.14543858226948));
#19183=CARTESIAN_POINT('Ctrl Pts',(-1.76997111386806,-1.,1.14000548337));
#19184=CARTESIAN_POINT('Ctrl Pts',(-1.76677384551883,-1.,1.13460291804635));
#19185=CARTESIAN_POINT('Ctrl Pts',(-1.76354571966171,-1.,1.12923123555076));
#19186=CARTESIAN_POINT('Ctrl Pts',(-1.76028671825084,-1.,1.12389096855078));
#19187=CARTESIAN_POINT('Ctrl Pts',(-1.75699720772089,-1.,1.11858293216752));
#19188=CARTESIAN_POINT('Ctrl Pts',(-1.75367772094617,-1.,1.11330807582542));
#19189=CARTESIAN_POINT('Ctrl Pts',(-1.75032866075914,-1.,1.10806728183003));
#19190=CARTESIAN_POINT('Ctrl Pts',(-1.74695004214924,-1.,1.10286118991144));
#19191=CARTESIAN_POINT('Ctrl Pts',(-1.74354119236212,-1.,1.09768999241229));
#19192=CARTESIAN_POINT('Ctrl Pts',(-1.74010053962252,-1.,1.09255329056496));
#19193=CARTESIAN_POINT('Ctrl Pts',(-1.73662628326093,-1.,1.08745056285429));
#19194=CARTESIAN_POINT('Ctrl Pts',(-1.73311705663407,-1.,1.08238162784749));
#19195=CARTESIAN_POINT('Ctrl Pts',(-1.72957248977424,-1.,1.0773470373727));
#19196=CARTESIAN_POINT('Ctrl Pts',(-1.72599406198489,-1.,1.07234866990252));
#19197=CARTESIAN_POINT('Ctrl Pts',(-1.72238500928456,-1.,1.06738966975463));
#19198=CARTESIAN_POINT('Ctrl Pts',(-1.71874858456908,-1.,1.0624732468065));
#19199=CARTESIAN_POINT('Ctrl Pts',(-1.71508654427022,-1.,1.05760163192481));
#19200=CARTESIAN_POINT('Ctrl Pts',(-1.71139783543986,-1.,1.05277517202854));
#19201=CARTESIAN_POINT('Ctrl Pts',(-1.70767646263641,-1.,1.0479908540499));
#19202=CARTESIAN_POINT('Ctrl Pts',(-1.70391338707969,-1.,1.04324363334546));
#19203=CARTESIAN_POINT('Ctrl Pts',(-1.70010052930951,-1.,1.03852922490782));
#19204=CARTESIAN_POINT('Ctrl Pts',(-1.69623414782769,-1.,1.03384646003587));
#19205=CARTESIAN_POINT('Ctrl Pts',(-1.69231840863471,-1.,1.02919977579155));
#19206=CARTESIAN_POINT('Ctrl Pts',(-1.68836910178475,-1.,1.02460180535272));
#19207=CARTESIAN_POINT('Ctrl Pts',(-1.68440578021739,-1.,1.02006795074222));
#19208=CARTESIAN_POINT('Ctrl Pts',(-1.6804428989482,-1.,1.01561026162787));
#19209=CARTESIAN_POINT('Ctrl Pts',(-1.67648246776457,-1.,1.01123236493507));
#19210=CARTESIAN_POINT('Ctrl Pts',(-1.67250335383248,-1.,1.00692206696387));
#19211=CARTESIAN_POINT('Ctrl Pts',(-1.66846059277231,-1.,1.00265091003682));
#19212=CARTESIAN_POINT('Ctrl Pts',(-1.66430758030304,-1.,0.998389654952317));
#19213=CARTESIAN_POINT('Ctrl Pts',(-1.66001553809916,-1.,0.994121836661116));
#19214=CARTESIAN_POINT('Ctrl Pts',(-1.65559044289746,-1.,0.98985562785445));
#19215=CARTESIAN_POINT('Ctrl Pts',(-1.6511001661277,-1.,0.985642622921626));
#19216=CARTESIAN_POINT('Ctrl Pts',(-1.64665139190834,-1.,0.981562530940574));
#19217=CARTESIAN_POINT('Ctrl Pts',(-1.64233990826831,-1.,0.977689794120297));
#19218=CARTESIAN_POINT('Ctrl Pts',(-1.63820952658157,-1.,0.974066058287501));
#19219=CARTESIAN_POINT('Ctrl Pts',(-1.63420665729609,-1.,0.970669715996356));
#19220=CARTESIAN_POINT('Ctrl Pts',(-1.63013849959083,-1.,0.967387853228041));
#19221=CARTESIAN_POINT('Ctrl Pts',(-1.6257193066974,-1.,0.964046107037821));
#19222=CARTESIAN_POINT('Ctrl Pts',(-1.62061638139929,-1.,0.960438326099958));
#19223=CARTESIAN_POINT('Ctrl Pts',(-1.61449324337233,-1.,0.956354422921573));
#19224=CARTESIAN_POINT('Ctrl Pts',(-1.60706069897794,-1.,0.951613284361248));
#19225=CARTESIAN_POINT('Ctrl Pts',(-1.59810042045408,-1.,0.946078063325796));
#19226=CARTESIAN_POINT('Ctrl Pts',(-1.58744937489796,-1.,0.939646377909319));
#19227=CARTESIAN_POINT('Ctrl Pts',(-1.57499388385561,-1.,0.932246680128849));
#19228=CARTESIAN_POINT('Ctrl Pts',(-1.56065988582509,-1.,0.923832188966322));
#19229=CARTESIAN_POINT('Ctrl Pts',(-1.54440491152808,-1.,0.91437591904658));
#19230=CARTESIAN_POINT('Ctrl Pts',(-1.52984849890434,-1.,0.905967409640499));
#19231=CARTESIAN_POINT('Ctrl Pts',(-1.51805569591479,-1.,0.89918504749193));
#19232=CARTESIAN_POINT('Ctrl Pts',(-1.50980486807181,-1.,0.894452006967538));
#19233=CARTESIAN_POINT('Ctrl Pts',(-1.5055822144029,-1.,0.892032620296855));
#19234=CARTESIAN_POINT('',(-1.60662857109684,-1.,0.693717979106305));
#19235=CARTESIAN_POINT('Origin',(0.,-1.,0.));
#19236=CARTESIAN_POINT('',(-2.0698113262342,-1.,0.7455743247944));
#19237=CARTESIAN_POINT('Ctrl Pts',(-1.60662857109684,-1.,0.693717979106305));
#19238=CARTESIAN_POINT('Ctrl Pts',(-1.61106790957619,-1.,0.69571209787897));
#19239=CARTESIAN_POINT('Ctrl Pts',(-1.61974673471117,-1.,0.699605146398837));
#19240=CARTESIAN_POINT('Ctrl Pts',(-1.6321654166204,-1.,0.705159151977294));
#19241=CARTESIAN_POINT('Ctrl Pts',(-1.64752408828442,-1.,0.711993139340447));
#19242=CARTESIAN_POINT('Ctrl Pts',(-1.66472880551777,-1.,0.71958543378795));
#19243=CARTESIAN_POINT('Ctrl Pts',(-1.67996158451922,-1.,0.726235967982445));
#19244=CARTESIAN_POINT('Ctrl Pts',(-1.69326921972915,-1.,0.731963238685357));
#19245=CARTESIAN_POINT('Ctrl Pts',(-1.70473309004249,-1.,0.736799665716932));
#19246=CARTESIAN_POINT('Ctrl Pts',(-1.71447789751001,-1.,0.74079516202821));
#19247=CARTESIAN_POINT('Ctrl Pts',(-1.72268229916769,-1.,0.744021445433093));
#19248=CARTESIAN_POINT('Ctrl Pts',(-1.72958533647714,-1.,0.746574710097752));
#19249=CARTESIAN_POINT('Ctrl Pts',(-1.7355035168033,-1.,0.74858246295687));
#19250=CARTESIAN_POINT('Ctrl Pts',(-1.74080458267114,-1.,0.750193435981249));
#19251=CARTESIAN_POINT('Ctrl Pts',(-1.74585086852502,-1.,0.751555614164482));
#19252=CARTESIAN_POINT('Ctrl Pts',(-1.75095139468794,-1.,0.752797683531314));
#19253=CARTESIAN_POINT('Ctrl Pts',(-1.75631083600019,-1.,0.754009254027829));
#19254=CARTESIAN_POINT('Ctrl Pts',(-1.76197817240128,-1.,0.755220979974461));
#19255=CARTESIAN_POINT('Ctrl Pts',(-1.76789396002998,-1.,0.75642189602781));
#19256=CARTESIAN_POINT('Ctrl Pts',(-1.77394167108292,-1.,0.757578264077029));
#19257=CARTESIAN_POINT('Ctrl Pts',(-1.77999411220945,-1.,0.758650626677518));
#19258=CARTESIAN_POINT('Ctrl Pts',(-1.78596964884604,-1.,0.759614401110189));
#19259=CARTESIAN_POINT('Ctrl Pts',(-1.7918581561088,-1.,0.760469555880749));
#19260=CARTESIAN_POINT('Ctrl Pts',(-1.79768986997783,-1.,0.761229695230558));
#19261=CARTESIAN_POINT('Ctrl Pts',(-1.80351583877342,-1.,0.761915336443547));
#19262=CARTESIAN_POINT('Ctrl Pts',(-1.80938551463965,-1.,0.762546129463938));
#19263=CARTESIAN_POINT('Ctrl Pts',(-1.8153211840553,-1.,0.763132003836634));
#19264=CARTESIAN_POINT('Ctrl Pts',(-1.82131873145266,-1.,0.763673465462726));
#19265=CARTESIAN_POINT('Ctrl Pts',(-1.82735991200065,-1.,0.764165902605995));
#19266=CARTESIAN_POINT('Ctrl Pts',(-1.83342077227142,-1.,0.764602549687853));
#19267=CARTESIAN_POINT('Ctrl Pts',(-1.83948181064835,-1.,0.764978057881737));
#19268=CARTESIAN_POINT('Ctrl Pts',(-1.84553698875924,-1.,0.765291664862029));
#19269=CARTESIAN_POINT('Ctrl Pts',(-1.85158945130063,-1.,0.765545710619062));
#19270=CARTESIAN_POINT('Ctrl Pts',(-1.85764741390394,-1.,0.765744212909318));
#19271=CARTESIAN_POINT('Ctrl Pts',(-1.86372027063312,-1.,0.765891519092547));
#19272=CARTESIAN_POINT('Ctrl Pts',(-1.86981398314341,-1.,0.765990708546091));
#19273=CARTESIAN_POINT('Ctrl Pts',(-1.87592888967883,-1.,0.766042837036744));
#19274=CARTESIAN_POINT('Ctrl Pts',(-1.88206215302561,-1.,0.766047794851864));
#19275=CARTESIAN_POINT('Ctrl Pts',(-1.88820926433409,-1.,0.766004837062091));
#19276=CARTESIAN_POINT('Ctrl Pts',(-1.89436577771388,-1.,0.765913193856978));
#19277=CARTESIAN_POINT('Ctrl Pts',(-1.90052930393596,-1.,0.765772772593386));
#19278=CARTESIAN_POINT('Ctrl Pts',(-1.90669961402356,-1.,0.765584196937919));
#19279=CARTESIAN_POINT('Ctrl Pts',(-1.91287765805169,-1.,0.765348465884722));
#19280=CARTESIAN_POINT('Ctrl Pts',(-1.91906491634196,-1.,0.765066729667088));
#19281=CARTESIAN_POINT('Ctrl Pts',(-1.92526263537048,-1.,0.764740025488211));
#19282=CARTESIAN_POINT('Ctrl Pts',(-1.93147105496382,-1.,0.76436901067394));
#19283=CARTESIAN_POINT('Ctrl Pts',(-1.93768964875886,-1.,0.763954049121458));
#19284=CARTESIAN_POINT('Ctrl Pts',(-1.9439174661764,-1.,0.763495333538629));
#19285=CARTESIAN_POINT('Ctrl Pts',(-1.95015342590024,-1.,0.762992990878769));
#19286=CARTESIAN_POINT('Ctrl Pts',(-1.95639665309869,-1.,0.762447203806179));
#19287=CARTESIAN_POINT('Ctrl Pts',(-1.96264672744186,-1.,0.761858300014423));
#19288=CARTESIAN_POINT('Ctrl Pts',(-1.96890351582499,-1.,0.76122669048382));
#19289=CARTESIAN_POINT('Ctrl Pts',(-1.97516705321494,-1.,0.760552825409757));
#19290=CARTESIAN_POINT('Ctrl Pts',(-1.98143741418172,-1.,0.75983714745219));
#19291=CARTESIAN_POINT('Ctrl Pts',(-1.98771456680874,-1.,0.759080037802488));
#19292=CARTESIAN_POINT('Ctrl Pts',(-1.99399831098817,-1.,0.758281796766761));
#19293=CARTESIAN_POINT('Ctrl Pts',(-2.00028834739178,-1.,0.757442676862724));
#19294=CARTESIAN_POINT('Ctrl Pts',(-2.0065843158773,-1.,0.75656290464667));
#19295=CARTESIAN_POINT('Ctrl Pts',(-2.01288584328084,-1.,0.755642704957865));
#19296=CARTESIAN_POINT('Ctrl Pts',(-2.01919259405809,-1.,0.754682330722816));
#19297=CARTESIAN_POINT('Ctrl Pts',(-2.02550428623313,-1.,0.753682061112768));
#19298=CARTESIAN_POINT('Ctrl Pts',(-2.03182068456221,-1.,0.752642180487211));
#19299=CARTESIAN_POINT('Ctrl Pts',(-2.03814160092099,-1.,0.751562963361115));
#19300=CARTESIAN_POINT('Ctrl Pts',(-2.04446689147979,-1.,0.750444657875576));
#19301=CARTESIAN_POINT('Ctrl Pts',(-2.05079645592154,-1.,0.749287468665046));
#19302=CARTESIAN_POINT('Ctrl Pts',(-2.05713023031006,-1.,0.748091554183802));
#19303=CARTESIAN_POINT('Ctrl Pts',(-2.06220058927826,-1.,0.747103932787919));
#19304=CARTESIAN_POINT('Ctrl Pts',(-2.06600523016815,-1.,0.7463458715442));
#19305=CARTESIAN_POINT('Ctrl Pts',(-2.06854248895728,-1.,0.745832791378367));
#19306=CARTESIAN_POINT('Ctrl Pts',(-2.0698113262342,-1.,0.7455743247944));
#19307=CARTESIAN_POINT('',(-2.11275013067528,-1.,0.61342227326009));
#19308=CARTESIAN_POINT('',(-2.0698113262342,-1.,0.7455743247944));
#19309=CARTESIAN_POINT('',(-1.7075470150345,-1.,0.383122945602004));
#19310=CARTESIAN_POINT('Ctrl Pts',(-2.11275013067528,-1.,0.61342227326009));
#19311=CARTESIAN_POINT('Ctrl Pts',(-2.11187554259986,-1.,0.6124673655618));
#19312=CARTESIAN_POINT('Ctrl Pts',(-2.11012443807238,-1.,0.610560911689899));
#19313=CARTESIAN_POINT('Ctrl Pts',(-2.1074919961518,-1.,0.607711315454876));
#19314=CARTESIAN_POINT('Ctrl Pts',(-2.10397049886949,-1.,0.60393203073603));
#19315=CARTESIAN_POINT('Ctrl Pts',(-2.0995493086477,-1.,0.599241616420533));
#19316=CARTESIAN_POINT('Ctrl Pts',(-2.0951087622027,-1.,0.594585006052162));
#19317=CARTESIAN_POINT('Ctrl Pts',(-2.09064881812129,-1.,0.589962365403406));
#19318=CARTESIAN_POINT('Ctrl Pts',(-2.08616943727951,-1.,0.585373918991617));
#19319=CARTESIAN_POINT('Ctrl Pts',(-2.08167059018418,-1.,0.580819952108063));
#19320=CARTESIAN_POINT('Ctrl Pts',(-2.07715226767559,-1.,0.576300797416844));
#19321=CARTESIAN_POINT('Ctrl Pts',(-2.07261449292824,-1.,0.571816823242603));
#19322=CARTESIAN_POINT('Ctrl Pts',(-2.06805732997334,-1.,0.567368421181087));
#19323=CARTESIAN_POINT('Ctrl Pts',(-2.06348090160589,-1.,0.562955993082261));
#19324=CARTESIAN_POINT('Ctrl Pts',(-2.05888537756462,-1.,0.558579940185151));
#19325=CARTESIAN_POINT('Ctrl Pts',(-2.05427091604413,-1.,0.554240657463906));
#19326=CARTESIAN_POINT('Ctrl Pts',(-2.04963761077958,-1.,0.549938525150295));
#19327=CARTESIAN_POINT('Ctrl Pts',(-2.04498544714588,-1.,0.54567390381743));
#19328=CARTESIAN_POINT('Ctrl Pts',(-2.04031422690527,-1.,0.541447120615659));
#19329=CARTESIAN_POINT('Ctrl Pts',(-2.03562362954037,-1.,0.537258489833262));
#19330=CARTESIAN_POINT('Ctrl Pts',(-2.03091336214426,-1.,0.533108355132976));
#19331=CARTESIAN_POINT('Ctrl Pts',(-2.0261832908329,-1.,0.528997127241914));
#19332=CARTESIAN_POINT('Ctrl Pts',(-2.02143356304698,-1.,0.524925318333476));
#19333=CARTESIAN_POINT('Ctrl Pts',(-2.01666477917286,-1.,0.52089359039937));
#19334=CARTESIAN_POINT('Ctrl Pts',(-2.01187773939242,-1.,0.516902681728687));
#19335=CARTESIAN_POINT('Ctrl Pts',(-2.00707309946949,-1.,0.512953306961792));
#19336=CARTESIAN_POINT('Ctrl Pts',(-2.00225107134734,-1.,0.509046069886157));
#19337=CARTESIAN_POINT('Ctrl Pts',(-1.99741107463572,-1.,0.505181361323026));
#19338=CARTESIAN_POINT('Ctrl Pts',(-1.99255149126155,-1.,0.501359287727146));
#19339=CARTESIAN_POINT('Ctrl Pts',(-1.98767044752932,-1.,0.497579909545574));
#19340=CARTESIAN_POINT('Ctrl Pts',(-1.98276658761821,-1.,0.493843476541494));
#19341=CARTESIAN_POINT('Ctrl Pts',(-1.97783973019229,-1.,0.490150627860952));
#19342=CARTESIAN_POINT('Ctrl Pts',(-1.97289186263272,-1.,0.486502692907659));
#19343=CARTESIAN_POINT('Ctrl Pts',(-1.96792703422362,-1.,0.48290166212069));
#19344=CARTESIAN_POINT('Ctrl Pts',(-1.96294933055943,-1.,0.479349583074855));
#19345=CARTESIAN_POINT('Ctrl Pts',(-1.95796111148177,-1.,0.475848034683176));
#19346=CARTESIAN_POINT('Ctrl Pts',(-1.95296148278133,-1.,0.472397672264072));
#19347=CARTESIAN_POINT('Ctrl Pts',(-1.94794381136514,-1.,0.468997482913135));
#19348=CARTESIAN_POINT('Ctrl Pts',(-1.9428979419619,-1.,0.46564546202603));
#19349=CARTESIAN_POINT('Ctrl Pts',(-1.93781486640821,-1.,0.462340031009056));
#19350=CARTESIAN_POINT('Ctrl Pts',(-1.93269066517934,-1.,0.459081234547926));
#19351=CARTESIAN_POINT('Ctrl Pts',(-1.92753067150476,-1.,0.455872005174371));
#19352=CARTESIAN_POINT('Ctrl Pts',(-1.92235380648502,-1.,0.452719478359432));
#19353=CARTESIAN_POINT('Ctrl Pts',(-1.91718342555755,-1.,0.449632260106662));
#19354=CARTESIAN_POINT('Ctrl Pts',(-1.9120369998112,-1.,0.446617343485711));
#19355=CARTESIAN_POINT('Ctrl Pts',(-1.90691756144898,-1.,0.44367755684915));
#19356=CARTESIAN_POINT('Ctrl Pts',(-1.90180124389086,-1.,0.440807833704038));
#19357=CARTESIAN_POINT('Ctrl Pts',(-1.89663648956466,-1.,0.437995003948244));
#19358=CARTESIAN_POINT('Ctrl Pts',(-1.89136993975504,-1.,0.435225660963383));
#19359=CARTESIAN_POINT('Ctrl Pts',(-1.88596913666793,-1.,0.432493038548748));
#19360=CARTESIAN_POINT('Ctrl Pts',(-1.88044229001832,-1.,0.429803062482344));
#19361=CARTESIAN_POINT('Ctrl Pts',(-1.87486989291484,-1.,0.427183828519102));
#19362=CARTESIAN_POINT('Ctrl Pts',(-1.86937803944323,-1.,0.424678177291359));
#19363=CARTESIAN_POINT('Ctrl Pts',(-1.86408083334028,-1.,0.422327307418275));
#19364=CARTESIAN_POINT('Ctrl Pts',(-1.85903281096686,-1.,0.420157287975619));
#19365=CARTESIAN_POINT('Ctrl Pts',(-1.85417632856234,-1.,0.418164129143534));
#19366=CARTESIAN_POINT('Ctrl Pts',(-1.84929312929882,-1.,0.416300022038864));
#19367=CARTESIAN_POINT('Ctrl Pts',(-1.8440575707371,-1.,0.41448743825434));
#19368=CARTESIAN_POINT('Ctrl Pts',(-1.83808953475839,-1.,0.412633125322161));
#19369=CARTESIAN_POINT('Ctrl Pts',(-1.83100408895216,-1.,0.410641256301675));
#19370=CARTESIAN_POINT('Ctrl Pts',(-1.8224702267854,-1.,0.408428948108533));
#19371=CARTESIAN_POINT('Ctrl Pts',(-1.81223801813988,-1.,0.405933518411838));
#19372=CARTESIAN_POINT('Ctrl Pts',(-1.80012077176221,-1.,0.403107976170441));
#19373=CARTESIAN_POINT('Ctrl Pts',(-1.78598826347533,-1.,0.39991940378308));
#19374=CARTESIAN_POINT('Ctrl Pts',(-1.7697556004756,-1.,0.39634619612042));
#19375=CARTESIAN_POINT('Ctrl Pts',(-1.75137405313962,-1.,0.392375812294307));
#19376=CARTESIAN_POINT('Ctrl Pts',(-1.7349317097561,-1.,0.388877023509191));
#19377=CARTESIAN_POINT('Ctrl Pts',(-1.72162022246158,-1.,0.38607079032701));
#19378=CARTESIAN_POINT('Ctrl Pts',(-1.71231062891958,-1.,0.384119047315542));
#19379=CARTESIAN_POINT('Ctrl Pts',(-1.7075470150345,-1.,0.383122945602004));
#19380=CARTESIAN_POINT('',(-1.74236521665491,-1.,0.163289472382896));
#19381=CARTESIAN_POINT('Origin',(0.,-1.,0.));
#19382=CARTESIAN_POINT('',(-2.19890268624765,-1.,0.069476445021958));
#19383=CARTESIAN_POINT('Ctrl Pts',(-1.74236521665491,-1.,0.163289472382896));
#19384=CARTESIAN_POINT('Ctrl Pts',(-1.7472034950333,-1.,0.163814161002002));
#19385=CARTESIAN_POINT('Ctrl Pts',(-1.75666056638427,-1.,0.164834765707158));
#19386=CARTESIAN_POINT('Ctrl Pts',(-1.77018771684844,-1.,0.1662793551464));
#19387=CARTESIAN_POINT('Ctrl Pts',(-1.7869064998507,-1.,0.168032772805197));
#19388=CARTESIAN_POINT('Ctrl Pts',(-1.80561530629706,-1.,0.169936923904608));
#19389=CARTESIAN_POINT('Ctrl Pts',(-1.82215766811545,-1.,0.171554770204119));
#19390=CARTESIAN_POINT('Ctrl Pts',(-1.83658380527692,-1.,0.1728894428919));
#19391=CARTESIAN_POINT('Ctrl Pts',(-1.8489811319852,-1.,0.173946627587731));
#19392=CARTESIAN_POINT('Ctrl Pts',(-1.85948367088837,-1.,0.17473525927603));
#19393=CARTESIAN_POINT('Ctrl Pts',(-1.86828349694799,-1.,0.175268337590758));
#19394=CARTESIAN_POINT('Ctrl Pts',(-1.87563767773588,-1.,0.175563480746485));
#19395=CARTESIAN_POINT('Ctrl Pts',(-1.88188663145367,-1.,0.175644148889698));
#19396=CARTESIAN_POINT('Ctrl Pts',(-1.88742606273259,-1.,0.175538155840648));
#19397=CARTESIAN_POINT('Ctrl Pts',(-1.892646301985,-1.,0.175274276190844));
#19398=CARTESIAN_POINT('Ctrl Pts',(-1.89788101117132,-1.,0.174879405091263));
#19399=CARTESIAN_POINT('Ctrl Pts',(-1.90335253862834,-1.,0.174375518661085));
#19400=CARTESIAN_POINT('Ctrl Pts',(-1.90911693975267,-1.,0.173776635257817));
#19401=CARTESIAN_POINT('Ctrl Pts',(-1.91511429159527,-1.,0.173090695383496));
#19402=CARTESIAN_POINT('Ctrl Pts',(-1.9212233439798,-1.,0.172321621259514));
#19403=CARTESIAN_POINT('Ctrl Pts',(-1.92731093582036,-1.,0.171471191532988));
#19404=CARTESIAN_POINT('Ctrl Pts',(-1.93329183155539,-1.,0.170541253116201));
#19405=CARTESIAN_POINT('Ctrl Pts',(-1.93915639211581,-1.,0.169534904817491));
#19406=CARTESIAN_POINT('Ctrl Pts',(-1.94493757756931,-1.,0.168455741607556));
#19407=CARTESIAN_POINT('Ctrl Pts',(-1.95069027794294,-1.,0.167307501784475));
#19408=CARTESIAN_POINT('Ctrl Pts',(-1.9564675971873,-1.,0.166093592002812));
#19409=CARTESIAN_POINT('Ctrl Pts',(-1.96229379940136,-1.,0.164816568920269));
#19410=CARTESIAN_POINT('Ctrl Pts',(-1.96816512677967,-1.,0.163478185457734));
#19411=CARTESIAN_POINT('Ctrl Pts',(-1.97406280235188,-1.,0.162079693556288));
#19412=CARTESIAN_POINT('Ctrl Pts',(-1.97996195437559,-1.,0.160622060784611));
#19413=CARTESIAN_POINT('Ctrl Pts',(-1.98584238283292,-1.,0.159106226437299));
#19414=CARTESIAN_POINT('Ctrl Pts',(-1.99169810931908,-1.,0.157533331459227));
#19415=CARTESIAN_POINT('Ctrl Pts',(-1.99753284771497,-1.,0.155904629548783));
#19416=CARTESIAN_POINT('Ctrl Pts',(-2.00335565310543,-1.,0.154221403049722));
#19417=CARTESIAN_POINT('Ctrl Pts',(-2.00917680318424,-1.,0.15248488362145));
#19418=CARTESIAN_POINT('Ctrl Pts',(-2.01500291940238,-1.,0.150696157673078));
#19419=CARTESIAN_POINT('Ctrl Pts',(-2.02083464969894,-1.,0.148856124775337));
#19420=CARTESIAN_POINT('Ctrl Pts',(-2.02666926182017,-1.,0.146965557332583));
#19421=CARTESIAN_POINT('Ctrl Pts',(-2.03250223739942,-1.,0.145025140186057));
#19422=CARTESIAN_POINT('Ctrl Pts',(-2.03832911025912,-1.,0.143035515058209));
#19423=CARTESIAN_POINT('Ctrl Pts',(-2.04414757947916,-1.,0.140997332152546));
#19424=CARTESIAN_POINT('Ctrl Pts',(-2.04995762001328,-1.,0.138911255368966));
#19425=CARTESIAN_POINT('Ctrl Pts',(-2.05576044414264,-1.,0.136777941218043));
#19426=CARTESIAN_POINT('Ctrl Pts',(-2.06155781517842,-1.,0.134598026192106));
#19427=CARTESIAN_POINT('Ctrl Pts',(-2.06735123910326,-1.,0.13237211154771));
#19428=CARTESIAN_POINT('Ctrl Pts',(-2.07314114713063,-1.,0.130100748328403));
#19429=CARTESIAN_POINT('Ctrl Pts',(-2.07892715110987,-1.,0.12778444527612));
#19430=CARTESIAN_POINT('Ctrl Pts',(-2.08470840653643,-1.,0.125423679412061));
#19431=CARTESIAN_POINT('Ctrl Pts',(-2.09048392424825,-1.,0.123018905621083));
#19432=CARTESIAN_POINT('Ctrl Pts',(-2.0962529286773,-1.,0.120570567965122));
#19433=CARTESIAN_POINT('Ctrl Pts',(-2.102015121329,-1.,0.118079107988355));
#19434=CARTESIAN_POINT('Ctrl Pts',(-2.10777050261309,-1.,0.115544957687926));
#19435=CARTESIAN_POINT('Ctrl Pts',(-2.11351924490306,-1.,0.112968534419737));
#19436=CARTESIAN_POINT('Ctrl Pts',(-2.11926155590865,-1.,0.110350236135025));
#19437=CARTESIAN_POINT('Ctrl Pts',(-2.12499752307,-1.,0.10769043523109));
#19438=CARTESIAN_POINT('Ctrl Pts',(-2.13072704887293,-1.,0.104989479152739));
#19439=CARTESIAN_POINT('Ctrl Pts',(-2.13644992667165,-1.,0.1022477005561));
#19440=CARTESIAN_POINT('Ctrl Pts',(-2.14216588396025,-1.,0.0994654261990914));
#19441=CARTESIAN_POINT('Ctrl Pts',(-2.14787463531795,-1.,0.0966429852305457));
#19442=CARTESIAN_POINT('Ctrl Pts',(-2.1535759397817,-1.,0.0937807218867642));
#19443=CARTESIAN_POINT('Ctrl Pts',(-2.15926961544516,-1.,0.0908789888107264));
#19444=CARTESIAN_POINT('Ctrl Pts',(-2.16495552645014,-1.,0.0879381291386921));
#19445=CARTESIAN_POINT('Ctrl Pts',(-2.17063357870952,-1.,0.0849584620835371));
#19446=CARTESIAN_POINT('Ctrl Pts',(-2.176303712113,-1.,0.0819402680872764));
#19447=CARTESIAN_POINT('Ctrl Pts',(-2.18196589448887,-1.,0.0788837727685241));
#19448=CARTESIAN_POINT('Ctrl Pts',(-2.1876201139953,-1.,0.0757891465836146));
#19449=CARTESIAN_POINT('Ctrl Pts',(-2.19213712013662,-1.,0.0732830357306724));
#19450=CARTESIAN_POINT('Ctrl Pts',(-2.19552129484002,-1.,0.0713863779526153));
#19451=CARTESIAN_POINT('Ctrl Pts',(-2.19777582085423,-1.,0.0701143536325489));
#19452=CARTESIAN_POINT('Ctrl Pts',(-2.19890268624765,-1.,0.069476445021958));
#19453=CARTESIAN_POINT('',(-2.19890268624765,-1.,-0.0694764450219585));
#19454=CARTESIAN_POINT('',(-2.19890268624765,-1.,0.069476445021958));
#19455=CARTESIAN_POINT('',(-1.74236521665491,-1.,-0.163289472382896));
#19456=CARTESIAN_POINT('Ctrl Pts',(-2.19890268624765,-1.,-0.0694764450219585));
#19457=CARTESIAN_POINT('Ctrl Pts',(-2.19777582085261,-1.,-0.0701143536324927));
#19458=CARTESIAN_POINT('Ctrl Pts',(-2.19552129483562,-1.,-0.0713863779524629));
#19459=CARTESIAN_POINT('Ctrl Pts',(-2.19213712012956,-1.,-0.0732830357304277));
#19460=CARTESIAN_POINT('Ctrl Pts',(-2.1876201139874,-1.,-0.0757891465833413));
#19461=CARTESIAN_POINT('Ctrl Pts',(-2.18196589448304,-1.,-0.0788837727683229));
#19462=CARTESIAN_POINT('Ctrl Pts',(-2.1763037121106,-1.,-0.0819402680871941));
#19463=CARTESIAN_POINT('Ctrl Pts',(-2.17063357871031,-1.,-0.0849584620835644));
#19464=CARTESIAN_POINT('Ctrl Pts',(-2.16495552645275,-1.,-0.0879381291387824));
#19465=CARTESIAN_POINT('Ctrl Pts',(-2.15926961544808,-1.,-0.0908789888108267));
#19466=CARTESIAN_POINT('Ctrl Pts',(-2.15357593978377,-1.,-0.0937807218868346));
#19467=CARTESIAN_POINT('Ctrl Pts',(-2.14787463531864,-1.,-0.096642985230569));
#19468=CARTESIAN_POINT('Ctrl Pts',(-2.14216588395974,-1.,-0.0994654261990744));
#19469=CARTESIAN_POINT('Ctrl Pts',(-2.13644992667052,-1.,-0.102247700556064));
#19470=CARTESIAN_POINT('Ctrl Pts',(-2.1307270488718,-1.,-0.104989479152703));
#19471=CARTESIAN_POINT('Ctrl Pts',(-2.12499752306927,-1.,-0.107690435231068));
#19472=CARTESIAN_POINT('Ctrl Pts',(-2.11926155590849,-1.,-0.11035023613502));
#19473=CARTESIAN_POINT('Ctrl Pts',(-2.11351924490335,-1.,-0.112968534419746));
#19474=CARTESIAN_POINT('Ctrl Pts',(-2.10777050261359,-1.,-0.11554495768794));
#19475=CARTESIAN_POINT('Ctrl Pts',(-2.10201512132945,-1.,-0.118079107988368));
#19476=CARTESIAN_POINT('Ctrl Pts',(-2.09625292867756,-1.,-0.120570567965129));
#19477=CARTESIAN_POINT('Ctrl Pts',(-2.09048392424826,-1.,-0.123018905621083));
#19478=CARTESIAN_POINT('Ctrl Pts',(-2.08470840653628,-1.,-0.125423679412058));
#19479=CARTESIAN_POINT('Ctrl Pts',(-2.07892715110967,-1.,-0.127784445276116));
#19480=CARTESIAN_POINT('Ctrl Pts',(-2.07314114713047,-1.,-0.130100748328401));
#19481=CARTESIAN_POINT('Ctrl Pts',(-2.06735123910319,-1.,-0.13237211154771));
#19482=CARTESIAN_POINT('Ctrl Pts',(-2.06155781517844,-1.,-0.134598026192107));
#19483=CARTESIAN_POINT('Ctrl Pts',(-2.0557604441427,-1.,-0.136777941218044));
#19484=CARTESIAN_POINT('Ctrl Pts',(-2.04995762001333,-1.,-0.138911255368966));
#19485=CARTESIAN_POINT('Ctrl Pts',(-2.04414757947919,-1.,-0.140997332152545));
#19486=CARTESIAN_POINT('Ctrl Pts',(-2.03832911025913,-1.,-0.143035515058208));
#19487=CARTESIAN_POINT('Ctrl Pts',(-2.03250223739941,-1.,-0.145025140186058));
#19488=CARTESIAN_POINT('Ctrl Pts',(-2.02666926182017,-1.,-0.146965557332586));
#19489=CARTESIAN_POINT('Ctrl Pts',(-2.02083464969897,-1.,-0.148856124775343));
#19490=CARTESIAN_POINT('Ctrl Pts',(-2.01500291940243,-1.,-0.150696157673084));
#19491=CARTESIAN_POINT('Ctrl Pts',(-2.00917680318426,-1.,-0.152484883621452));
#19492=CARTESIAN_POINT('Ctrl Pts',(-2.00335565310539,-1.,-0.154221403049719));
#19493=CARTESIAN_POINT('Ctrl Pts',(-1.99753284771487,-1.,-0.155904629548775));
#19494=CARTESIAN_POINT('Ctrl Pts',(-1.99169810931893,-1.,-0.157533331459215));
#19495=CARTESIAN_POINT('Ctrl Pts',(-1.98584238283279,-1.,-0.159106226437289));
#19496=CARTESIAN_POINT('Ctrl Pts',(-1.97996195437557,-1.,-0.16062206078461));
#19497=CARTESIAN_POINT('Ctrl Pts',(-1.97406280235204,-1.,-0.162079693556302));
#19498=CARTESIAN_POINT('Ctrl Pts',(-1.96816512678,-1.,-0.16347818545776));
#19499=CARTESIAN_POINT('Ctrl Pts',(-1.96229379940174,-1.,-0.1648165689203));
#19500=CARTESIAN_POINT('Ctrl Pts',(-1.95646759718755,-1.,-0.166093592002833));
#19501=CARTESIAN_POINT('Ctrl Pts',(-1.95069027794286,-1.,-0.167307501784469));
#19502=CARTESIAN_POINT('Ctrl Pts',(-1.94493757756879,-1.,-0.168455741607516));
#19503=CARTESIAN_POINT('Ctrl Pts',(-1.93915639211497,-1.,-0.169534904817425));
#19504=CARTESIAN_POINT('Ctrl Pts',(-1.93329183155455,-1.,-0.170541253116136));
#19505=CARTESIAN_POINT('Ctrl Pts',(-1.92731093582,-1.,-0.17147119153296));
#19506=CARTESIAN_POINT('Ctrl Pts',(-1.92122334398034,-1.,-0.172321621259557));
#19507=CARTESIAN_POINT('Ctrl Pts',(-1.91511429159681,-1.,-0.173090695383619));
#19508=CARTESIAN_POINT('Ctrl Pts',(-1.90911693975475,-1.,-0.173776635257984));
#19509=CARTESIAN_POINT('Ctrl Pts',(-1.90335253863003,-1.,-0.174375518661222));
#19510=CARTESIAN_POINT('Ctrl Pts',(-1.89788101117148,-1.,-0.174879405091277));
#19511=CARTESIAN_POINT('Ctrl Pts',(-1.89264630198279,-1.,-0.175274276190664));
#19512=CARTESIAN_POINT('Ctrl Pts',(-1.88742606272818,-1.,-0.175538155840286));
#19513=CARTESIAN_POINT('Ctrl Pts',(-1.88188663144846,-1.,-0.175644148889271));
#19514=CARTESIAN_POINT('Ctrl Pts',(-1.87563767773249,-1.,-0.175563480746205));
#19515=CARTESIAN_POINT('Ctrl Pts',(-1.86828349694972,-1.,-0.175268337590901));
#19516=CARTESIAN_POINT('Ctrl Pts',(-1.85948367089838,-1.,-0.174735259276856));
#19517=CARTESIAN_POINT('Ctrl Pts',(-1.84898113200543,-1.,-0.173946627589401));
#19518=CARTESIAN_POINT('Ctrl Pts',(-1.83658380530747,-1.,-0.17288944289442));
#19519=CARTESIAN_POINT('Ctrl Pts',(-1.82215766815414,-1.,-0.171554770207306));
#19520=CARTESIAN_POINT('Ctrl Pts',(-1.80561530633924,-1.,-0.169936923908078));
#19521=CARTESIAN_POINT('Ctrl Pts',(-1.78690649988931,-1.,-0.16803277280837));
#19522=CARTESIAN_POINT('Ctrl Pts',(-1.77018771687692,-1.,-0.166279355148738));
#19523=CARTESIAN_POINT('Ctrl Pts',(-1.75666056640041,-1.,-0.164834765708484));
#19524=CARTESIAN_POINT('Ctrl Pts',(-1.74720349503904,-1.,-0.163814161002474));
#19525=CARTESIAN_POINT('Ctrl Pts',(-1.74236521665491,-1.,-0.163289472382896));
#19526=CARTESIAN_POINT('',(-1.7075470150345,-1.,-0.383122945602004));
#19527=CARTESIAN_POINT('Origin',(0.,-1.,0.));
#19528=CARTESIAN_POINT('',(-2.11275013067528,-1.,-0.61342227326009));
#19529=CARTESIAN_POINT('Ctrl Pts',(-1.7075470150345,-1.,-0.383122945602004));
#19530=CARTESIAN_POINT('Ctrl Pts',(-1.71231062891398,-1.,-0.384119047314215));
#19531=CARTESIAN_POINT('Ctrl Pts',(-1.72162022244582,-1.,-0.386070790323281));
#19532=CARTESIAN_POINT('Ctrl Pts',(-1.73493170972829,-1.,-0.388877023502615));
#19533=CARTESIAN_POINT('Ctrl Pts',(-1.75137405310193,-1.,-0.392375812285395));
#19534=CARTESIAN_POINT('Ctrl Pts',(-1.76975560043442,-1.,-0.396346196110688));
#19535=CARTESIAN_POINT('Ctrl Pts',(-1.78598826343754,-1.,-0.399919403774155));
#19536=CARTESIAN_POINT('Ctrl Pts',(-1.80012077173238,-1.,-0.403107976163396));
#19537=CARTESIAN_POINT('Ctrl Pts',(-1.81223801812013,-1.,-0.405933518407175));
#19538=CARTESIAN_POINT('Ctrl Pts',(-1.82247022677562,-1.,-0.408428948106227));
#19539=CARTESIAN_POINT('Ctrl Pts',(-1.83100408895047,-1.,-0.410641256301276));
#19540=CARTESIAN_POINT('Ctrl Pts',(-1.8380895347617,-1.,-0.412633125322945));
#19541=CARTESIAN_POINT('Ctrl Pts',(-1.84405757074218,-1.,-0.414487438255542));
#19542=CARTESIAN_POINT('Ctrl Pts',(-1.84929312930314,-1.,-0.416300022039885));
#19543=CARTESIAN_POINT('Ctrl Pts',(-1.8541763285645,-1.,-0.418164129144045));
#19544=CARTESIAN_POINT('Ctrl Pts',(-1.8590328109667,-1.,-0.420157287975583));
#19545=CARTESIAN_POINT('Ctrl Pts',(-1.86408083333863,-1.,-0.422327307417884));
#19546=CARTESIAN_POINT('Ctrl Pts',(-1.8693780394412,-1.,-0.424678177290876));
#19547=CARTESIAN_POINT('Ctrl Pts',(-1.87486989291333,-1.,-0.427183828518743));
#19548=CARTESIAN_POINT('Ctrl Pts',(-1.88044229001778,-1.,-0.429803062482217));
#19549=CARTESIAN_POINT('Ctrl Pts',(-1.88596913666828,-1.,-0.432493038548833));
#19550=CARTESIAN_POINT('Ctrl Pts',(-1.89136993975585,-1.,-0.43522566096358));
#19551=CARTESIAN_POINT('Ctrl Pts',(-1.89663648956549,-1.,-0.437995003948443));
#19552=CARTESIAN_POINT('Ctrl Pts',(-1.90180124389137,-1.,-0.44080783370416));
#19553=CARTESIAN_POINT('Ctrl Pts',(-1.90691756144906,-1.,-0.44367755684917));
#19554=CARTESIAN_POINT('Ctrl Pts',(-1.91203699981095,-1.,-0.446617343485651));
#19555=CARTESIAN_POINT('Ctrl Pts',(-1.91718342555717,-1.,-0.449632260106572));
#19556=CARTESIAN_POINT('Ctrl Pts',(-1.9223538064847,-1.,-0.452719478359356));
#19557=CARTESIAN_POINT('Ctrl Pts',(-1.92753067150461,-1.,-0.455872005174335));
#19558=CARTESIAN_POINT('Ctrl Pts',(-1.93269066517936,-1.,-0.459081234547931));
#19559=CARTESIAN_POINT('Ctrl Pts',(-1.93781486640834,-1.,-0.462340031009087));
#19560=CARTESIAN_POINT('Ctrl Pts',(-1.94289794196205,-1.,-0.465645462026064));
#19561=CARTESIAN_POINT('Ctrl Pts',(-1.94794381136524,-1.,-0.468997482913158));
#19562=CARTESIAN_POINT('Ctrl Pts',(-1.95296148278136,-1.,-0.472397672264079));
#19563=CARTESIAN_POINT('Ctrl Pts',(-1.95796111148175,-1.,-0.475848034683171));
#19564=CARTESIAN_POINT('Ctrl Pts',(-1.96294933055938,-1.,-0.479349583074846));
#19565=CARTESIAN_POINT('Ctrl Pts',(-1.96792703422358,-1.,-0.482901662120686));
#19566=CARTESIAN_POINT('Ctrl Pts',(-1.97289186263272,-1.,-0.486502692907661));
#19567=CARTESIAN_POINT('Ctrl Pts',(-1.97783973019229,-1.,-0.490150627860955));
#19568=CARTESIAN_POINT('Ctrl Pts',(-1.9827665876182,-1.,-0.493843476541492));
#19569=CARTESIAN_POINT('Ctrl Pts',(-1.98767044752929,-1.,-0.497579909545564));
#19570=CARTESIAN_POINT('Ctrl Pts',(-1.9925514912615,-1.,-0.501359287727129));
#19571=CARTESIAN_POINT('Ctrl Pts',(-1.99741107463567,-1.,-0.505181361323011));
#19572=CARTESIAN_POINT('Ctrl Pts',(-2.00225107134733,-1.,-0.509046069886152));
#19573=CARTESIAN_POINT('Ctrl Pts',(-2.00707309946955,-1.,-0.512953306961813));
#19574=CARTESIAN_POINT('Ctrl Pts',(-2.01187773939257,-1.,-0.516902681728733));
#19575=CARTESIAN_POINT('Ctrl Pts',(-2.01666477917305,-1.,-0.520893590399428));
#19576=CARTESIAN_POINT('Ctrl Pts',(-2.02143356304712,-1.,-0.524925318333518));
#19577=CARTESIAN_POINT('Ctrl Pts',(-2.02618329083289,-1.,-0.52899712724191));
#19578=CARTESIAN_POINT('Ctrl Pts',(-2.03091336214401,-1.,-0.533108355132905));
#19579=CARTESIAN_POINT('Ctrl Pts',(-2.03562362953993,-1.,-0.537258489833134));
#19580=CARTESIAN_POINT('Ctrl Pts',(-2.0403142269048,-1.,-0.54144712061552));
#19581=CARTESIAN_POINT('Ctrl Pts',(-2.0449854471456,-1.,-0.545673903817348));
#19582=CARTESIAN_POINT('Ctrl Pts',(-2.04963761077974,-1.,-0.549938525150342));
#19583=CARTESIAN_POINT('Ctrl Pts',(-2.05427091604482,-1.,-0.554240657464109));
#19584=CARTESIAN_POINT('Ctrl Pts',(-2.05888537756571,-1.,-0.558579940185467));
#19585=CARTESIAN_POINT('Ctrl Pts',(-2.06348090160697,-1.,-0.562955993082574));
#19586=CARTESIAN_POINT('Ctrl Pts',(-2.06805732997383,-1.,-0.567368421181229));
#19587=CARTESIAN_POINT('Ctrl Pts',(-2.07261449292757,-1.,-0.571816823242411));
#19588=CARTESIAN_POINT('Ctrl Pts',(-2.07715226767361,-1.,-0.576300797416274));
#19589=CARTESIAN_POINT('Ctrl Pts',(-2.08167059018138,-1.,-0.580819952107257));
#19590=CARTESIAN_POINT('Ctrl Pts',(-2.086169437277,-1.,-0.585373918990895));
#19591=CARTESIAN_POINT('Ctrl Pts',(-2.09064881812053,-1.,-0.589962365403189));
#19592=CARTESIAN_POINT('Ctrl Pts',(-2.09510876220501,-1.,-0.594585006052823));
#19593=CARTESIAN_POINT('Ctrl Pts',(-2.09954930865331,-1.,-0.599241616422144));
#19594=CARTESIAN_POINT('Ctrl Pts',(-2.10397049887709,-1.,-0.603932030738212));
#19595=CARTESIAN_POINT('Ctrl Pts',(-2.10749199615859,-1.,-0.607711315456826));
#19596=CARTESIAN_POINT('Ctrl Pts',(-2.11012443807661,-1.,-0.610560911691113));
#19597=CARTESIAN_POINT('Ctrl Pts',(-2.11187554260142,-1.,-0.61246736556225));
#19598=CARTESIAN_POINT('Ctrl Pts',(-2.11275013067528,-1.,-0.61342227326009));
#19599=CARTESIAN_POINT('',(-2.0698113262342,-1.,-0.745574324794401));
#19600=CARTESIAN_POINT('',(-2.11275013067528,-1.,-0.61342227326009));
#19601=CARTESIAN_POINT('',(-1.60662857109684,-1.,-0.693717979106306));
#19602=CARTESIAN_POINT('Ctrl Pts',(-2.0698113262342,-1.,-0.745574324794401));
#19603=CARTESIAN_POINT('Ctrl Pts',(-2.06854248895575,-1.,-0.74583279137781));
#19604=CARTESIAN_POINT('Ctrl Pts',(-2.06600523016401,-1.,-0.746345871542695));
#19605=CARTESIAN_POINT('Ctrl Pts',(-2.06220058927162,-1.,-0.747103932785504));
#19606=CARTESIAN_POINT('Ctrl Pts',(-2.05713023030263,-1.,-0.748091554181101));
#19607=CARTESIAN_POINT('Ctrl Pts',(-2.05079645591606,-1.,-0.749287468663053));
#19608=CARTESIAN_POINT('Ctrl Pts',(-2.04446689147754,-1.,-0.750444657874758));
#19609=CARTESIAN_POINT('Ctrl Pts',(-2.03814160092173,-1.,-0.751562963361383));
#19610=CARTESIAN_POINT('Ctrl Pts',(-2.03182068456467,-1.,-0.752642180488104));
#19611=CARTESIAN_POINT('Ctrl Pts',(-2.02550428623587,-1.,-0.753682061113765));
#19612=CARTESIAN_POINT('Ctrl Pts',(-2.01919259406003,-1.,-0.75468233072352));
#19613=CARTESIAN_POINT('Ctrl Pts',(-2.01288584328149,-1.,-0.7556427049581));
#19614=CARTESIAN_POINT('Ctrl Pts',(-2.00658431587682,-1.,-0.756562904646496));
#19615=CARTESIAN_POINT('Ctrl Pts',(-2.00028834739072,-1.,-0.757442676862341));
#19616=CARTESIAN_POINT('Ctrl Pts',(-1.9939983109871,-1.,-0.758281796766377));
#19617=CARTESIAN_POINT('Ctrl Pts',(-1.98771456680806,-1.,-0.759080037802242));
#19618=CARTESIAN_POINT('Ctrl Pts',(-1.98143741418156,-1.,-0.759837147452135));
#19619=CARTESIAN_POINT('Ctrl Pts',(-1.97516705321521,-1.,-0.760552825409855));
#19620=CARTESIAN_POINT('Ctrl Pts',(-1.96890351582545,-1.,-0.761226690483986));
#19621=CARTESIAN_POINT('Ctrl Pts',(-1.96264672744229,-1.,-0.761858300014575));
#19622=CARTESIAN_POINT('Ctrl Pts',(-1.95639665309893,-1.,-0.762447203806263));
#19623=CARTESIAN_POINT('Ctrl Pts',(-1.95015342590025,-1.,-0.762992990878774));
#19624=CARTESIAN_POINT('Ctrl Pts',(-1.94391746617626,-1.,-0.76349533353858));
#19625=CARTESIAN_POINT('Ctrl Pts',(-1.93768964875867,-1.,-0.763954049121393));
#19626=CARTESIAN_POINT('Ctrl Pts',(-1.93147105496367,-1.,-0.764369010673889));
#19627=CARTESIAN_POINT('Ctrl Pts',(-1.92526263537041,-1.,-0.764740025488189));
#19628=CARTESIAN_POINT('Ctrl Pts',(-1.91906491634197,-1.,-0.765066729667095));
#19629=CARTESIAN_POINT('Ctrl Pts',(-1.91287765805174,-1.,-0.765348465884739));
#19630=CARTESIAN_POINT('Ctrl Pts',(-1.90669961402362,-1.,-0.765584196937936));
#19631=CARTESIAN_POINT('Ctrl Pts',(-1.90052930393599,-1.,-0.765772772593395));
#19632=CARTESIAN_POINT('Ctrl Pts',(-1.89436577771389,-1.,-0.765913193856979));
#19633=CARTESIAN_POINT('Ctrl Pts',(-1.88820926433409,-1.,-0.76600483706209));
#19634=CARTESIAN_POINT('Ctrl Pts',(-1.88206215302561,-1.,-0.766047794851868));
#19635=CARTESIAN_POINT('Ctrl Pts',(-1.87592888967886,-1.,-0.766042837036759));
#19636=CARTESIAN_POINT('Ctrl Pts',(-1.86981398314345,-1.,-0.765990708546111));
#19637=CARTESIAN_POINT('Ctrl Pts',(-1.86372027063314,-1.,-0.765891519092557));
#19638=CARTESIAN_POINT('Ctrl Pts',(-1.85764741390391,-1.,-0.765744212909305));
#19639=CARTESIAN_POINT('Ctrl Pts',(-1.85158945130054,-1.,-0.765545710619023));
#19640=CARTESIAN_POINT('Ctrl Pts',(-1.8455369887591,-1.,-0.765291664861971));
#19641=CARTESIAN_POINT('Ctrl Pts',(-1.83948181064823,-1.,-0.764978057881687));
#19642=CARTESIAN_POINT('Ctrl Pts',(-1.8334207722714,-1.,-0.764602549687845));
#19643=CARTESIAN_POINT('Ctrl Pts',(-1.8273599120008,-1.,-0.764165902606055));
#19644=CARTESIAN_POINT('Ctrl Pts',(-1.82131873145297,-1.,-0.763673465462854));
#19645=CARTESIAN_POINT('Ctrl Pts',(-1.81532118405566,-1.,-0.763132003836783));
#19646=CARTESIAN_POINT('Ctrl Pts',(-1.80938551463989,-1.,-0.762546129464036));
#19647=CARTESIAN_POINT('Ctrl Pts',(-1.80351583877334,-1.,-0.761915336443515));
#19648=CARTESIAN_POINT('Ctrl Pts',(-1.79768986997735,-1.,-0.761229695230359));
#19649=CARTESIAN_POINT('Ctrl Pts',(-1.79185815610802,-1.,-0.760469555880425));
#19650=CARTESIAN_POINT('Ctrl Pts',(-1.78596964884526,-1.,-0.759614401109868));
#19651=CARTESIAN_POINT('Ctrl Pts',(-1.77999411220912,-1.,-0.75865062667738));
#19652=CARTESIAN_POINT('Ctrl Pts',(-1.77394167108342,-1.,-0.757578264077238));
#19653=CARTESIAN_POINT('Ctrl Pts',(-1.76789396003141,-1.,-0.756421896028403));
#19654=CARTESIAN_POINT('Ctrl Pts',(-1.7619781724032,-1.,-0.755220979975262));
#19655=CARTESIAN_POINT('Ctrl Pts',(-1.75631083600175,-1.,-0.75400925402848));
#19656=CARTESIAN_POINT('Ctrl Pts',(-1.75095139468809,-1.,-0.752797683531377));
#19657=CARTESIAN_POINT('Ctrl Pts',(-1.74585086852298,-1.,-0.751555614163629));
#19658=CARTESIAN_POINT('Ctrl Pts',(-1.74080458266705,-1.,-0.75019343597954));
#19659=CARTESIAN_POINT('Ctrl Pts',(-1.73550351679848,-1.,-0.748582462954854));
#19660=CARTESIAN_POINT('Ctrl Pts',(-1.72958533647399,-1.,-0.746574710096436));
#19661=CARTESIAN_POINT('Ctrl Pts',(-1.7226822991693,-1.,-0.744021445433764));
#19662=CARTESIAN_POINT('Ctrl Pts',(-1.71447789751927,-1.,-0.740795162032087));
#19663=CARTESIAN_POINT('Ctrl Pts',(-1.70473309006121,-1.,-0.736799665724771));
#19664=CARTESIAN_POINT('Ctrl Pts',(-1.69326921975743,-1.,-0.731963238697195));
#19665=CARTESIAN_POINT('Ctrl Pts',(-1.67996158455503,-1.,-0.726235967997433));
#19666=CARTESIAN_POINT('Ctrl Pts',(-1.6647288055568,-1.,-0.719585433804282));
#19667=CARTESIAN_POINT('Ctrl Pts',(-1.64752408832016,-1.,-0.711993139355394));
#19668=CARTESIAN_POINT('Ctrl Pts',(-1.63216541664676,-1.,-0.705159151988319));
#19669=CARTESIAN_POINT('Ctrl Pts',(-1.61974673472612,-1.,-0.699605146405088));
#19670=CARTESIAN_POINT('Ctrl Pts',(-1.61106790958151,-1.,-0.695712097881194));
#19671=CARTESIAN_POINT('Ctrl Pts',(-1.60662857109684,-1.,-0.693717979106306));
#19672=CARTESIAN_POINT('',(-1.5055822144029,-1.,-0.892032620296855));
#19673=CARTESIAN_POINT('Origin',(0.,-1.,0.));
#19674=CARTESIAN_POINT('',(-1.81978687191668,-1.,-1.23627494547115));
#19675=CARTESIAN_POINT('Ctrl Pts',(-1.5055822144029,-1.,-0.892032620296855));
#19676=CARTESIAN_POINT('Ctrl Pts',(-1.50980486806688,-1.,-0.894452006964543));
#19677=CARTESIAN_POINT('Ctrl Pts',(-1.51805569590094,-1.,-0.899185047483511));
#19678=CARTESIAN_POINT('Ctrl Pts',(-1.52984849887993,-1.,-0.905967409625651));
#19679=CARTESIAN_POINT('Ctrl Pts',(-1.54440491149498,-1.,-0.914375919026456));
#19680=CARTESIAN_POINT('Ctrl Pts',(-1.56065988578893,-1.,-0.923832188944341));
#19681=CARTESIAN_POINT('Ctrl Pts',(-1.57499388382243,-1.,-0.932246680108685));
#19682=CARTESIAN_POINT('Ctrl Pts',(-1.58744937487176,-1.,-0.939646377893399));
#19683=CARTESIAN_POINT('Ctrl Pts',(-1.59810042043673,-1.,-0.946078063315257));
#19684=CARTESIAN_POINT('Ctrl Pts',(-1.60706069896936,-1.,-0.951613284356035));
#19685=CARTESIAN_POINT('Ctrl Pts',(-1.61449324337085,-1.,-0.956354422920671));
#19686=CARTESIAN_POINT('Ctrl Pts',(-1.62061638140221,-1.,-0.960438326101729));
#19687=CARTESIAN_POINT('Ctrl Pts',(-1.62571930670187,-1.,-0.964046107040536));
#19688=CARTESIAN_POINT('Ctrl Pts',(-1.63013849959461,-1.,-0.967387853230345));
#19689=CARTESIAN_POINT('Ctrl Pts',(-1.63420665729798,-1.,-0.970669715997509));
#19690=CARTESIAN_POINT('Ctrl Pts',(-1.63820952658144,-1.,-0.974066058287418));
#19691=CARTESIAN_POINT('Ctrl Pts',(-1.64233990826687,-1.,-0.977689794119416));
#19692=CARTESIAN_POINT('Ctrl Pts',(-1.64665139190656,-1.,-0.981562530939489));
#19693=CARTESIAN_POINT('Ctrl Pts',(-1.65110016612638,-1.,-0.985642622920821));
#19694=CARTESIAN_POINT('Ctrl Pts',(-1.65559044289699,-1.,-0.989855627854165));
#19695=CARTESIAN_POINT('Ctrl Pts',(-1.66001553809947,-1.,-0.994121836661306));
#19696=CARTESIAN_POINT('Ctrl Pts',(-1.66430758030376,-1.,-0.998389654952758));
#19697=CARTESIAN_POINT('Ctrl Pts',(-1.66846059277303,-1.,-1.00265091003727));
#19698=CARTESIAN_POINT('Ctrl Pts',(-1.67250335383293,-1.,-1.00692206696414));
#19699=CARTESIAN_POINT('Ctrl Pts',(-1.67648246776464,-1.,-1.01123236493511));
#19700=CARTESIAN_POINT('Ctrl Pts',(-1.68044289894798,-1.,-1.01561026162773));
#19701=CARTESIAN_POINT('Ctrl Pts',(-1.68440578021706,-1.,-1.02006795074201));
#19702=CARTESIAN_POINT('Ctrl Pts',(-1.68836910178447,-1.,-1.02460180535255));
#19703=CARTESIAN_POINT('Ctrl Pts',(-1.69231840863458,-1.,-1.02919977579147));
#19704=CARTESIAN_POINT('Ctrl Pts',(-1.69623414782771,-1.,-1.03384646003588));
#19705=CARTESIAN_POINT('Ctrl Pts',(-1.70010052930962,-1.,-1.03852922490789));
#19706=CARTESIAN_POINT('Ctrl Pts',(-1.70391338707982,-1.,-1.04324363334554));
#19707=CARTESIAN_POINT('Ctrl Pts',(-1.70767646263649,-1.,-1.04799085404995));
#19708=CARTESIAN_POINT('Ctrl Pts',(-1.71139783543989,-1.,-1.05277517202855));
#19709=CARTESIAN_POINT('Ctrl Pts',(-1.7150865442702,-1.,-1.05760163192479));
#19710=CARTESIAN_POINT('Ctrl Pts',(-1.71874858456904,-1.,-1.06247324680647));
#19711=CARTESIAN_POINT('Ctrl Pts',(-1.72238500928453,-1.,-1.06738966975462));
#19712=CARTESIAN_POINT('Ctrl Pts',(-1.72599406198488,-1.,-1.07234866990252));
#19713=CARTESIAN_POINT('Ctrl Pts',(-1.72957248977424,-1.,-1.0773470373727));
#19714=CARTESIAN_POINT('Ctrl Pts',(-1.73311705663407,-1.,-1.08238162784749));
#19715=CARTESIAN_POINT('Ctrl Pts',(-1.73662628326091,-1.,-1.08745056285427));
#19716=CARTESIAN_POINT('Ctrl Pts',(-1.74010053962247,-1.,-1.09255329056493));
#19717=CARTESIAN_POINT('Ctrl Pts',(-1.74354119236208,-1.,-1.09768999241225));
#19718=CARTESIAN_POINT('Ctrl Pts',(-1.74695004214923,-1.,-1.10286118991143));
#19719=CARTESIAN_POINT('Ctrl Pts',(-1.7503286607592,-1.,-1.10806728183007));
#19720=CARTESIAN_POINT('Ctrl Pts',(-1.7536777209463,-1.,-1.11330807582551));
#19721=CARTESIAN_POINT('Ctrl Pts',(-1.75699720772105,-1.,-1.11858293216763));
#19722=CARTESIAN_POINT('Ctrl Pts',(-1.76028671825096,-1.,-1.12389096855086));
#19723=CARTESIAN_POINT('Ctrl Pts',(-1.7635457196617,-1.,-1.12923123555075));
#19724=CARTESIAN_POINT('Ctrl Pts',(-1.76677384551862,-1.,-1.1346029180462));
#19725=CARTESIAN_POINT('Ctrl Pts',(-1.76997111386769,-1.,-1.14000548336975));
#19726=CARTESIAN_POINT('Ctrl Pts',(-1.77313777896194,-1.,-1.1454385822692));
#19727=CARTESIAN_POINT('Ctrl Pts',(-1.7762742255701,-1.,-1.15090197841515));
#19728=CARTESIAN_POINT('Ctrl Pts',(-1.77938085564275,-1.,-1.15639547194698));
#19729=CARTESIAN_POINT('Ctrl Pts',(-1.78245795881009,-1.,-1.16191881298499));
#19730=CARTESIAN_POINT('Ctrl Pts',(-1.78550566040443,-1.,-1.16747166312303));
#19731=CARTESIAN_POINT('Ctrl Pts',(-1.78852398877616,-1.,-1.17305363177328));
#19732=CARTESIAN_POINT('Ctrl Pts',(-1.79151291552689,-1.,-1.17866429440809));
#19733=CARTESIAN_POINT('Ctrl Pts',(-1.79447240321515,-1.,-1.18430321697432));
#19734=CARTESIAN_POINT('Ctrl Pts',(-1.79740245923478,-1.,-1.18996997934445));
#19735=CARTESIAN_POINT('Ctrl Pts',(-1.80030314369879,-1.,-1.19566418930242));
#19736=CARTESIAN_POINT('Ctrl Pts',(-1.80317454838603,-1.,-1.20138548938974));
#19737=CARTESIAN_POINT('Ctrl Pts',(-1.80601678480707,-1.,-1.20713356605475));
#19738=CARTESIAN_POINT('Ctrl Pts',(-1.80882996917129,-1.,-1.21290815708314));
#19739=CARTESIAN_POINT('Ctrl Pts',(-1.81161420806656,-1.,-1.21870906103557));
#19740=CARTESIAN_POINT('Ctrl Pts',(-1.81436959210434,-1.,-1.2245361330495));
#19741=CARTESIAN_POINT('Ctrl Pts',(-1.8165508718364,-1.,-1.2292186489137));
#19742=CARTESIAN_POINT('Ctrl Pts',(-1.81817389921279,-1.,-1.2327422452705));
#19743=CARTESIAN_POINT('Ctrl Pts',(-1.81925017193666,-1.,-1.23509651170476));
#19744=CARTESIAN_POINT('Ctrl Pts',(-1.81978687191668,-1.,-1.23627494547115));
#19745=CARTESIAN_POINT('',(-1.73811241238545,-1.,-1.34869019493419));
#19746=CARTESIAN_POINT('',(-1.81978687191668,-1.,-1.23627494547115));
#19747=CARTESIAN_POINT('',(-1.31362392696032,-1.,-1.15624053661742));
#19748=CARTESIAN_POINT('Ctrl Pts',(-1.73811241238545,-1.,-1.34869019493419));
#19749=CARTESIAN_POINT('Ctrl Pts',(-1.73682580585691,-1.,-1.34854391898045));
#19750=CARTESIAN_POINT('Ctrl Pts',(-1.73425417885907,-1.,-1.34824783112887));
#19751=CARTESIAN_POINT('Ctrl Pts',(-1.7304014965394,-1.,-1.34779309152035));
#19752=CARTESIAN_POINT('Ctrl Pts',(-1.72527410680674,-1.,-1.34716554819527));
#19753=CARTESIAN_POINT('Ctrl Pts',(-1.7188807715049,-1.,-1.34634568653227));
#19754=CARTESIAN_POINT('Ctrl Pts',(-1.71250340686822,-1.,-1.34549029589416));
#19755=CARTESIAN_POINT('Ctrl Pts',(-1.70614212266738,-1.,-1.34459924533831));
#19756=CARTESIAN_POINT('Ctrl Pts',(-1.69979707754427,-1.,-1.34367237124483));
#19757=CARTESIAN_POINT('Ctrl Pts',(-1.6934684849687,-1.,-1.34270948206319));
#19758=CARTESIAN_POINT('Ctrl Pts',(-1.68715660868764,-1.,-1.341710374848));
#19759=CARTESIAN_POINT('Ctrl Pts',(-1.68086176030362,-1.,-1.34067485185203));
#19760=CARTESIAN_POINT('Ctrl Pts',(-1.67458429426086,-1.,-1.3396027347034));
#19761=CARTESIAN_POINT('Ctrl Pts',(-1.66832460783989,-1.,-1.33849388654388));
#19762=CARTESIAN_POINT('Ctrl Pts',(-1.66208312541983,-1.,-1.33734820885262));
#19763=CARTESIAN_POINT('Ctrl Pts',(-1.65586025952593,-1.,-1.33616559745172));
#19764=CARTESIAN_POINT('Ctrl Pts',(-1.6496563728683,-1.,-1.33494590467993));
#19765=CARTESIAN_POINT('Ctrl Pts',(-1.6434717485603,-1.,-1.33368890676572));
#19766=CARTESIAN_POINT('Ctrl Pts',(-1.63730653475089,-1.,-1.33239425103724));
#19767=CARTESIAN_POINT('Ctrl Pts',(-1.63116079730923,-1.,-1.33106149345645));
#19768=CARTESIAN_POINT('Ctrl Pts',(-1.62503464209797,-1.,-1.3296901950568));
#19769=CARTESIAN_POINT('Ctrl Pts',(-1.61892832270724,-1.,-1.32828000610449));
#19770=CARTESIAN_POINT('Ctrl Pts',(-1.6128423401575,-1.,-1.32683074483356));
#19771=CARTESIAN_POINT('Ctrl Pts',(-1.60677758290954,-1.,-1.32534250785782));
#19772=CARTESIAN_POINT('Ctrl Pts',(-1.60073511858687,-1.,-1.32381550858256));
#19773=CARTESIAN_POINT('Ctrl Pts',(-1.59471591079403,-1.,-1.32224985747682));
#19774=CARTESIAN_POINT('Ctrl Pts',(-1.58872057258245,-1.,-1.32064537110892));
#19775=CARTESIAN_POINT('Ctrl Pts',(-1.58274907898834,-1.,-1.31900135021432));
#19776=CARTESIAN_POINT('Ctrl Pts',(-1.5768005650559,-1.,-1.31731642317187));
#19777=CARTESIAN_POINT('Ctrl Pts',(-1.57087397835723,-1.,-1.31558903860016));
#19778=CARTESIAN_POINT('Ctrl Pts',(-1.56496872402353,-1.,-1.31381795281002));
#19779=CARTESIAN_POINT('Ctrl Pts',(-1.55908521254821,-1.,-1.31200264341696));
#19780=CARTESIAN_POINT('Ctrl Pts',(-1.55322568759481,-1.,-1.31014393684222));
#19781=CARTESIAN_POINT('Ctrl Pts',(-1.54739413957185,-1.,-1.30824393907473));
#19782=CARTESIAN_POINT('Ctrl Pts',(-1.54159462645432,-1.,-1.30630475189556));
#19783=CARTESIAN_POINT('Ctrl Pts',(-1.53582981268977,-1.,-1.30432735639489));
#19784=CARTESIAN_POINT('Ctrl Pts',(-1.53009970283891,-1.,-1.30231064395568));
#19785=CARTESIAN_POINT('Ctrl Pts',(-1.52439957861062,-1.,-1.30024984366328));
#19786=CARTESIAN_POINT('Ctrl Pts',(-1.51872184912724,-1.,-1.29813791800747));
#19787=CARTESIAN_POINT('Ctrl Pts',(-1.51305994241402,-1.,-1.29596850710509));
#19788=CARTESIAN_POINT('Ctrl Pts',(-1.50741159078365,-1.,-1.29373841372842));
#19789=CARTESIAN_POINT('Ctrl Pts',(-1.50178230149776,-1.,-1.29145022885181));
#19790=CARTESIAN_POINT('Ctrl Pts',(-1.49618896881754,-1.,-1.28911506584254));
#19791=CARTESIAN_POINT('Ctrl Pts',(-1.4906522831278,-1.,-1.2867467611644));
#19792=CARTESIAN_POINT('Ctrl Pts',(-1.4851881711891,-1.,-1.28435533880201));
#19793=CARTESIAN_POINT('Ctrl Pts',(-1.47980070347095,-1.,-1.28194158939517));
#19794=CARTESIAN_POINT('Ctrl Pts',(-1.4744717526707,-1.,-1.2794891824849));
#19795=CARTESIAN_POINT('Ctrl Pts',(-1.46916035917133,-1.,-1.27696414831089));
#19796=CARTESIAN_POINT('Ctrl Pts',(-1.46382431332476,-1.,-1.27433119897822));
#19797=CARTESIAN_POINT('Ctrl Pts',(-1.45843906294697,-1.,-1.27156805265289));
#19798=CARTESIAN_POINT('Ctrl Pts',(-1.45301422764247,-1.,-1.2686778680489));
#19799=CARTESIAN_POINT('Ctrl Pts',(-1.44761985001662,-1.,-1.26570925118868));
#19800=CARTESIAN_POINT('Ctrl Pts',(-1.44236470511303,-1.,-1.26273903323859));
#19801=CARTESIAN_POINT('Ctrl Pts',(-1.43734919180848,-1.,-1.25983531012005));
#19802=CARTESIAN_POINT('Ctrl Pts',(-1.43262645609691,-1.,-1.25702687965755));
#19803=CARTESIAN_POINT('Ctrl Pts',(-1.42815938799387,-1.,-1.25426945222639));
#19804=CARTESIAN_POINT('Ctrl Pts',(-1.42378102115575,-1.,-1.2514145557001));
#19805=CARTESIAN_POINT('Ctrl Pts',(-1.41923722596025,-1.,-1.24824430986571));
#19806=CARTESIAN_POINT('Ctrl Pts',(-1.41422913175179,-1.,-1.24450600513056));
#19807=CARTESIAN_POINT('Ctrl Pts',(-1.40845295531283,-1.,-1.23994455029534));
#19808=CARTESIAN_POINT('Ctrl Pts',(-1.40164708206106,-1.,-1.23434087290423));
#19809=CARTESIAN_POINT('Ctrl Pts',(-1.39361389568796,-1.,-1.22752961899387));
#19810=CARTESIAN_POINT('Ctrl Pts',(-1.38420564527715,-1.,-1.21938737280852));
#19811=CARTESIAN_POINT('Ctrl Pts',(-1.37331915607905,-1.,-1.20982812925645));
#19812=CARTESIAN_POINT('Ctrl Pts',(-1.36088705043885,-1.,-1.1987959077932));
#19813=CARTESIAN_POINT('Ctrl Pts',(-1.34687054001093,-1.,-1.18625865667441));
#19814=CARTESIAN_POINT('Ctrl Pts',(-1.33437539347008,-1.,-1.17501305789857));
#19815=CARTESIAN_POINT('Ctrl Pts',(-1.32428080721772,-1.,-1.16589330093588));
#19816=CARTESIAN_POINT('Ctrl Pts',(-1.31722977216397,-1.,-1.15950888730809));
#19817=CARTESIAN_POINT('Ctrl Pts',(-1.31362392696032,-1.,-1.15624053661742));
#19818=CARTESIAN_POINT('',(-1.15624053661742,-1.,-1.31362392696033));
#19819=CARTESIAN_POINT('Origin',(0.,-1.,0.));
#19820=CARTESIAN_POINT('',(-1.34869019493419,-1.,-1.73811241238545));
#19821=CARTESIAN_POINT('Ctrl Pts',(-1.15624053661742,-1.,-1.31362392696033));
#19822=CARTESIAN_POINT('Ctrl Pts',(-1.15950888730433,-1.,-1.3172297721596));
#19823=CARTESIAN_POINT('Ctrl Pts',(-1.16589330092532,-1.,-1.32428080720544));
#19824=CARTESIAN_POINT('Ctrl Pts',(-1.17501305787994,-1.,-1.33437539344842));
#19825=CARTESIAN_POINT('Ctrl Pts',(-1.18625865664915,-1.,-1.34687053998157));
#19826=CARTESIAN_POINT('Ctrl Pts',(-1.1987959077656,-1.,-1.36088705040677));
#19827=CARTESIAN_POINT('Ctrl Pts',(-1.20982812923113,-1.,-1.37331915604962));
#19828=CARTESIAN_POINT('Ctrl Pts',(-1.21938737278853,-1.,-1.38420564525391));
#19829=CARTESIAN_POINT('Ctrl Pts',(-1.22752961898063,-1.,-1.39361389567257));
#19830=CARTESIAN_POINT('Ctrl Pts',(-1.23434087289768,-1.,-1.40164708205345));
#19831=CARTESIAN_POINT('Ctrl Pts',(-1.23994455029421,-1.,-1.40845295531151));
#19832=CARTESIAN_POINT('Ctrl Pts',(-1.24450600513278,-1.,-1.41422913175437));
#19833=CARTESIAN_POINT('Ctrl Pts',(-1.24824430986911,-1.,-1.41923722596421));
#19834=CARTESIAN_POINT('Ctrl Pts',(-1.25141455570299,-1.,-1.42378102115911));
#19835=CARTESIAN_POINT('Ctrl Pts',(-1.25426945222783,-1.,-1.42815938799555));
#19836=CARTESIAN_POINT('Ctrl Pts',(-1.25702687965744,-1.,-1.43262645609679));
#19837=CARTESIAN_POINT('Ctrl Pts',(-1.25983531011894,-1.,-1.43734919180719));
#19838=CARTESIAN_POINT('Ctrl Pts',(-1.26273903323723,-1.,-1.44236470511145));
#19839=CARTESIAN_POINT('Ctrl Pts',(-1.26570925118767,-1.,-1.44761985001544));
#19840=CARTESIAN_POINT('Ctrl Pts',(-1.26867786804854,-1.,-1.45301422764205));
#19841=CARTESIAN_POINT('Ctrl Pts',(-1.27156805265312,-1.,-1.45843906294725));
#19842=CARTESIAN_POINT('Ctrl Pts',(-1.27433119897877,-1.,-1.4638243133254));
#19843=CARTESIAN_POINT('Ctrl Pts',(-1.27696414831144,-1.,-1.46916035917197));
#19844=CARTESIAN_POINT('Ctrl Pts',(-1.27948918248524,-1.,-1.4744717526711));
#19845=CARTESIAN_POINT('Ctrl Pts',(-1.28194158939522,-1.,-1.47980070347102));
#19846=CARTESIAN_POINT('Ctrl Pts',(-1.28435533880184,-1.,-1.48518817118891));
#19847=CARTESIAN_POINT('Ctrl Pts',(-1.28674676116415,-1.,-1.4906522831275));
#19848=CARTESIAN_POINT('Ctrl Pts',(-1.28911506584232,-1.,-1.49618896881729));
#19849=CARTESIAN_POINT('Ctrl Pts',(-1.29145022885171,-1.,-1.50178230149764));
#19850=CARTESIAN_POINT('Ctrl Pts',(-1.29373841372843,-1.,-1.50741159078367));
#19851=CARTESIAN_POINT('Ctrl Pts',(-1.29596850710518,-1.,-1.51305994241412));
#19852=CARTESIAN_POINT('Ctrl Pts',(-1.29813791800757,-1.,-1.51872184912735));
#19853=CARTESIAN_POINT('Ctrl Pts',(-1.30024984366334,-1.,-1.5243995786107));
#19854=CARTESIAN_POINT('Ctrl Pts',(-1.3023106439557,-1.,-1.53009970283893));
#19855=CARTESIAN_POINT('Ctrl Pts',(-1.30432735639487,-1.,-1.53582981268976));
#19856=CARTESIAN_POINT('Ctrl Pts',(-1.30630475189553,-1.,-1.54159462645428));
#19857=CARTESIAN_POINT('Ctrl Pts',(-1.30824393907471,-1.,-1.54739413957183));
#19858=CARTESIAN_POINT('Ctrl Pts',(-1.31014393684221,-1.,-1.55322568759481));
#19859=CARTESIAN_POINT('Ctrl Pts',(-1.31200264341696,-1.,-1.55908521254822));
#19860=CARTESIAN_POINT('Ctrl Pts',(-1.31381795281002,-1.,-1.56496872402352));
#19861=CARTESIAN_POINT('Ctrl Pts',(-1.31558903860015,-1.,-1.57087397835721));
#19862=CARTESIAN_POINT('Ctrl Pts',(-1.31731642317183,-1.,-1.57680056505585));
#19863=CARTESIAN_POINT('Ctrl Pts',(-1.31900135021428,-1.,-1.58274907898829));
#19864=CARTESIAN_POINT('Ctrl Pts',(-1.32064537110891,-1.,-1.58872057258244));
#19865=CARTESIAN_POINT('Ctrl Pts',(-1.32224985747686,-1.,-1.59471591079408));
#19866=CARTESIAN_POINT('Ctrl Pts',(-1.32381550858266,-1.,-1.600735118587));
#19867=CARTESIAN_POINT('Ctrl Pts',(-1.32534250785794,-1.,-1.6067775829097));
#19868=CARTESIAN_POINT('Ctrl Pts',(-1.32683074483365,-1.,-1.61284234015762));
#19869=CARTESIAN_POINT('Ctrl Pts',(-1.32828000610448,-1.,-1.61892832270723));
#19870=CARTESIAN_POINT('Ctrl Pts',(-1.32969019505665,-1.,-1.62503464209777));
#19871=CARTESIAN_POINT('Ctrl Pts',(-1.33106149345618,-1.,-1.63116079730887));
#19872=CARTESIAN_POINT('Ctrl Pts',(-1.33239425103694,-1.,-1.6373065347505));
#19873=CARTESIAN_POINT('Ctrl Pts',(-1.33368890676554,-1.,-1.64347174856007));
#19874=CARTESIAN_POINT('Ctrl Pts',(-1.33494590468003,-1.,-1.64965637286843));
#19875=CARTESIAN_POINT('Ctrl Pts',(-1.33616559745217,-1.,-1.65586025952651));
#19876=CARTESIAN_POINT('Ctrl Pts',(-1.33734820885331,-1.,-1.66208312542073));
#19877=CARTESIAN_POINT('Ctrl Pts',(-1.33849388654458,-1.,-1.66832460784078));
#19878=CARTESIAN_POINT('Ctrl Pts',(-1.33960273470372,-1.,-1.67458429426126));
#19879=CARTESIAN_POINT('Ctrl Pts',(-1.3406748518516,-1.,-1.68086176030308));
#19880=CARTESIAN_POINT('Ctrl Pts',(-1.34171037484673,-1.,-1.68715660868602));
#19881=CARTESIAN_POINT('Ctrl Pts',(-1.34270948206139,-1.,-1.6934684849664));
#19882=CARTESIAN_POINT('Ctrl Pts',(-1.34367237124322,-1.,-1.69979707754221));
#19883=CARTESIAN_POINT('Ctrl Pts',(-1.34459924533783,-1.,-1.70614212266676));
#19884=CARTESIAN_POINT('Ctrl Pts',(-1.34549029589563,-1.,-1.71250340687011));
#19885=CARTESIAN_POINT('Ctrl Pts',(-1.34634568653586,-1.,-1.7188807715095));
#19886=CARTESIAN_POINT('Ctrl Pts',(-1.34716554820013,-1.,-1.72527410681298));
#19887=CARTESIAN_POINT('Ctrl Pts',(-1.3477930915247,-1.,-1.73040149654497));
#19888=CARTESIAN_POINT('Ctrl Pts',(-1.34824783113158,-1.,-1.73425417886255));
#19889=CARTESIAN_POINT('Ctrl Pts',(-1.34854391898145,-1.,-1.73682580585819));
#19890=CARTESIAN_POINT('Ctrl Pts',(-1.34869019493419,-1.,-1.73811241238545));
#19891=CARTESIAN_POINT('',(-1.23627494547115,-1.,-1.81978687191668));
#19892=CARTESIAN_POINT('',(-1.34869019493419,-1.,-1.73811241238545));
#19893=CARTESIAN_POINT('',(-0.892032620296855,-1.,-1.5055822144029));
#19894=CARTESIAN_POINT('Ctrl Pts',(-1.23627494547115,-1.,-1.81978687191668));
#19895=CARTESIAN_POINT('Ctrl Pts',(-1.23509651170384,-1.,-1.81925017193531));
#19896=CARTESIAN_POINT('Ctrl Pts',(-1.23274224526804,-1.,-1.81817389920914));
#19897=CARTESIAN_POINT('Ctrl Pts',(-1.22921864890975,-1.,-1.81655087183054));
#19898=CARTESIAN_POINT('Ctrl Pts',(-1.22453613304507,-1.,-1.81436959209778));
#19899=CARTESIAN_POINT('Ctrl Pts',(-1.2187090610323,-1.,-1.81161420806172));
#19900=CARTESIAN_POINT('Ctrl Pts',(-1.2129081570818,-1.,-1.80882996916931));
#19901=CARTESIAN_POINT('Ctrl Pts',(-1.20713356605519,-1.,-1.80601678480772));
#19902=CARTESIAN_POINT('Ctrl Pts',(-1.2013854893912,-1.,-1.8031745483882));
#19903=CARTESIAN_POINT('Ctrl Pts',(-1.19566418930405,-1.,-1.80030314370121));
#19904=CARTESIAN_POINT('Ctrl Pts',(-1.1899699793456,-1.,-1.79740245923649));
#19905=CARTESIAN_POINT('Ctrl Pts',(-1.18430321697471,-1.,-1.79447240321572));
#19906=CARTESIAN_POINT('Ctrl Pts',(-1.17866429440781,-1.,-1.79151291552646));
#19907=CARTESIAN_POINT('Ctrl Pts',(-1.17305363177265,-1.,-1.78852398877523));
#19908=CARTESIAN_POINT('Ctrl Pts',(-1.16747166312239,-1.,-1.78550566040349));
#19909=CARTESIAN_POINT('Ctrl Pts',(-1.16191881298458,-1.,-1.78245795880949));
#19910=CARTESIAN_POINT('Ctrl Pts',(-1.15639547194689,-1.,-1.77938085564261));
#19911=CARTESIAN_POINT('Ctrl Pts',(-1.15090197841531,-1.,-1.77627422557034));
#19912=CARTESIAN_POINT('Ctrl Pts',(-1.14543858226948,-1.,-1.77313777896234));
#19913=CARTESIAN_POINT('Ctrl Pts',(-1.14000548337,-1.,-1.76997111386806));
#19914=CARTESIAN_POINT('Ctrl Pts',(-1.13460291804635,-1.,-1.76677384551883));
#19915=CARTESIAN_POINT('Ctrl Pts',(-1.12923123555076,-1.,-1.76354571966171));
#19916=CARTESIAN_POINT('Ctrl Pts',(-1.12389096855078,-1.,-1.76028671825084));
#19917=CARTESIAN_POINT('Ctrl Pts',(-1.11858293216752,-1.,-1.75699720772089));
#19918=CARTESIAN_POINT('Ctrl Pts',(-1.11330807582542,-1.,-1.75367772094617));
#19919=CARTESIAN_POINT('Ctrl Pts',(-1.10806728183003,-1.,-1.75032866075914));
#19920=CARTESIAN_POINT('Ctrl Pts',(-1.10286118991144,-1.,-1.74695004214924));
#19921=CARTESIAN_POINT('Ctrl Pts',(-1.09768999241229,-1.,-1.74354119236212));
#19922=CARTESIAN_POINT('Ctrl Pts',(-1.09255329056496,-1.,-1.74010053962252));
#19923=CARTESIAN_POINT('Ctrl Pts',(-1.08745056285429,-1.,-1.73662628326093));
#19924=CARTESIAN_POINT('Ctrl Pts',(-1.08238162784749,-1.,-1.73311705663407));
#19925=CARTESIAN_POINT('Ctrl Pts',(-1.0773470373727,-1.,-1.72957248977424));
#19926=CARTESIAN_POINT('Ctrl Pts',(-1.07234866990252,-1.,-1.72599406198489));
#19927=CARTESIAN_POINT('Ctrl Pts',(-1.06738966975463,-1.,-1.72238500928456));
#19928=CARTESIAN_POINT('Ctrl Pts',(-1.0624732468065,-1.,-1.71874858456908));
#19929=CARTESIAN_POINT('Ctrl Pts',(-1.05760163192481,-1.,-1.71508654427022));
#19930=CARTESIAN_POINT('Ctrl Pts',(-1.05277517202854,-1.,-1.71139783543986));
#19931=CARTESIAN_POINT('Ctrl Pts',(-1.0479908540499,-1.,-1.70767646263641));
#19932=CARTESIAN_POINT('Ctrl Pts',(-1.04324363334546,-1.,-1.70391338707969));
#19933=CARTESIAN_POINT('Ctrl Pts',(-1.03852922490782,-1.,-1.70010052930951));
#19934=CARTESIAN_POINT('Ctrl Pts',(-1.03384646003587,-1.,-1.69623414782769));
#19935=CARTESIAN_POINT('Ctrl Pts',(-1.02919977579155,-1.,-1.69231840863471));
#19936=CARTESIAN_POINT('Ctrl Pts',(-1.02460180535272,-1.,-1.68836910178475));
#19937=CARTESIAN_POINT('Ctrl Pts',(-1.02006795074222,-1.,-1.68440578021739));
#19938=CARTESIAN_POINT('Ctrl Pts',(-1.01561026162787,-1.,-1.6804428989482));
#19939=CARTESIAN_POINT('Ctrl Pts',(-1.01123236493507,-1.,-1.67648246776457));
#19940=CARTESIAN_POINT('Ctrl Pts',(-1.00692206696387,-1.,-1.67250335383248));
#19941=CARTESIAN_POINT('Ctrl Pts',(-1.00265091003682,-1.,-1.66846059277231));
#19942=CARTESIAN_POINT('Ctrl Pts',(-0.998389654952317,-1.,-1.66430758030304));
#19943=CARTESIAN_POINT('Ctrl Pts',(-0.994121836661116,-1.,-1.66001553809916));
#19944=CARTESIAN_POINT('Ctrl Pts',(-0.98985562785445,-1.,-1.65559044289746));
#19945=CARTESIAN_POINT('Ctrl Pts',(-0.985642622921626,-1.,-1.6511001661277));
#19946=CARTESIAN_POINT('Ctrl Pts',(-0.981562530940574,-1.,-1.64665139190834));
#19947=CARTESIAN_POINT('Ctrl Pts',(-0.977689794120297,-1.,-1.64233990826831));
#19948=CARTESIAN_POINT('Ctrl Pts',(-0.974066058287501,-1.,-1.63820952658157));
#19949=CARTESIAN_POINT('Ctrl Pts',(-0.970669715996356,-1.,-1.63420665729609));
#19950=CARTESIAN_POINT('Ctrl Pts',(-0.967387853228041,-1.,-1.63013849959083));
#19951=CARTESIAN_POINT('Ctrl Pts',(-0.964046107037821,-1.,-1.6257193066974));
#19952=CARTESIAN_POINT('Ctrl Pts',(-0.960438326099958,-1.,-1.62061638139929));
#19953=CARTESIAN_POINT('Ctrl Pts',(-0.956354422921573,-1.,-1.61449324337233));
#19954=CARTESIAN_POINT('Ctrl Pts',(-0.951613284361248,-1.,-1.60706069897794));
#19955=CARTESIAN_POINT('Ctrl Pts',(-0.946078063325796,-1.,-1.59810042045408));
#19956=CARTESIAN_POINT('Ctrl Pts',(-0.939646377909319,-1.,-1.58744937489796));
#19957=CARTESIAN_POINT('Ctrl Pts',(-0.932246680128849,-1.,-1.57499388385561));
#19958=CARTESIAN_POINT('Ctrl Pts',(-0.923832188966322,-1.,-1.56065988582509));
#19959=CARTESIAN_POINT('Ctrl Pts',(-0.91437591904658,-1.,-1.54440491152808));
#19960=CARTESIAN_POINT('Ctrl Pts',(-0.905967409640499,-1.,-1.52984849890434));
#19961=CARTESIAN_POINT('Ctrl Pts',(-0.89918504749193,-1.,-1.51805569591479));
#19962=CARTESIAN_POINT('Ctrl Pts',(-0.894452006967538,-1.,-1.50980486807181));
#19963=CARTESIAN_POINT('Ctrl Pts',(-0.892032620296855,-1.,-1.5055822144029));
#19964=CARTESIAN_POINT('',(-0.693717979106305,-1.,-1.60662857109684));
#19965=CARTESIAN_POINT('Origin',(0.,-1.,0.));
#19966=CARTESIAN_POINT('',(-0.745574324794401,-1.,-2.0698113262342));
#19967=CARTESIAN_POINT('Ctrl Pts',(-0.693717979106305,-1.,-1.60662857109684));
#19968=CARTESIAN_POINT('Ctrl Pts',(-0.69571209787897,-1.,-1.61106790957619));
#19969=CARTESIAN_POINT('Ctrl Pts',(-0.699605146398837,-1.,-1.61974673471117));
#19970=CARTESIAN_POINT('Ctrl Pts',(-0.705159151977294,-1.,-1.6321654166204));
#19971=CARTESIAN_POINT('Ctrl Pts',(-0.711993139340447,-1.,-1.64752408828442));
#19972=CARTESIAN_POINT('Ctrl Pts',(-0.71958543378795,-1.,-1.66472880551777));
#19973=CARTESIAN_POINT('Ctrl Pts',(-0.726235967982445,-1.,-1.67996158451922));
#19974=CARTESIAN_POINT('Ctrl Pts',(-0.731963238685357,-1.,-1.69326921972915));
#19975=CARTESIAN_POINT('Ctrl Pts',(-0.736799665716932,-1.,-1.70473309004249));
#19976=CARTESIAN_POINT('Ctrl Pts',(-0.74079516202821,-1.,-1.71447789751001));
#19977=CARTESIAN_POINT('Ctrl Pts',(-0.744021445433093,-1.,-1.72268229916769));
#19978=CARTESIAN_POINT('Ctrl Pts',(-0.746574710097752,-1.,-1.72958533647714));
#19979=CARTESIAN_POINT('Ctrl Pts',(-0.74858246295687,-1.,-1.7355035168033));
#19980=CARTESIAN_POINT('Ctrl Pts',(-0.750193435981249,-1.,-1.74080458267114));
#19981=CARTESIAN_POINT('Ctrl Pts',(-0.751555614164482,-1.,-1.74585086852502));
#19982=CARTESIAN_POINT('Ctrl Pts',(-0.752797683531314,-1.,-1.75095139468794));
#19983=CARTESIAN_POINT('Ctrl Pts',(-0.754009254027829,-1.,-1.75631083600019));
#19984=CARTESIAN_POINT('Ctrl Pts',(-0.755220979974461,-1.,-1.76197817240128));
#19985=CARTESIAN_POINT('Ctrl Pts',(-0.75642189602781,-1.,-1.76789396002998));
#19986=CARTESIAN_POINT('Ctrl Pts',(-0.757578264077029,-1.,-1.77394167108292));
#19987=CARTESIAN_POINT('Ctrl Pts',(-0.758650626677518,-1.,-1.77999411220945));
#19988=CARTESIAN_POINT('Ctrl Pts',(-0.759614401110189,-1.,-1.78596964884604));
#19989=CARTESIAN_POINT('Ctrl Pts',(-0.760469555880749,-1.,-1.7918581561088));
#19990=CARTESIAN_POINT('Ctrl Pts',(-0.761229695230558,-1.,-1.79768986997783));
#19991=CARTESIAN_POINT('Ctrl Pts',(-0.761915336443547,-1.,-1.80351583877342));
#19992=CARTESIAN_POINT('Ctrl Pts',(-0.762546129463938,-1.,-1.80938551463965));
#19993=CARTESIAN_POINT('Ctrl Pts',(-0.763132003836634,-1.,-1.8153211840553));
#19994=CARTESIAN_POINT('Ctrl Pts',(-0.763673465462726,-1.,-1.82131873145266));
#19995=CARTESIAN_POINT('Ctrl Pts',(-0.764165902605995,-1.,-1.82735991200065));
#19996=CARTESIAN_POINT('Ctrl Pts',(-0.764602549687853,-1.,-1.83342077227142));
#19997=CARTESIAN_POINT('Ctrl Pts',(-0.764978057881737,-1.,-1.83948181064835));
#19998=CARTESIAN_POINT('Ctrl Pts',(-0.765291664862029,-1.,-1.84553698875924));
#19999=CARTESIAN_POINT('Ctrl Pts',(-0.765545710619062,-1.,-1.85158945130063));
#20000=CARTESIAN_POINT('Ctrl Pts',(-0.765744212909318,-1.,-1.85764741390394));
#20001=CARTESIAN_POINT('Ctrl Pts',(-0.765891519092547,-1.,-1.86372027063312));
#20002=CARTESIAN_POINT('Ctrl Pts',(-0.765990708546091,-1.,-1.86981398314341));
#20003=CARTESIAN_POINT('Ctrl Pts',(-0.766042837036744,-1.,-1.87592888967883));
#20004=CARTESIAN_POINT('Ctrl Pts',(-0.766047794851865,-1.,-1.88206215302561));
#20005=CARTESIAN_POINT('Ctrl Pts',(-0.766004837062091,-1.,-1.88820926433409));
#20006=CARTESIAN_POINT('Ctrl Pts',(-0.765913193856978,-1.,-1.89436577771388));
#20007=CARTESIAN_POINT('Ctrl Pts',(-0.765772772593386,-1.,-1.90052930393596));
#20008=CARTESIAN_POINT('Ctrl Pts',(-0.765584196937919,-1.,-1.90669961402356));
#20009=CARTESIAN_POINT('Ctrl Pts',(-0.765348465884722,-1.,-1.91287765805169));
#20010=CARTESIAN_POINT('Ctrl Pts',(-0.765066729667088,-1.,-1.91906491634196));
#20011=CARTESIAN_POINT('Ctrl Pts',(-0.764740025488211,-1.,-1.92526263537048));
#20012=CARTESIAN_POINT('Ctrl Pts',(-0.764369010673941,-1.,-1.93147105496382));
#20013=CARTESIAN_POINT('Ctrl Pts',(-0.763954049121458,-1.,-1.93768964875886));
#20014=CARTESIAN_POINT('Ctrl Pts',(-0.763495333538629,-1.,-1.9439174661764));
#20015=CARTESIAN_POINT('Ctrl Pts',(-0.762992990878769,-1.,-1.95015342590024));
#20016=CARTESIAN_POINT('Ctrl Pts',(-0.762447203806179,-1.,-1.95639665309869));
#20017=CARTESIAN_POINT('Ctrl Pts',(-0.761858300014423,-1.,-1.96264672744186));
#20018=CARTESIAN_POINT('Ctrl Pts',(-0.76122669048382,-1.,-1.96890351582499));
#20019=CARTESIAN_POINT('Ctrl Pts',(-0.760552825409757,-1.,-1.97516705321494));
#20020=CARTESIAN_POINT('Ctrl Pts',(-0.75983714745219,-1.,-1.98143741418172));
#20021=CARTESIAN_POINT('Ctrl Pts',(-0.759080037802488,-1.,-1.98771456680874));
#20022=CARTESIAN_POINT('Ctrl Pts',(-0.758281796766761,-1.,-1.99399831098817));
#20023=CARTESIAN_POINT('Ctrl Pts',(-0.757442676862724,-1.,-2.00028834739178));
#20024=CARTESIAN_POINT('Ctrl Pts',(-0.75656290464667,-1.,-2.0065843158773));
#20025=CARTESIAN_POINT('Ctrl Pts',(-0.755642704957865,-1.,-2.01288584328084));
#20026=CARTESIAN_POINT('Ctrl Pts',(-0.754682330722816,-1.,-2.01919259405809));
#20027=CARTESIAN_POINT('Ctrl Pts',(-0.753682061112768,-1.,-2.02550428623313));
#20028=CARTESIAN_POINT('Ctrl Pts',(-0.752642180487211,-1.,-2.03182068456221));
#20029=CARTESIAN_POINT('Ctrl Pts',(-0.751562963361115,-1.,-2.03814160092099));
#20030=CARTESIAN_POINT('Ctrl Pts',(-0.750444657875576,-1.,-2.04446689147979));
#20031=CARTESIAN_POINT('Ctrl Pts',(-0.749287468665046,-1.,-2.05079645592154));
#20032=CARTESIAN_POINT('Ctrl Pts',(-0.748091554183802,-1.,-2.05713023031006));
#20033=CARTESIAN_POINT('Ctrl Pts',(-0.747103932787919,-1.,-2.06220058927826));
#20034=CARTESIAN_POINT('Ctrl Pts',(-0.7463458715442,-1.,-2.06600523016815));
#20035=CARTESIAN_POINT('Ctrl Pts',(-0.745832791378367,-1.,-2.06854248895728));
#20036=CARTESIAN_POINT('Ctrl Pts',(-0.745574324794401,-1.,-2.0698113262342));
#20037=CARTESIAN_POINT('',(-0.61342227326009,-1.,-2.11275013067528));
#20038=CARTESIAN_POINT('',(-0.745574324794401,-1.,-2.0698113262342));
#20039=CARTESIAN_POINT('',(-0.383122945602004,-1.,-1.7075470150345));
#20040=CARTESIAN_POINT('Ctrl Pts',(-0.61342227326009,-1.,-2.11275013067528));
#20041=CARTESIAN_POINT('Ctrl Pts',(-0.6124673655618,-1.,-2.11187554259986));
#20042=CARTESIAN_POINT('Ctrl Pts',(-0.610560911689899,-1.,-2.11012443807238));
#20043=CARTESIAN_POINT('Ctrl Pts',(-0.607711315454876,-1.,-2.1074919961518));
#20044=CARTESIAN_POINT('Ctrl Pts',(-0.60393203073603,-1.,-2.10397049886949));
#20045=CARTESIAN_POINT('Ctrl Pts',(-0.599241616420533,-1.,-2.0995493086477));
#20046=CARTESIAN_POINT('Ctrl Pts',(-0.594585006052162,-1.,-2.0951087622027));
#20047=CARTESIAN_POINT('Ctrl Pts',(-0.589962365403406,-1.,-2.09064881812129));
#20048=CARTESIAN_POINT('Ctrl Pts',(-0.585373918991617,-1.,-2.08616943727951));
#20049=CARTESIAN_POINT('Ctrl Pts',(-0.580819952108063,-1.,-2.08167059018418));
#20050=CARTESIAN_POINT('Ctrl Pts',(-0.576300797416844,-1.,-2.07715226767559));
#20051=CARTESIAN_POINT('Ctrl Pts',(-0.571816823242603,-1.,-2.07261449292824));
#20052=CARTESIAN_POINT('Ctrl Pts',(-0.567368421181087,-1.,-2.06805732997334));
#20053=CARTESIAN_POINT('Ctrl Pts',(-0.562955993082261,-1.,-2.06348090160589));
#20054=CARTESIAN_POINT('Ctrl Pts',(-0.558579940185151,-1.,-2.05888537756462));
#20055=CARTESIAN_POINT('Ctrl Pts',(-0.554240657463906,-1.,-2.05427091604413));
#20056=CARTESIAN_POINT('Ctrl Pts',(-0.549938525150295,-1.,-2.04963761077958));
#20057=CARTESIAN_POINT('Ctrl Pts',(-0.54567390381743,-1.,-2.04498544714588));
#20058=CARTESIAN_POINT('Ctrl Pts',(-0.541447120615659,-1.,-2.04031422690527));
#20059=CARTESIAN_POINT('Ctrl Pts',(-0.537258489833262,-1.,-2.03562362954037));
#20060=CARTESIAN_POINT('Ctrl Pts',(-0.533108355132977,-1.,-2.03091336214426));
#20061=CARTESIAN_POINT('Ctrl Pts',(-0.528997127241914,-1.,-2.0261832908329));
#20062=CARTESIAN_POINT('Ctrl Pts',(-0.524925318333476,-1.,-2.02143356304698));
#20063=CARTESIAN_POINT('Ctrl Pts',(-0.52089359039937,-1.,-2.01666477917286));
#20064=CARTESIAN_POINT('Ctrl Pts',(-0.516902681728687,-1.,-2.01187773939242));
#20065=CARTESIAN_POINT('Ctrl Pts',(-0.512953306961792,-1.,-2.00707309946949));
#20066=CARTESIAN_POINT('Ctrl Pts',(-0.509046069886157,-1.,-2.00225107134734));
#20067=CARTESIAN_POINT('Ctrl Pts',(-0.505181361323026,-1.,-1.99741107463572));
#20068=CARTESIAN_POINT('Ctrl Pts',(-0.501359287727146,-1.,-1.99255149126155));
#20069=CARTESIAN_POINT('Ctrl Pts',(-0.497579909545574,-1.,-1.98767044752932));
#20070=CARTESIAN_POINT('Ctrl Pts',(-0.493843476541495,-1.,-1.98276658761821));
#20071=CARTESIAN_POINT('Ctrl Pts',(-0.490150627860952,-1.,-1.97783973019229));
#20072=CARTESIAN_POINT('Ctrl Pts',(-0.486502692907659,-1.,-1.97289186263272));
#20073=CARTESIAN_POINT('Ctrl Pts',(-0.482901662120691,-1.,-1.96792703422362));
#20074=CARTESIAN_POINT('Ctrl Pts',(-0.479349583074855,-1.,-1.96294933055943));
#20075=CARTESIAN_POINT('Ctrl Pts',(-0.475848034683176,-1.,-1.95796111148177));
#20076=CARTESIAN_POINT('Ctrl Pts',(-0.472397672264072,-1.,-1.95296148278133));
#20077=CARTESIAN_POINT('Ctrl Pts',(-0.468997482913135,-1.,-1.94794381136514));
#20078=CARTESIAN_POINT('Ctrl Pts',(-0.46564546202603,-1.,-1.9428979419619));
#20079=CARTESIAN_POINT('Ctrl Pts',(-0.462340031009056,-1.,-1.93781486640821));
#20080=CARTESIAN_POINT('Ctrl Pts',(-0.459081234547926,-1.,-1.93269066517934));
#20081=CARTESIAN_POINT('Ctrl Pts',(-0.455872005174371,-1.,-1.92753067150476));
#20082=CARTESIAN_POINT('Ctrl Pts',(-0.452719478359432,-1.,-1.92235380648502));
#20083=CARTESIAN_POINT('Ctrl Pts',(-0.449632260106662,-1.,-1.91718342555755));
#20084=CARTESIAN_POINT('Ctrl Pts',(-0.446617343485711,-1.,-1.9120369998112));
#20085=CARTESIAN_POINT('Ctrl Pts',(-0.443677556849151,-1.,-1.90691756144898));
#20086=CARTESIAN_POINT('Ctrl Pts',(-0.440807833704038,-1.,-1.90180124389086));
#20087=CARTESIAN_POINT('Ctrl Pts',(-0.437995003948244,-1.,-1.89663648956466));
#20088=CARTESIAN_POINT('Ctrl Pts',(-0.435225660963383,-1.,-1.89136993975504));
#20089=CARTESIAN_POINT('Ctrl Pts',(-0.432493038548748,-1.,-1.88596913666793));
#20090=CARTESIAN_POINT('Ctrl Pts',(-0.429803062482344,-1.,-1.88044229001832));
#20091=CARTESIAN_POINT('Ctrl Pts',(-0.427183828519102,-1.,-1.87486989291484));
#20092=CARTESIAN_POINT('Ctrl Pts',(-0.424678177291359,-1.,-1.86937803944323));
#20093=CARTESIAN_POINT('Ctrl Pts',(-0.422327307418275,-1.,-1.86408083334028));
#20094=CARTESIAN_POINT('Ctrl Pts',(-0.420157287975619,-1.,-1.85903281096686));
#20095=CARTESIAN_POINT('Ctrl Pts',(-0.418164129143534,-1.,-1.85417632856234));
#20096=CARTESIAN_POINT('Ctrl Pts',(-0.416300022038864,-1.,-1.84929312929882));
#20097=CARTESIAN_POINT('Ctrl Pts',(-0.41448743825434,-1.,-1.8440575707371));
#20098=CARTESIAN_POINT('Ctrl Pts',(-0.412633125322162,-1.,-1.83808953475839));
#20099=CARTESIAN_POINT('Ctrl Pts',(-0.410641256301675,-1.,-1.83100408895216));
#20100=CARTESIAN_POINT('Ctrl Pts',(-0.408428948108533,-1.,-1.8224702267854));
#20101=CARTESIAN_POINT('Ctrl Pts',(-0.405933518411838,-1.,-1.81223801813988));
#20102=CARTESIAN_POINT('Ctrl Pts',(-0.403107976170441,-1.,-1.80012077176221));
#20103=CARTESIAN_POINT('Ctrl Pts',(-0.39991940378308,-1.,-1.78598826347533));
#20104=CARTESIAN_POINT('Ctrl Pts',(-0.39634619612042,-1.,-1.7697556004756));
#20105=CARTESIAN_POINT('Ctrl Pts',(-0.392375812294307,-1.,-1.75137405313962));
#20106=CARTESIAN_POINT('Ctrl Pts',(-0.388877023509191,-1.,-1.7349317097561));
#20107=CARTESIAN_POINT('Ctrl Pts',(-0.38607079032701,-1.,-1.72162022246158));
#20108=CARTESIAN_POINT('Ctrl Pts',(-0.384119047315542,-1.,-1.71231062891958));
#20109=CARTESIAN_POINT('Ctrl Pts',(-0.383122945602004,-1.,-1.7075470150345));
#20110=CARTESIAN_POINT('',(-0.163289472382896,-1.,-1.74236521665491));
#20111=CARTESIAN_POINT('Origin',(0.,-1.,0.));
#20112=CARTESIAN_POINT('',(-0.0694764450219581,-1.,-2.19890268624765));
#20113=CARTESIAN_POINT('Ctrl Pts',(-0.163289472382896,-1.,-1.74236521665491));
#20114=CARTESIAN_POINT('Ctrl Pts',(-0.163814161002002,-1.,-1.7472034950333));
#20115=CARTESIAN_POINT('Ctrl Pts',(-0.164834765707158,-1.,-1.75666056638427));
#20116=CARTESIAN_POINT('Ctrl Pts',(-0.1662793551464,-1.,-1.77018771684844));
#20117=CARTESIAN_POINT('Ctrl Pts',(-0.168032772805197,-1.,-1.7869064998507));
#20118=CARTESIAN_POINT('Ctrl Pts',(-0.169936923904608,-1.,-1.80561530629706));
#20119=CARTESIAN_POINT('Ctrl Pts',(-0.171554770204119,-1.,-1.82215766811545));
#20120=CARTESIAN_POINT('Ctrl Pts',(-0.1728894428919,-1.,-1.83658380527692));
#20121=CARTESIAN_POINT('Ctrl Pts',(-0.173946627587731,-1.,-1.8489811319852));
#20122=CARTESIAN_POINT('Ctrl Pts',(-0.17473525927603,-1.,-1.85948367088837));
#20123=CARTESIAN_POINT('Ctrl Pts',(-0.175268337590758,-1.,-1.86828349694799));
#20124=CARTESIAN_POINT('Ctrl Pts',(-0.175563480746485,-1.,-1.87563767773588));
#20125=CARTESIAN_POINT('Ctrl Pts',(-0.175644148889699,-1.,-1.88188663145367));
#20126=CARTESIAN_POINT('Ctrl Pts',(-0.175538155840648,-1.,-1.88742606273259));
#20127=CARTESIAN_POINT('Ctrl Pts',(-0.175274276190844,-1.,-1.892646301985));
#20128=CARTESIAN_POINT('Ctrl Pts',(-0.174879405091263,-1.,-1.89788101117132));
#20129=CARTESIAN_POINT('Ctrl Pts',(-0.174375518661085,-1.,-1.90335253862834));
#20130=CARTESIAN_POINT('Ctrl Pts',(-0.173776635257817,-1.,-1.90911693975267));
#20131=CARTESIAN_POINT('Ctrl Pts',(-0.173090695383496,-1.,-1.91511429159527));
#20132=CARTESIAN_POINT('Ctrl Pts',(-0.172321621259514,-1.,-1.9212233439798));
#20133=CARTESIAN_POINT('Ctrl Pts',(-0.171471191532988,-1.,-1.92731093582036));
#20134=CARTESIAN_POINT('Ctrl Pts',(-0.170541253116202,-1.,-1.93329183155539));
#20135=CARTESIAN_POINT('Ctrl Pts',(-0.169534904817491,-1.,-1.93915639211581));
#20136=CARTESIAN_POINT('Ctrl Pts',(-0.168455741607556,-1.,-1.94493757756931));
#20137=CARTESIAN_POINT('Ctrl Pts',(-0.167307501784475,-1.,-1.95069027794294));
#20138=CARTESIAN_POINT('Ctrl Pts',(-0.166093592002812,-1.,-1.9564675971873));
#20139=CARTESIAN_POINT('Ctrl Pts',(-0.164816568920269,-1.,-1.96229379940136));
#20140=CARTESIAN_POINT('Ctrl Pts',(-0.163478185457734,-1.,-1.96816512677967));
#20141=CARTESIAN_POINT('Ctrl Pts',(-0.162079693556289,-1.,-1.97406280235188));
#20142=CARTESIAN_POINT('Ctrl Pts',(-0.160622060784611,-1.,-1.97996195437559));
#20143=CARTESIAN_POINT('Ctrl Pts',(-0.159106226437299,-1.,-1.98584238283292));
#20144=CARTESIAN_POINT('Ctrl Pts',(-0.157533331459227,-1.,-1.99169810931908));
#20145=CARTESIAN_POINT('Ctrl Pts',(-0.155904629548783,-1.,-1.99753284771497));
#20146=CARTESIAN_POINT('Ctrl Pts',(-0.154221403049722,-1.,-2.00335565310543));
#20147=CARTESIAN_POINT('Ctrl Pts',(-0.15248488362145,-1.,-2.00917680318424));
#20148=CARTESIAN_POINT('Ctrl Pts',(-0.150696157673078,-1.,-2.01500291940238));
#20149=CARTESIAN_POINT('Ctrl Pts',(-0.148856124775337,-1.,-2.02083464969894));
#20150=CARTESIAN_POINT('Ctrl Pts',(-0.146965557332583,-1.,-2.02666926182017));
#20151=CARTESIAN_POINT('Ctrl Pts',(-0.145025140186057,-1.,-2.03250223739942));
#20152=CARTESIAN_POINT('Ctrl Pts',(-0.143035515058209,-1.,-2.03832911025912));
#20153=CARTESIAN_POINT('Ctrl Pts',(-0.140997332152546,-1.,-2.04414757947916));
#20154=CARTESIAN_POINT('Ctrl Pts',(-0.138911255368966,-1.,-2.04995762001328));
#20155=CARTESIAN_POINT('Ctrl Pts',(-0.136777941218044,-1.,-2.05576044414264));
#20156=CARTESIAN_POINT('Ctrl Pts',(-0.134598026192106,-1.,-2.06155781517842));
#20157=CARTESIAN_POINT('Ctrl Pts',(-0.13237211154771,-1.,-2.06735123910326));
#20158=CARTESIAN_POINT('Ctrl Pts',(-0.130100748328403,-1.,-2.07314114713063));
#20159=CARTESIAN_POINT('Ctrl Pts',(-0.12778444527612,-1.,-2.07892715110987));
#20160=CARTESIAN_POINT('Ctrl Pts',(-0.125423679412061,-1.,-2.08470840653643));
#20161=CARTESIAN_POINT('Ctrl Pts',(-0.123018905621083,-1.,-2.09048392424825));
#20162=CARTESIAN_POINT('Ctrl Pts',(-0.120570567965122,-1.,-2.0962529286773));
#20163=CARTESIAN_POINT('Ctrl Pts',(-0.118079107988355,-1.,-2.102015121329));
#20164=CARTESIAN_POINT('Ctrl Pts',(-0.115544957687926,-1.,-2.10777050261309));
#20165=CARTESIAN_POINT('Ctrl Pts',(-0.112968534419737,-1.,-2.11351924490306));
#20166=CARTESIAN_POINT('Ctrl Pts',(-0.110350236135025,-1.,-2.11926155590865));
#20167=CARTESIAN_POINT('Ctrl Pts',(-0.10769043523109,-1.,-2.12499752307));
#20168=CARTESIAN_POINT('Ctrl Pts',(-0.104989479152739,-1.,-2.13072704887293));
#20169=CARTESIAN_POINT('Ctrl Pts',(-0.1022477005561,-1.,-2.13644992667165));
#20170=CARTESIAN_POINT('Ctrl Pts',(-0.0994654261990915,-1.,-2.14216588396025));
#20171=CARTESIAN_POINT('Ctrl Pts',(-0.0966429852305459,-1.,-2.14787463531795));
#20172=CARTESIAN_POINT('Ctrl Pts',(-0.0937807218867643,-1.,-2.1535759397817));
#20173=CARTESIAN_POINT('Ctrl Pts',(-0.0908789888107265,-1.,-2.15926961544516));
#20174=CARTESIAN_POINT('Ctrl Pts',(-0.0879381291386923,-1.,-2.16495552645014));
#20175=CARTESIAN_POINT('Ctrl Pts',(-0.0849584620835372,-1.,-2.17063357870952));
#20176=CARTESIAN_POINT('Ctrl Pts',(-0.0819402680872765,-1.,-2.176303712113));
#20177=CARTESIAN_POINT('Ctrl Pts',(-0.0788837727685243,-1.,-2.18196589448887));
#20178=CARTESIAN_POINT('Ctrl Pts',(-0.0757891465836148,-1.,-2.1876201139953));
#20179=CARTESIAN_POINT('Ctrl Pts',(-0.0732830357306725,-1.,-2.19213712013662));
#20180=CARTESIAN_POINT('Ctrl Pts',(-0.0713863779526154,-1.,-2.19552129484002));
#20181=CARTESIAN_POINT('Ctrl Pts',(-0.070114353632549,-1.,-2.19777582085423));
#20182=CARTESIAN_POINT('Ctrl Pts',(-0.0694764450219581,-1.,-2.19890268624765));
#20183=CARTESIAN_POINT('',(0.0694764450219584,-1.,-2.19890268624765));
#20184=CARTESIAN_POINT('',(-0.0694764450219581,-1.,-2.19890268624765));
#20185=CARTESIAN_POINT('',(0.163289472382896,-1.,-1.74236521665491));
#20186=CARTESIAN_POINT('Ctrl Pts',(0.0694764450219584,-1.,-2.19890268624765));
#20187=CARTESIAN_POINT('Ctrl Pts',(0.0701143536324926,-1.,-2.19777582085261));
#20188=CARTESIAN_POINT('Ctrl Pts',(0.0713863779524627,-1.,-2.19552129483562));
#20189=CARTESIAN_POINT('Ctrl Pts',(0.0732830357304276,-1.,-2.19213712012956));
#20190=CARTESIAN_POINT('Ctrl Pts',(0.0757891465833411,-1.,-2.1876201139874));
#20191=CARTESIAN_POINT('Ctrl Pts',(0.0788837727683228,-1.,-2.18196589448304));
#20192=CARTESIAN_POINT('Ctrl Pts',(0.0819402680871939,-1.,-2.1763037121106));
#20193=CARTESIAN_POINT('Ctrl Pts',(0.0849584620835643,-1.,-2.17063357871031));
#20194=CARTESIAN_POINT('Ctrl Pts',(0.0879381291387823,-1.,-2.16495552645275));
#20195=CARTESIAN_POINT('Ctrl Pts',(0.0908789888108266,-1.,-2.15926961544808));
#20196=CARTESIAN_POINT('Ctrl Pts',(0.0937807218868345,-1.,-2.15357593978377));
#20197=CARTESIAN_POINT('Ctrl Pts',(0.0966429852305689,-1.,-2.14787463531864));
#20198=CARTESIAN_POINT('Ctrl Pts',(0.0994654261990743,-1.,-2.14216588395974));
#20199=CARTESIAN_POINT('Ctrl Pts',(0.102247700556064,-1.,-2.13644992667052));
#20200=CARTESIAN_POINT('Ctrl Pts',(0.104989479152703,-1.,-2.1307270488718));
#20201=CARTESIAN_POINT('Ctrl Pts',(0.107690435231068,-1.,-2.12499752306927));
#20202=CARTESIAN_POINT('Ctrl Pts',(0.11035023613502,-1.,-2.11926155590849));
#20203=CARTESIAN_POINT('Ctrl Pts',(0.112968534419746,-1.,-2.11351924490335));
#20204=CARTESIAN_POINT('Ctrl Pts',(0.11554495768794,-1.,-2.10777050261359));
#20205=CARTESIAN_POINT('Ctrl Pts',(0.118079107988368,-1.,-2.10201512132945));
#20206=CARTESIAN_POINT('Ctrl Pts',(0.120570567965129,-1.,-2.09625292867756));
#20207=CARTESIAN_POINT('Ctrl Pts',(0.123018905621083,-1.,-2.09048392424826));
#20208=CARTESIAN_POINT('Ctrl Pts',(0.125423679412058,-1.,-2.08470840653628));
#20209=CARTESIAN_POINT('Ctrl Pts',(0.127784445276116,-1.,-2.07892715110967));
#20210=CARTESIAN_POINT('Ctrl Pts',(0.1301007483284,-1.,-2.07314114713047));
#20211=CARTESIAN_POINT('Ctrl Pts',(0.13237211154771,-1.,-2.06735123910319));
#20212=CARTESIAN_POINT('Ctrl Pts',(0.134598026192107,-1.,-2.06155781517844));
#20213=CARTESIAN_POINT('Ctrl Pts',(0.136777941218044,-1.,-2.0557604441427));
#20214=CARTESIAN_POINT('Ctrl Pts',(0.138911255368966,-1.,-2.04995762001333));
#20215=CARTESIAN_POINT('Ctrl Pts',(0.140997332152545,-1.,-2.04414757947919));
#20216=CARTESIAN_POINT('Ctrl Pts',(0.143035515058208,-1.,-2.03832911025913));
#20217=CARTESIAN_POINT('Ctrl Pts',(0.145025140186058,-1.,-2.03250223739941));
#20218=CARTESIAN_POINT('Ctrl Pts',(0.146965557332586,-1.,-2.02666926182017));
#20219=CARTESIAN_POINT('Ctrl Pts',(0.148856124775343,-1.,-2.02083464969897));
#20220=CARTESIAN_POINT('Ctrl Pts',(0.150696157673084,-1.,-2.01500291940243));
#20221=CARTESIAN_POINT('Ctrl Pts',(0.152484883621452,-1.,-2.00917680318426));
#20222=CARTESIAN_POINT('Ctrl Pts',(0.154221403049719,-1.,-2.00335565310539));
#20223=CARTESIAN_POINT('Ctrl Pts',(0.155904629548774,-1.,-1.99753284771487));
#20224=CARTESIAN_POINT('Ctrl Pts',(0.157533331459215,-1.,-1.99169810931893));
#20225=CARTESIAN_POINT('Ctrl Pts',(0.159106226437288,-1.,-1.98584238283279));
#20226=CARTESIAN_POINT('Ctrl Pts',(0.16062206078461,-1.,-1.97996195437557));
#20227=CARTESIAN_POINT('Ctrl Pts',(0.162079693556302,-1.,-1.97406280235204));
#20228=CARTESIAN_POINT('Ctrl Pts',(0.16347818545776,-1.,-1.96816512678));
#20229=CARTESIAN_POINT('Ctrl Pts',(0.1648165689203,-1.,-1.96229379940174));
#20230=CARTESIAN_POINT('Ctrl Pts',(0.166093592002833,-1.,-1.95646759718755));
#20231=CARTESIAN_POINT('Ctrl Pts',(0.167307501784469,-1.,-1.95069027794286));
#20232=CARTESIAN_POINT('Ctrl Pts',(0.168455741607516,-1.,-1.94493757756879));
#20233=CARTESIAN_POINT('Ctrl Pts',(0.169534904817425,-1.,-1.93915639211497));
#20234=CARTESIAN_POINT('Ctrl Pts',(0.170541253116136,-1.,-1.93329183155455));
#20235=CARTESIAN_POINT('Ctrl Pts',(0.17147119153296,-1.,-1.92731093582));
#20236=CARTESIAN_POINT('Ctrl Pts',(0.172321621259557,-1.,-1.92122334398034));
#20237=CARTESIAN_POINT('Ctrl Pts',(0.173090695383619,-1.,-1.91511429159681));
#20238=CARTESIAN_POINT('Ctrl Pts',(0.173776635257984,-1.,-1.90911693975475));
#20239=CARTESIAN_POINT('Ctrl Pts',(0.174375518661222,-1.,-1.90335253863003));
#20240=CARTESIAN_POINT('Ctrl Pts',(0.174879405091277,-1.,-1.89788101117148));
#20241=CARTESIAN_POINT('Ctrl Pts',(0.175274276190664,-1.,-1.89264630198279));
#20242=CARTESIAN_POINT('Ctrl Pts',(0.175538155840286,-1.,-1.88742606272818));
#20243=CARTESIAN_POINT('Ctrl Pts',(0.175644148889271,-1.,-1.88188663144846));
#20244=CARTESIAN_POINT('Ctrl Pts',(0.175563480746205,-1.,-1.87563767773249));
#20245=CARTESIAN_POINT('Ctrl Pts',(0.175268337590901,-1.,-1.86828349694972));
#20246=CARTESIAN_POINT('Ctrl Pts',(0.174735259276856,-1.,-1.85948367089838));
#20247=CARTESIAN_POINT('Ctrl Pts',(0.173946627589401,-1.,-1.84898113200543));
#20248=CARTESIAN_POINT('Ctrl Pts',(0.17288944289442,-1.,-1.83658380530747));
#20249=CARTESIAN_POINT('Ctrl Pts',(0.171554770207306,-1.,-1.82215766815414));
#20250=CARTESIAN_POINT('Ctrl Pts',(0.169936923908078,-1.,-1.80561530633924));
#20251=CARTESIAN_POINT('Ctrl Pts',(0.16803277280837,-1.,-1.78690649988931));
#20252=CARTESIAN_POINT('Ctrl Pts',(0.166279355148738,-1.,-1.77018771687692));
#20253=CARTESIAN_POINT('Ctrl Pts',(0.164834765708484,-1.,-1.75666056640041));
#20254=CARTESIAN_POINT('Ctrl Pts',(0.163814161002474,-1.,-1.74720349503904));
#20255=CARTESIAN_POINT('Ctrl Pts',(0.163289472382896,-1.,-1.74236521665491));
#20256=CARTESIAN_POINT('',(0.383122945602004,-1.,-1.7075470150345));
#20257=CARTESIAN_POINT('Origin',(0.,-1.,0.));
#20258=CARTESIAN_POINT('',(0.61342227326009,-1.,-2.11275013067528));
#20259=CARTESIAN_POINT('Ctrl Pts',(0.383122945602004,-1.,-1.7075470150345));
#20260=CARTESIAN_POINT('Ctrl Pts',(0.384119047314215,-1.,-1.71231062891398));
#20261=CARTESIAN_POINT('Ctrl Pts',(0.386070790323281,-1.,-1.72162022244582));
#20262=CARTESIAN_POINT('Ctrl Pts',(0.388877023502615,-1.,-1.73493170972829));
#20263=CARTESIAN_POINT('Ctrl Pts',(0.392375812285395,-1.,-1.75137405310193));
#20264=CARTESIAN_POINT('Ctrl Pts',(0.396346196110688,-1.,-1.76975560043442));
#20265=CARTESIAN_POINT('Ctrl Pts',(0.399919403774155,-1.,-1.78598826343754));
#20266=CARTESIAN_POINT('Ctrl Pts',(0.403107976163396,-1.,-1.80012077173238));
#20267=CARTESIAN_POINT('Ctrl Pts',(0.405933518407175,-1.,-1.81223801812013));
#20268=CARTESIAN_POINT('Ctrl Pts',(0.408428948106227,-1.,-1.82247022677562));
#20269=CARTESIAN_POINT('Ctrl Pts',(0.410641256301276,-1.,-1.83100408895047));
#20270=CARTESIAN_POINT('Ctrl Pts',(0.412633125322945,-1.,-1.8380895347617));
#20271=CARTESIAN_POINT('Ctrl Pts',(0.414487438255542,-1.,-1.84405757074218));
#20272=CARTESIAN_POINT('Ctrl Pts',(0.416300022039885,-1.,-1.84929312930314));
#20273=CARTESIAN_POINT('Ctrl Pts',(0.418164129144045,-1.,-1.8541763285645));
#20274=CARTESIAN_POINT('Ctrl Pts',(0.420157287975583,-1.,-1.8590328109667));
#20275=CARTESIAN_POINT('Ctrl Pts',(0.422327307417884,-1.,-1.86408083333863));
#20276=CARTESIAN_POINT('Ctrl Pts',(0.424678177290876,-1.,-1.8693780394412));
#20277=CARTESIAN_POINT('Ctrl Pts',(0.427183828518743,-1.,-1.87486989291334));
#20278=CARTESIAN_POINT('Ctrl Pts',(0.429803062482217,-1.,-1.88044229001779));
#20279=CARTESIAN_POINT('Ctrl Pts',(0.432493038548833,-1.,-1.88596913666828));
#20280=CARTESIAN_POINT('Ctrl Pts',(0.43522566096358,-1.,-1.89136993975585));
#20281=CARTESIAN_POINT('Ctrl Pts',(0.437995003948443,-1.,-1.89663648956549));
#20282=CARTESIAN_POINT('Ctrl Pts',(0.44080783370416,-1.,-1.90180124389137));
#20283=CARTESIAN_POINT('Ctrl Pts',(0.44367755684917,-1.,-1.90691756144906));
#20284=CARTESIAN_POINT('Ctrl Pts',(0.446617343485651,-1.,-1.91203699981095));
#20285=CARTESIAN_POINT('Ctrl Pts',(0.449632260106572,-1.,-1.91718342555717));
#20286=CARTESIAN_POINT('Ctrl Pts',(0.452719478359356,-1.,-1.9223538064847));
#20287=CARTESIAN_POINT('Ctrl Pts',(0.455872005174335,-1.,-1.92753067150461));
#20288=CARTESIAN_POINT('Ctrl Pts',(0.459081234547931,-1.,-1.93269066517936));
#20289=CARTESIAN_POINT('Ctrl Pts',(0.462340031009087,-1.,-1.93781486640834));
#20290=CARTESIAN_POINT('Ctrl Pts',(0.465645462026064,-1.,-1.94289794196205));
#20291=CARTESIAN_POINT('Ctrl Pts',(0.468997482913158,-1.,-1.94794381136524));
#20292=CARTESIAN_POINT('Ctrl Pts',(0.472397672264079,-1.,-1.95296148278136));
#20293=CARTESIAN_POINT('Ctrl Pts',(0.475848034683171,-1.,-1.95796111148175));
#20294=CARTESIAN_POINT('Ctrl Pts',(0.479349583074846,-1.,-1.96294933055938));
#20295=CARTESIAN_POINT('Ctrl Pts',(0.482901662120686,-1.,-1.96792703422358));
#20296=CARTESIAN_POINT('Ctrl Pts',(0.486502692907661,-1.,-1.97289186263272));
#20297=CARTESIAN_POINT('Ctrl Pts',(0.490150627860955,-1.,-1.97783973019229));
#20298=CARTESIAN_POINT('Ctrl Pts',(0.493843476541492,-1.,-1.9827665876182));
#20299=CARTESIAN_POINT('Ctrl Pts',(0.497579909545564,-1.,-1.98767044752929));
#20300=CARTESIAN_POINT('Ctrl Pts',(0.501359287727129,-1.,-1.9925514912615));
#20301=CARTESIAN_POINT('Ctrl Pts',(0.505181361323011,-1.,-1.99741107463567));
#20302=CARTESIAN_POINT('Ctrl Pts',(0.509046069886152,-1.,-2.00225107134733));
#20303=CARTESIAN_POINT('Ctrl Pts',(0.512953306961813,-1.,-2.00707309946955));
#20304=CARTESIAN_POINT('Ctrl Pts',(0.516902681728733,-1.,-2.01187773939257));
#20305=CARTESIAN_POINT('Ctrl Pts',(0.520893590399428,-1.,-2.01666477917306));
#20306=CARTESIAN_POINT('Ctrl Pts',(0.524925318333518,-1.,-2.02143356304712));
#20307=CARTESIAN_POINT('Ctrl Pts',(0.52899712724191,-1.,-2.02618329083289));
#20308=CARTESIAN_POINT('Ctrl Pts',(0.533108355132905,-1.,-2.03091336214401));
#20309=CARTESIAN_POINT('Ctrl Pts',(0.537258489833134,-1.,-2.03562362953993));
#20310=CARTESIAN_POINT('Ctrl Pts',(0.54144712061552,-1.,-2.0403142269048));
#20311=CARTESIAN_POINT('Ctrl Pts',(0.545673903817348,-1.,-2.0449854471456));
#20312=CARTESIAN_POINT('Ctrl Pts',(0.549938525150342,-1.,-2.04963761077974));
#20313=CARTESIAN_POINT('Ctrl Pts',(0.554240657464109,-1.,-2.05427091604482));
#20314=CARTESIAN_POINT('Ctrl Pts',(0.558579940185467,-1.,-2.05888537756571));
#20315=CARTESIAN_POINT('Ctrl Pts',(0.562955993082574,-1.,-2.06348090160697));
#20316=CARTESIAN_POINT('Ctrl Pts',(0.567368421181229,-1.,-2.06805732997383));
#20317=CARTESIAN_POINT('Ctrl Pts',(0.571816823242411,-1.,-2.07261449292758));
#20318=CARTESIAN_POINT('Ctrl Pts',(0.576300797416274,-1.,-2.07715226767361));
#20319=CARTESIAN_POINT('Ctrl Pts',(0.580819952107256,-1.,-2.08167059018138));
#20320=CARTESIAN_POINT('Ctrl Pts',(0.585373918990895,-1.,-2.086169437277));
#20321=CARTESIAN_POINT('Ctrl Pts',(0.589962365403189,-1.,-2.09064881812053));
#20322=CARTESIAN_POINT('Ctrl Pts',(0.594585006052823,-1.,-2.09510876220501));
#20323=CARTESIAN_POINT('Ctrl Pts',(0.599241616422144,-1.,-2.09954930865331));
#20324=CARTESIAN_POINT('Ctrl Pts',(0.603932030738212,-1.,-2.10397049887709));
#20325=CARTESIAN_POINT('Ctrl Pts',(0.607711315456826,-1.,-2.10749199615859));
#20326=CARTESIAN_POINT('Ctrl Pts',(0.610560911691113,-1.,-2.11012443807661));
#20327=CARTESIAN_POINT('Ctrl Pts',(0.61246736556225,-1.,-2.11187554260142));
#20328=CARTESIAN_POINT('Ctrl Pts',(0.61342227326009,-1.,-2.11275013067528));
#20329=CARTESIAN_POINT('',(0.745574324794401,-1.,-2.0698113262342));
#20330=CARTESIAN_POINT('',(0.61342227326009,-1.,-2.11275013067528));
#20331=CARTESIAN_POINT('',(0.693717979106306,-1.,-1.60662857109684));
#20332=CARTESIAN_POINT('Ctrl Pts',(0.745574324794401,-1.,-2.0698113262342));
#20333=CARTESIAN_POINT('Ctrl Pts',(0.74583279137781,-1.,-2.06854248895575));
#20334=CARTESIAN_POINT('Ctrl Pts',(0.746345871542695,-1.,-2.06600523016401));
#20335=CARTESIAN_POINT('Ctrl Pts',(0.747103932785504,-1.,-2.06220058927162));
#20336=CARTESIAN_POINT('Ctrl Pts',(0.748091554181101,-1.,-2.05713023030263));
#20337=CARTESIAN_POINT('Ctrl Pts',(0.749287468663053,-1.,-2.05079645591606));
#20338=CARTESIAN_POINT('Ctrl Pts',(0.750444657874758,-1.,-2.04446689147754));
#20339=CARTESIAN_POINT('Ctrl Pts',(0.751562963361383,-1.,-2.03814160092173));
#20340=CARTESIAN_POINT('Ctrl Pts',(0.752642180488104,-1.,-2.03182068456467));
#20341=CARTESIAN_POINT('Ctrl Pts',(0.753682061113765,-1.,-2.02550428623587));
#20342=CARTESIAN_POINT('Ctrl Pts',(0.75468233072352,-1.,-2.01919259406003));
#20343=CARTESIAN_POINT('Ctrl Pts',(0.7556427049581,-1.,-2.01288584328149));
#20344=CARTESIAN_POINT('Ctrl Pts',(0.756562904646496,-1.,-2.00658431587682));
#20345=CARTESIAN_POINT('Ctrl Pts',(0.757442676862341,-1.,-2.00028834739072));
#20346=CARTESIAN_POINT('Ctrl Pts',(0.758281796766377,-1.,-1.9939983109871));
#20347=CARTESIAN_POINT('Ctrl Pts',(0.759080037802242,-1.,-1.98771456680806));
#20348=CARTESIAN_POINT('Ctrl Pts',(0.759837147452135,-1.,-1.98143741418156));
#20349=CARTESIAN_POINT('Ctrl Pts',(0.760552825409855,-1.,-1.97516705321521));
#20350=CARTESIAN_POINT('Ctrl Pts',(0.761226690483986,-1.,-1.96890351582545));
#20351=CARTESIAN_POINT('Ctrl Pts',(0.761858300014575,-1.,-1.96264672744229));
#20352=CARTESIAN_POINT('Ctrl Pts',(0.762447203806263,-1.,-1.95639665309893));
#20353=CARTESIAN_POINT('Ctrl Pts',(0.762992990878774,-1.,-1.95015342590025));
#20354=CARTESIAN_POINT('Ctrl Pts',(0.76349533353858,-1.,-1.94391746617626));
#20355=CARTESIAN_POINT('Ctrl Pts',(0.763954049121393,-1.,-1.93768964875867));
#20356=CARTESIAN_POINT('Ctrl Pts',(0.764369010673889,-1.,-1.93147105496367));
#20357=CARTESIAN_POINT('Ctrl Pts',(0.764740025488189,-1.,-1.92526263537041));
#20358=CARTESIAN_POINT('Ctrl Pts',(0.765066729667095,-1.,-1.91906491634197));
#20359=CARTESIAN_POINT('Ctrl Pts',(0.765348465884739,-1.,-1.91287765805174));
#20360=CARTESIAN_POINT('Ctrl Pts',(0.765584196937936,-1.,-1.90669961402362));
#20361=CARTESIAN_POINT('Ctrl Pts',(0.765772772593395,-1.,-1.90052930393599));
#20362=CARTESIAN_POINT('Ctrl Pts',(0.765913193856979,-1.,-1.89436577771389));
#20363=CARTESIAN_POINT('Ctrl Pts',(0.76600483706209,-1.,-1.88820926433409));
#20364=CARTESIAN_POINT('Ctrl Pts',(0.766047794851868,-1.,-1.88206215302561));
#20365=CARTESIAN_POINT('Ctrl Pts',(0.766042837036759,-1.,-1.87592888967886));
#20366=CARTESIAN_POINT('Ctrl Pts',(0.765990708546111,-1.,-1.86981398314345));
#20367=CARTESIAN_POINT('Ctrl Pts',(0.765891519092557,-1.,-1.86372027063315));
#20368=CARTESIAN_POINT('Ctrl Pts',(0.765744212909305,-1.,-1.85764741390391));
#20369=CARTESIAN_POINT('Ctrl Pts',(0.765545710619023,-1.,-1.85158945130054));
#20370=CARTESIAN_POINT('Ctrl Pts',(0.765291664861971,-1.,-1.84553698875911));
#20371=CARTESIAN_POINT('Ctrl Pts',(0.764978057881687,-1.,-1.83948181064823));
#20372=CARTESIAN_POINT('Ctrl Pts',(0.764602549687845,-1.,-1.8334207722714));
#20373=CARTESIAN_POINT('Ctrl Pts',(0.764165902606055,-1.,-1.8273599120008));
#20374=CARTESIAN_POINT('Ctrl Pts',(0.763673465462854,-1.,-1.82131873145297));
#20375=CARTESIAN_POINT('Ctrl Pts',(0.763132003836783,-1.,-1.81532118405566));
#20376=CARTESIAN_POINT('Ctrl Pts',(0.762546129464036,-1.,-1.80938551463989));
#20377=CARTESIAN_POINT('Ctrl Pts',(0.761915336443515,-1.,-1.80351583877334));
#20378=CARTESIAN_POINT('Ctrl Pts',(0.761229695230359,-1.,-1.79768986997735));
#20379=CARTESIAN_POINT('Ctrl Pts',(0.760469555880425,-1.,-1.79185815610802));
#20380=CARTESIAN_POINT('Ctrl Pts',(0.759614401109868,-1.,-1.78596964884527));
#20381=CARTESIAN_POINT('Ctrl Pts',(0.75865062667738,-1.,-1.77999411220912));
#20382=CARTESIAN_POINT('Ctrl Pts',(0.757578264077238,-1.,-1.77394167108342));
#20383=CARTESIAN_POINT('Ctrl Pts',(0.756421896028403,-1.,-1.76789396003141));
#20384=CARTESIAN_POINT('Ctrl Pts',(0.755220979975262,-1.,-1.7619781724032));
#20385=CARTESIAN_POINT('Ctrl Pts',(0.75400925402848,-1.,-1.75631083600175));
#20386=CARTESIAN_POINT('Ctrl Pts',(0.752797683531377,-1.,-1.75095139468809));
#20387=CARTESIAN_POINT('Ctrl Pts',(0.751555614163629,-1.,-1.74585086852298));
#20388=CARTESIAN_POINT('Ctrl Pts',(0.75019343597954,-1.,-1.74080458266705));
#20389=CARTESIAN_POINT('Ctrl Pts',(0.748582462954854,-1.,-1.73550351679848));
#20390=CARTESIAN_POINT('Ctrl Pts',(0.746574710096436,-1.,-1.72958533647399));
#20391=CARTESIAN_POINT('Ctrl Pts',(0.744021445433764,-1.,-1.7226822991693));
#20392=CARTESIAN_POINT('Ctrl Pts',(0.740795162032087,-1.,-1.71447789751927));
#20393=CARTESIAN_POINT('Ctrl Pts',(0.736799665724771,-1.,-1.70473309006121));
#20394=CARTESIAN_POINT('Ctrl Pts',(0.731963238697195,-1.,-1.69326921975743));
#20395=CARTESIAN_POINT('Ctrl Pts',(0.726235967997433,-1.,-1.67996158455503));
#20396=CARTESIAN_POINT('Ctrl Pts',(0.719585433804282,-1.,-1.6647288055568));
#20397=CARTESIAN_POINT('Ctrl Pts',(0.711993139355394,-1.,-1.64752408832016));
#20398=CARTESIAN_POINT('Ctrl Pts',(0.705159151988319,-1.,-1.63216541664676));
#20399=CARTESIAN_POINT('Ctrl Pts',(0.699605146405088,-1.,-1.61974673472612));
#20400=CARTESIAN_POINT('Ctrl Pts',(0.695712097881194,-1.,-1.61106790958151));
#20401=CARTESIAN_POINT('Ctrl Pts',(0.693717979106306,-1.,-1.60662857109684));
#20402=CARTESIAN_POINT('',(0.892032620296855,-1.,-1.5055822144029));
#20403=CARTESIAN_POINT('Origin',(0.,-1.,0.));
#20404=CARTESIAN_POINT('',(1.23627494547115,-1.,-1.81978687191668));
#20405=CARTESIAN_POINT('Ctrl Pts',(0.892032620296855,-1.,-1.5055822144029));
#20406=CARTESIAN_POINT('Ctrl Pts',(0.894452006964543,-1.,-1.50980486806688));
#20407=CARTESIAN_POINT('Ctrl Pts',(0.89918504748351,-1.,-1.51805569590094));
#20408=CARTESIAN_POINT('Ctrl Pts',(0.905967409625651,-1.,-1.52984849887993));
#20409=CARTESIAN_POINT('Ctrl Pts',(0.914375919026456,-1.,-1.54440491149498));
#20410=CARTESIAN_POINT('Ctrl Pts',(0.923832188944341,-1.,-1.56065988578893));
#20411=CARTESIAN_POINT('Ctrl Pts',(0.932246680108685,-1.,-1.57499388382243));
#20412=CARTESIAN_POINT('Ctrl Pts',(0.939646377893399,-1.,-1.58744937487176));
#20413=CARTESIAN_POINT('Ctrl Pts',(0.946078063315257,-1.,-1.59810042043673));
#20414=CARTESIAN_POINT('Ctrl Pts',(0.951613284356035,-1.,-1.60706069896936));
#20415=CARTESIAN_POINT('Ctrl Pts',(0.95635442292067,-1.,-1.61449324337085));
#20416=CARTESIAN_POINT('Ctrl Pts',(0.960438326101728,-1.,-1.62061638140221));
#20417=CARTESIAN_POINT('Ctrl Pts',(0.964046107040535,-1.,-1.62571930670187));
#20418=CARTESIAN_POINT('Ctrl Pts',(0.967387853230345,-1.,-1.63013849959462));
#20419=CARTESIAN_POINT('Ctrl Pts',(0.970669715997509,-1.,-1.63420665729798));
#20420=CARTESIAN_POINT('Ctrl Pts',(0.974066058287418,-1.,-1.63820952658144));
#20421=CARTESIAN_POINT('Ctrl Pts',(0.977689794119416,-1.,-1.64233990826687));
#20422=CARTESIAN_POINT('Ctrl Pts',(0.981562530939489,-1.,-1.64665139190656));
#20423=CARTESIAN_POINT('Ctrl Pts',(0.98564262292082,-1.,-1.65110016612638));
#20424=CARTESIAN_POINT('Ctrl Pts',(0.989855627854164,-1.,-1.65559044289699));
#20425=CARTESIAN_POINT('Ctrl Pts',(0.994121836661305,-1.,-1.66001553809947));
#20426=CARTESIAN_POINT('Ctrl Pts',(0.998389654952757,-1.,-1.66430758030376));
#20427=CARTESIAN_POINT('Ctrl Pts',(1.00265091003727,-1.,-1.66846059277303));
#20428=CARTESIAN_POINT('Ctrl Pts',(1.00692206696414,-1.,-1.67250335383293));
#20429=CARTESIAN_POINT('Ctrl Pts',(1.01123236493511,-1.,-1.67648246776464));
#20430=CARTESIAN_POINT('Ctrl Pts',(1.01561026162773,-1.,-1.68044289894798));
#20431=CARTESIAN_POINT('Ctrl Pts',(1.02006795074201,-1.,-1.68440578021706));
#20432=CARTESIAN_POINT('Ctrl Pts',(1.02460180535255,-1.,-1.68836910178447));
#20433=CARTESIAN_POINT('Ctrl Pts',(1.02919977579147,-1.,-1.69231840863458));
#20434=CARTESIAN_POINT('Ctrl Pts',(1.03384646003588,-1.,-1.69623414782771));
#20435=CARTESIAN_POINT('Ctrl Pts',(1.03852922490789,-1.,-1.70010052930962));
#20436=CARTESIAN_POINT('Ctrl Pts',(1.04324363334554,-1.,-1.70391338707982));
#20437=CARTESIAN_POINT('Ctrl Pts',(1.04799085404995,-1.,-1.70767646263649));
#20438=CARTESIAN_POINT('Ctrl Pts',(1.05277517202855,-1.,-1.71139783543989));
#20439=CARTESIAN_POINT('Ctrl Pts',(1.05760163192479,-1.,-1.7150865442702));
#20440=CARTESIAN_POINT('Ctrl Pts',(1.06247324680647,-1.,-1.71874858456904));
#20441=CARTESIAN_POINT('Ctrl Pts',(1.06738966975462,-1.,-1.72238500928453));
#20442=CARTESIAN_POINT('Ctrl Pts',(1.07234866990252,-1.,-1.72599406198488));
#20443=CARTESIAN_POINT('Ctrl Pts',(1.0773470373727,-1.,-1.72957248977424));
#20444=CARTESIAN_POINT('Ctrl Pts',(1.08238162784749,-1.,-1.73311705663407));
#20445=CARTESIAN_POINT('Ctrl Pts',(1.08745056285427,-1.,-1.73662628326091));
#20446=CARTESIAN_POINT('Ctrl Pts',(1.09255329056493,-1.,-1.74010053962247));
#20447=CARTESIAN_POINT('Ctrl Pts',(1.09768999241225,-1.,-1.74354119236208));
#20448=CARTESIAN_POINT('Ctrl Pts',(1.10286118991143,-1.,-1.74695004214923));
#20449=CARTESIAN_POINT('Ctrl Pts',(1.10806728183007,-1.,-1.7503286607592));
#20450=CARTESIAN_POINT('Ctrl Pts',(1.11330807582551,-1.,-1.7536777209463));
#20451=CARTESIAN_POINT('Ctrl Pts',(1.11858293216763,-1.,-1.75699720772105));
#20452=CARTESIAN_POINT('Ctrl Pts',(1.12389096855086,-1.,-1.76028671825096));
#20453=CARTESIAN_POINT('Ctrl Pts',(1.12923123555075,-1.,-1.7635457196617));
#20454=CARTESIAN_POINT('Ctrl Pts',(1.1346029180462,-1.,-1.76677384551862));
#20455=CARTESIAN_POINT('Ctrl Pts',(1.14000548336975,-1.,-1.76997111386769));
#20456=CARTESIAN_POINT('Ctrl Pts',(1.1454385822692,-1.,-1.77313777896194));
#20457=CARTESIAN_POINT('Ctrl Pts',(1.15090197841514,-1.,-1.7762742255701));
#20458=CARTESIAN_POINT('Ctrl Pts',(1.15639547194698,-1.,-1.77938085564275));
#20459=CARTESIAN_POINT('Ctrl Pts',(1.16191881298499,-1.,-1.78245795881009));
#20460=CARTESIAN_POINT('Ctrl Pts',(1.16747166312303,-1.,-1.78550566040443));
#20461=CARTESIAN_POINT('Ctrl Pts',(1.17305363177328,-1.,-1.78852398877617));
#20462=CARTESIAN_POINT('Ctrl Pts',(1.17866429440809,-1.,-1.79151291552689));
#20463=CARTESIAN_POINT('Ctrl Pts',(1.18430321697432,-1.,-1.79447240321515));
#20464=CARTESIAN_POINT('Ctrl Pts',(1.18996997934445,-1.,-1.79740245923478));
#20465=CARTESIAN_POINT('Ctrl Pts',(1.19566418930242,-1.,-1.80030314369879));
#20466=CARTESIAN_POINT('Ctrl Pts',(1.20138548938974,-1.,-1.80317454838603));
#20467=CARTESIAN_POINT('Ctrl Pts',(1.20713356605475,-1.,-1.80601678480707));
#20468=CARTESIAN_POINT('Ctrl Pts',(1.21290815708314,-1.,-1.80882996917129));
#20469=CARTESIAN_POINT('Ctrl Pts',(1.21870906103557,-1.,-1.81161420806656));
#20470=CARTESIAN_POINT('Ctrl Pts',(1.2245361330495,-1.,-1.81436959210434));
#20471=CARTESIAN_POINT('Ctrl Pts',(1.2292186489137,-1.,-1.8165508718364));
#20472=CARTESIAN_POINT('Ctrl Pts',(1.2327422452705,-1.,-1.81817389921279));
#20473=CARTESIAN_POINT('Ctrl Pts',(1.23509651170476,-1.,-1.81925017193666));
#20474=CARTESIAN_POINT('Ctrl Pts',(1.23627494547115,-1.,-1.81978687191668));
#20475=CARTESIAN_POINT('',(1.34869019493419,-1.,-1.73811241238545));
#20476=CARTESIAN_POINT('',(1.23627494547115,-1.,-1.81978687191668));
#20477=CARTESIAN_POINT('',(1.15624053661742,-1.,-1.31362392696032));
#20478=CARTESIAN_POINT('Ctrl Pts',(1.34869019493419,-1.,-1.73811241238545));
#20479=CARTESIAN_POINT('Ctrl Pts',(1.34854391898045,-1.,-1.73682580585691));
#20480=CARTESIAN_POINT('Ctrl Pts',(1.34824783112887,-1.,-1.73425417885907));
#20481=CARTESIAN_POINT('Ctrl Pts',(1.34779309152035,-1.,-1.7304014965394));
#20482=CARTESIAN_POINT('Ctrl Pts',(1.34716554819527,-1.,-1.72527410680674));
#20483=CARTESIAN_POINT('Ctrl Pts',(1.34634568653227,-1.,-1.7188807715049));
#20484=CARTESIAN_POINT('Ctrl Pts',(1.34549029589416,-1.,-1.71250340686822));
#20485=CARTESIAN_POINT('Ctrl Pts',(1.34459924533831,-1.,-1.70614212266738));
#20486=CARTESIAN_POINT('Ctrl Pts',(1.34367237124483,-1.,-1.69979707754427));
#20487=CARTESIAN_POINT('Ctrl Pts',(1.34270948206319,-1.,-1.6934684849687));
#20488=CARTESIAN_POINT('Ctrl Pts',(1.341710374848,-1.,-1.68715660868764));
#20489=CARTESIAN_POINT('Ctrl Pts',(1.34067485185203,-1.,-1.68086176030362));
#20490=CARTESIAN_POINT('Ctrl Pts',(1.3396027347034,-1.,-1.67458429426086));
#20491=CARTESIAN_POINT('Ctrl Pts',(1.33849388654388,-1.,-1.66832460783989));
#20492=CARTESIAN_POINT('Ctrl Pts',(1.33734820885262,-1.,-1.66208312541983));
#20493=CARTESIAN_POINT('Ctrl Pts',(1.33616559745172,-1.,-1.65586025952593));
#20494=CARTESIAN_POINT('Ctrl Pts',(1.33494590467993,-1.,-1.6496563728683));
#20495=CARTESIAN_POINT('Ctrl Pts',(1.33368890676572,-1.,-1.6434717485603));
#20496=CARTESIAN_POINT('Ctrl Pts',(1.33239425103724,-1.,-1.63730653475089));
#20497=CARTESIAN_POINT('Ctrl Pts',(1.33106149345645,-1.,-1.63116079730923));
#20498=CARTESIAN_POINT('Ctrl Pts',(1.3296901950568,-1.,-1.62503464209797));
#20499=CARTESIAN_POINT('Ctrl Pts',(1.32828000610449,-1.,-1.61892832270724));
#20500=CARTESIAN_POINT('Ctrl Pts',(1.32683074483356,-1.,-1.6128423401575));
#20501=CARTESIAN_POINT('Ctrl Pts',(1.32534250785782,-1.,-1.60677758290954));
#20502=CARTESIAN_POINT('Ctrl Pts',(1.32381550858256,-1.,-1.60073511858687));
#20503=CARTESIAN_POINT('Ctrl Pts',(1.32224985747682,-1.,-1.59471591079403));
#20504=CARTESIAN_POINT('Ctrl Pts',(1.32064537110892,-1.,-1.58872057258245));
#20505=CARTESIAN_POINT('Ctrl Pts',(1.31900135021432,-1.,-1.58274907898834));
#20506=CARTESIAN_POINT('Ctrl Pts',(1.31731642317187,-1.,-1.5768005650559));
#20507=CARTESIAN_POINT('Ctrl Pts',(1.31558903860016,-1.,-1.57087397835723));
#20508=CARTESIAN_POINT('Ctrl Pts',(1.31381795281002,-1.,-1.56496872402353));
#20509=CARTESIAN_POINT('Ctrl Pts',(1.31200264341696,-1.,-1.55908521254821));
#20510=CARTESIAN_POINT('Ctrl Pts',(1.31014393684222,-1.,-1.55322568759481));
#20511=CARTESIAN_POINT('Ctrl Pts',(1.30824393907473,-1.,-1.54739413957185));
#20512=CARTESIAN_POINT('Ctrl Pts',(1.30630475189556,-1.,-1.54159462645432));
#20513=CARTESIAN_POINT('Ctrl Pts',(1.30432735639489,-1.,-1.53582981268977));
#20514=CARTESIAN_POINT('Ctrl Pts',(1.30231064395568,-1.,-1.53009970283891));
#20515=CARTESIAN_POINT('Ctrl Pts',(1.30024984366328,-1.,-1.52439957861062));
#20516=CARTESIAN_POINT('Ctrl Pts',(1.29813791800747,-1.,-1.51872184912724));
#20517=CARTESIAN_POINT('Ctrl Pts',(1.29596850710509,-1.,-1.51305994241402));
#20518=CARTESIAN_POINT('Ctrl Pts',(1.29373841372842,-1.,-1.50741159078365));
#20519=CARTESIAN_POINT('Ctrl Pts',(1.29145022885181,-1.,-1.50178230149776));
#20520=CARTESIAN_POINT('Ctrl Pts',(1.28911506584254,-1.,-1.49618896881754));
#20521=CARTESIAN_POINT('Ctrl Pts',(1.2867467611644,-1.,-1.4906522831278));
#20522=CARTESIAN_POINT('Ctrl Pts',(1.28435533880201,-1.,-1.4851881711891));
#20523=CARTESIAN_POINT('Ctrl Pts',(1.28194158939517,-1.,-1.47980070347096));
#20524=CARTESIAN_POINT('Ctrl Pts',(1.2794891824849,-1.,-1.4744717526707));
#20525=CARTESIAN_POINT('Ctrl Pts',(1.27696414831089,-1.,-1.46916035917133));
#20526=CARTESIAN_POINT('Ctrl Pts',(1.27433119897822,-1.,-1.46382431332476));
#20527=CARTESIAN_POINT('Ctrl Pts',(1.27156805265289,-1.,-1.45843906294697));
#20528=CARTESIAN_POINT('Ctrl Pts',(1.2686778680489,-1.,-1.45301422764247));
#20529=CARTESIAN_POINT('Ctrl Pts',(1.26570925118868,-1.,-1.44761985001662));
#20530=CARTESIAN_POINT('Ctrl Pts',(1.26273903323858,-1.,-1.44236470511303));
#20531=CARTESIAN_POINT('Ctrl Pts',(1.25983531012005,-1.,-1.43734919180848));
#20532=CARTESIAN_POINT('Ctrl Pts',(1.25702687965755,-1.,-1.43262645609691));
#20533=CARTESIAN_POINT('Ctrl Pts',(1.25426945222639,-1.,-1.42815938799387));
#20534=CARTESIAN_POINT('Ctrl Pts',(1.2514145557001,-1.,-1.42378102115575));
#20535=CARTESIAN_POINT('Ctrl Pts',(1.24824430986571,-1.,-1.41923722596025));
#20536=CARTESIAN_POINT('Ctrl Pts',(1.24450600513056,-1.,-1.41422913175179));
#20537=CARTESIAN_POINT('Ctrl Pts',(1.23994455029534,-1.,-1.40845295531283));
#20538=CARTESIAN_POINT('Ctrl Pts',(1.23434087290423,-1.,-1.40164708206106));
#20539=CARTESIAN_POINT('Ctrl Pts',(1.22752961899387,-1.,-1.39361389568796));
#20540=CARTESIAN_POINT('Ctrl Pts',(1.21938737280852,-1.,-1.38420564527715));
#20541=CARTESIAN_POINT('Ctrl Pts',(1.20982812925645,-1.,-1.37331915607905));
#20542=CARTESIAN_POINT('Ctrl Pts',(1.1987959077932,-1.,-1.36088705043885));
#20543=CARTESIAN_POINT('Ctrl Pts',(1.18625865667441,-1.,-1.34687054001093));
#20544=CARTESIAN_POINT('Ctrl Pts',(1.17501305789857,-1.,-1.33437539347008));
#20545=CARTESIAN_POINT('Ctrl Pts',(1.16589330093588,-1.,-1.32428080721772));
#20546=CARTESIAN_POINT('Ctrl Pts',(1.15950888730809,-1.,-1.31722977216397));
#20547=CARTESIAN_POINT('Ctrl Pts',(1.15624053661742,-1.,-1.31362392696032));
#20548=CARTESIAN_POINT('',(1.31362392696032,-1.,-1.15624053661742));
#20549=CARTESIAN_POINT('Origin',(0.,-1.,0.));
#20550=CARTESIAN_POINT('',(1.73811241238545,-1.,-1.34869019493419));
#20551=CARTESIAN_POINT('Ctrl Pts',(1.31362392696032,-1.,-1.15624053661742));
#20552=CARTESIAN_POINT('Ctrl Pts',(1.3172297721596,-1.,-1.15950888730433));
#20553=CARTESIAN_POINT('Ctrl Pts',(1.32428080720544,-1.,-1.16589330092532));
#20554=CARTESIAN_POINT('Ctrl Pts',(1.33437539344842,-1.,-1.17501305787994));
#20555=CARTESIAN_POINT('Ctrl Pts',(1.34687053998157,-1.,-1.18625865664915));
#20556=CARTESIAN_POINT('Ctrl Pts',(1.36088705040677,-1.,-1.1987959077656));
#20557=CARTESIAN_POINT('Ctrl Pts',(1.37331915604962,-1.,-1.20982812923113));
#20558=CARTESIAN_POINT('Ctrl Pts',(1.38420564525391,-1.,-1.21938737278853));
#20559=CARTESIAN_POINT('Ctrl Pts',(1.39361389567257,-1.,-1.22752961898063));
#20560=CARTESIAN_POINT('Ctrl Pts',(1.40164708205345,-1.,-1.23434087289768));
#20561=CARTESIAN_POINT('Ctrl Pts',(1.40845295531151,-1.,-1.23994455029421));
#20562=CARTESIAN_POINT('Ctrl Pts',(1.41422913175437,-1.,-1.24450600513278));
#20563=CARTESIAN_POINT('Ctrl Pts',(1.41923722596421,-1.,-1.24824430986911));
#20564=CARTESIAN_POINT('Ctrl Pts',(1.42378102115911,-1.,-1.25141455570299));
#20565=CARTESIAN_POINT('Ctrl Pts',(1.42815938799555,-1.,-1.25426945222783));
#20566=CARTESIAN_POINT('Ctrl Pts',(1.43262645609679,-1.,-1.25702687965744));
#20567=CARTESIAN_POINT('Ctrl Pts',(1.43734919180719,-1.,-1.25983531011894));
#20568=CARTESIAN_POINT('Ctrl Pts',(1.44236470511145,-1.,-1.26273903323723));
#20569=CARTESIAN_POINT('Ctrl Pts',(1.44761985001544,-1.,-1.26570925118767));
#20570=CARTESIAN_POINT('Ctrl Pts',(1.45301422764205,-1.,-1.26867786804854));
#20571=CARTESIAN_POINT('Ctrl Pts',(1.45843906294725,-1.,-1.27156805265312));
#20572=CARTESIAN_POINT('Ctrl Pts',(1.4638243133254,-1.,-1.27433119897877));
#20573=CARTESIAN_POINT('Ctrl Pts',(1.46916035917197,-1.,-1.27696414831144));
#20574=CARTESIAN_POINT('Ctrl Pts',(1.4744717526711,-1.,-1.27948918248524));
#20575=CARTESIAN_POINT('Ctrl Pts',(1.47980070347102,-1.,-1.28194158939522));
#20576=CARTESIAN_POINT('Ctrl Pts',(1.48518817118891,-1.,-1.28435533880184));
#20577=CARTESIAN_POINT('Ctrl Pts',(1.4906522831275,-1.,-1.28674676116415));
#20578=CARTESIAN_POINT('Ctrl Pts',(1.49618896881729,-1.,-1.28911506584232));
#20579=CARTESIAN_POINT('Ctrl Pts',(1.50178230149764,-1.,-1.29145022885171));
#20580=CARTESIAN_POINT('Ctrl Pts',(1.50741159078367,-1.,-1.29373841372843));
#20581=CARTESIAN_POINT('Ctrl Pts',(1.51305994241412,-1.,-1.29596850710518));
#20582=CARTESIAN_POINT('Ctrl Pts',(1.51872184912735,-1.,-1.29813791800757));
#20583=CARTESIAN_POINT('Ctrl Pts',(1.5243995786107,-1.,-1.30024984366334));
#20584=CARTESIAN_POINT('Ctrl Pts',(1.53009970283893,-1.,-1.3023106439557));
#20585=CARTESIAN_POINT('Ctrl Pts',(1.53582981268976,-1.,-1.30432735639487));
#20586=CARTESIAN_POINT('Ctrl Pts',(1.54159462645428,-1.,-1.30630475189553));
#20587=CARTESIAN_POINT('Ctrl Pts',(1.54739413957183,-1.,-1.30824393907471));
#20588=CARTESIAN_POINT('Ctrl Pts',(1.55322568759481,-1.,-1.31014393684221));
#20589=CARTESIAN_POINT('Ctrl Pts',(1.55908521254822,-1.,-1.31200264341696));
#20590=CARTESIAN_POINT('Ctrl Pts',(1.56496872402352,-1.,-1.31381795281002));
#20591=CARTESIAN_POINT('Ctrl Pts',(1.57087397835721,-1.,-1.31558903860015));
#20592=CARTESIAN_POINT('Ctrl Pts',(1.57680056505585,-1.,-1.31731642317183));
#20593=CARTESIAN_POINT('Ctrl Pts',(1.58274907898829,-1.,-1.31900135021428));
#20594=CARTESIAN_POINT('Ctrl Pts',(1.58872057258244,-1.,-1.32064537110891));
#20595=CARTESIAN_POINT('Ctrl Pts',(1.59471591079408,-1.,-1.32224985747686));
#20596=CARTESIAN_POINT('Ctrl Pts',(1.600735118587,-1.,-1.32381550858266));
#20597=CARTESIAN_POINT('Ctrl Pts',(1.6067775829097,-1.,-1.32534250785794));
#20598=CARTESIAN_POINT('Ctrl Pts',(1.61284234015762,-1.,-1.32683074483365));
#20599=CARTESIAN_POINT('Ctrl Pts',(1.61892832270723,-1.,-1.32828000610448));
#20600=CARTESIAN_POINT('Ctrl Pts',(1.62503464209777,-1.,-1.32969019505665));
#20601=CARTESIAN_POINT('Ctrl Pts',(1.63116079730887,-1.,-1.33106149345618));
#20602=CARTESIAN_POINT('Ctrl Pts',(1.63730653475049,-1.,-1.33239425103694));
#20603=CARTESIAN_POINT('Ctrl Pts',(1.64347174856007,-1.,-1.33368890676554));
#20604=CARTESIAN_POINT('Ctrl Pts',(1.64965637286843,-1.,-1.33494590468003));
#20605=CARTESIAN_POINT('Ctrl Pts',(1.65586025952651,-1.,-1.33616559745217));
#20606=CARTESIAN_POINT('Ctrl Pts',(1.66208312542073,-1.,-1.33734820885331));
#20607=CARTESIAN_POINT('Ctrl Pts',(1.66832460784078,-1.,-1.33849388654458));
#20608=CARTESIAN_POINT('Ctrl Pts',(1.67458429426126,-1.,-1.33960273470372));
#20609=CARTESIAN_POINT('Ctrl Pts',(1.68086176030308,-1.,-1.3406748518516));
#20610=CARTESIAN_POINT('Ctrl Pts',(1.68715660868602,-1.,-1.34171037484673));
#20611=CARTESIAN_POINT('Ctrl Pts',(1.6934684849664,-1.,-1.34270948206139));
#20612=CARTESIAN_POINT('Ctrl Pts',(1.69979707754221,-1.,-1.34367237124322));
#20613=CARTESIAN_POINT('Ctrl Pts',(1.70614212266676,-1.,-1.34459924533783));
#20614=CARTESIAN_POINT('Ctrl Pts',(1.71250340687011,-1.,-1.34549029589563));
#20615=CARTESIAN_POINT('Ctrl Pts',(1.7188807715095,-1.,-1.34634568653586));
#20616=CARTESIAN_POINT('Ctrl Pts',(1.72527410681298,-1.,-1.34716554820013));
#20617=CARTESIAN_POINT('Ctrl Pts',(1.73040149654497,-1.,-1.3477930915247));
#20618=CARTESIAN_POINT('Ctrl Pts',(1.73425417886254,-1.,-1.34824783113158));
#20619=CARTESIAN_POINT('Ctrl Pts',(1.73682580585819,-1.,-1.34854391898145));
#20620=CARTESIAN_POINT('Ctrl Pts',(1.73811241238545,-1.,-1.34869019493419));
#20621=CARTESIAN_POINT('',(1.81978687191668,-1.,-1.23627494547115));
#20622=CARTESIAN_POINT('',(1.73811241238545,-1.,-1.34869019493419));
#20623=CARTESIAN_POINT('',(1.5055822144029,-1.,-0.892032620296855));
#20624=CARTESIAN_POINT('Ctrl Pts',(1.81978687191668,-1.,-1.23627494547115));
#20625=CARTESIAN_POINT('Ctrl Pts',(1.81925017193531,-1.,-1.23509651170384));
#20626=CARTESIAN_POINT('Ctrl Pts',(1.81817389920914,-1.,-1.23274224526804));
#20627=CARTESIAN_POINT('Ctrl Pts',(1.81655087183054,-1.,-1.22921864890975));
#20628=CARTESIAN_POINT('Ctrl Pts',(1.81436959209778,-1.,-1.22453613304507));
#20629=CARTESIAN_POINT('Ctrl Pts',(1.81161420806172,-1.,-1.2187090610323));
#20630=CARTESIAN_POINT('Ctrl Pts',(1.80882996916931,-1.,-1.2129081570818));
#20631=CARTESIAN_POINT('Ctrl Pts',(1.80601678480772,-1.,-1.20713356605519));
#20632=CARTESIAN_POINT('Ctrl Pts',(1.8031745483882,-1.,-1.2013854893912));
#20633=CARTESIAN_POINT('Ctrl Pts',(1.80030314370121,-1.,-1.19566418930405));
#20634=CARTESIAN_POINT('Ctrl Pts',(1.79740245923649,-1.,-1.1899699793456));
#20635=CARTESIAN_POINT('Ctrl Pts',(1.79447240321572,-1.,-1.18430321697471));
#20636=CARTESIAN_POINT('Ctrl Pts',(1.79151291552646,-1.,-1.17866429440781));
#20637=CARTESIAN_POINT('Ctrl Pts',(1.78852398877523,-1.,-1.17305363177265));
#20638=CARTESIAN_POINT('Ctrl Pts',(1.78550566040349,-1.,-1.16747166312239));
#20639=CARTESIAN_POINT('Ctrl Pts',(1.78245795880949,-1.,-1.16191881298458));
#20640=CARTESIAN_POINT('Ctrl Pts',(1.77938085564261,-1.,-1.15639547194689));
#20641=CARTESIAN_POINT('Ctrl Pts',(1.77627422557034,-1.,-1.15090197841531));
#20642=CARTESIAN_POINT('Ctrl Pts',(1.77313777896234,-1.,-1.14543858226948));
#20643=CARTESIAN_POINT('Ctrl Pts',(1.76997111386806,-1.,-1.14000548337));
#20644=CARTESIAN_POINT('Ctrl Pts',(1.76677384551883,-1.,-1.13460291804635));
#20645=CARTESIAN_POINT('Ctrl Pts',(1.76354571966171,-1.,-1.12923123555076));
#20646=CARTESIAN_POINT('Ctrl Pts',(1.76028671825084,-1.,-1.12389096855078));
#20647=CARTESIAN_POINT('Ctrl Pts',(1.75699720772089,-1.,-1.11858293216752));
#20648=CARTESIAN_POINT('Ctrl Pts',(1.75367772094617,-1.,-1.11330807582542));
#20649=CARTESIAN_POINT('Ctrl Pts',(1.75032866075914,-1.,-1.10806728183003));
#20650=CARTESIAN_POINT('Ctrl Pts',(1.74695004214924,-1.,-1.10286118991144));
#20651=CARTESIAN_POINT('Ctrl Pts',(1.74354119236212,-1.,-1.09768999241229));
#20652=CARTESIAN_POINT('Ctrl Pts',(1.74010053962252,-1.,-1.09255329056496));
#20653=CARTESIAN_POINT('Ctrl Pts',(1.73662628326093,-1.,-1.08745056285429));
#20654=CARTESIAN_POINT('Ctrl Pts',(1.73311705663407,-1.,-1.08238162784749));
#20655=CARTESIAN_POINT('Ctrl Pts',(1.72957248977424,-1.,-1.0773470373727));
#20656=CARTESIAN_POINT('Ctrl Pts',(1.72599406198489,-1.,-1.07234866990252));
#20657=CARTESIAN_POINT('Ctrl Pts',(1.72238500928456,-1.,-1.06738966975463));
#20658=CARTESIAN_POINT('Ctrl Pts',(1.71874858456908,-1.,-1.0624732468065));
#20659=CARTESIAN_POINT('Ctrl Pts',(1.71508654427022,-1.,-1.05760163192481));
#20660=CARTESIAN_POINT('Ctrl Pts',(1.71139783543986,-1.,-1.05277517202854));
#20661=CARTESIAN_POINT('Ctrl Pts',(1.70767646263641,-1.,-1.0479908540499));
#20662=CARTESIAN_POINT('Ctrl Pts',(1.70391338707969,-1.,-1.04324363334546));
#20663=CARTESIAN_POINT('Ctrl Pts',(1.70010052930951,-1.,-1.03852922490782));
#20664=CARTESIAN_POINT('Ctrl Pts',(1.69623414782769,-1.,-1.03384646003587));
#20665=CARTESIAN_POINT('Ctrl Pts',(1.69231840863471,-1.,-1.02919977579155));
#20666=CARTESIAN_POINT('Ctrl Pts',(1.68836910178475,-1.,-1.02460180535272));
#20667=CARTESIAN_POINT('Ctrl Pts',(1.68440578021739,-1.,-1.02006795074222));
#20668=CARTESIAN_POINT('Ctrl Pts',(1.6804428989482,-1.,-1.01561026162787));
#20669=CARTESIAN_POINT('Ctrl Pts',(1.67648246776457,-1.,-1.01123236493507));
#20670=CARTESIAN_POINT('Ctrl Pts',(1.67250335383248,-1.,-1.00692206696387));
#20671=CARTESIAN_POINT('Ctrl Pts',(1.66846059277231,-1.,-1.00265091003682));
#20672=CARTESIAN_POINT('Ctrl Pts',(1.66430758030304,-1.,-0.998389654952317));
#20673=CARTESIAN_POINT('Ctrl Pts',(1.66001553809916,-1.,-0.994121836661116));
#20674=CARTESIAN_POINT('Ctrl Pts',(1.65559044289746,-1.,-0.98985562785445));
#20675=CARTESIAN_POINT('Ctrl Pts',(1.6511001661277,-1.,-0.985642622921626));
#20676=CARTESIAN_POINT('Ctrl Pts',(1.64665139190834,-1.,-0.981562530940574));
#20677=CARTESIAN_POINT('Ctrl Pts',(1.64233990826831,-1.,-0.977689794120297));
#20678=CARTESIAN_POINT('Ctrl Pts',(1.63820952658157,-1.,-0.974066058287501));
#20679=CARTESIAN_POINT('Ctrl Pts',(1.63420665729609,-1.,-0.970669715996356));
#20680=CARTESIAN_POINT('Ctrl Pts',(1.63013849959083,-1.,-0.967387853228041));
#20681=CARTESIAN_POINT('Ctrl Pts',(1.6257193066974,-1.,-0.964046107037821));
#20682=CARTESIAN_POINT('Ctrl Pts',(1.62061638139929,-1.,-0.960438326099958));
#20683=CARTESIAN_POINT('Ctrl Pts',(1.61449324337233,-1.,-0.956354422921573));
#20684=CARTESIAN_POINT('Ctrl Pts',(1.60706069897794,-1.,-0.951613284361248));
#20685=CARTESIAN_POINT('Ctrl Pts',(1.59810042045408,-1.,-0.946078063325796));
#20686=CARTESIAN_POINT('Ctrl Pts',(1.58744937489796,-1.,-0.939646377909319));
#20687=CARTESIAN_POINT('Ctrl Pts',(1.57499388385561,-1.,-0.932246680128849));
#20688=CARTESIAN_POINT('Ctrl Pts',(1.56065988582509,-1.,-0.923832188966322));
#20689=CARTESIAN_POINT('Ctrl Pts',(1.54440491152807,-1.,-0.91437591904658));
#20690=CARTESIAN_POINT('Ctrl Pts',(1.52984849890434,-1.,-0.905967409640499));
#20691=CARTESIAN_POINT('Ctrl Pts',(1.51805569591479,-1.,-0.89918504749193));
#20692=CARTESIAN_POINT('Ctrl Pts',(1.50980486807181,-1.,-0.894452006967538));
#20693=CARTESIAN_POINT('Ctrl Pts',(1.5055822144029,-1.,-0.892032620296855));
#20694=CARTESIAN_POINT('',(1.60662857109684,-1.,-0.693717979106306));
#20695=CARTESIAN_POINT('Origin',(0.,-1.,0.));
#20696=CARTESIAN_POINT('',(2.0698113262342,-1.,-0.745574324794401));
#20697=CARTESIAN_POINT('Ctrl Pts',(1.60662857109684,-1.,-0.693717979106306));
#20698=CARTESIAN_POINT('Ctrl Pts',(1.61106790957619,-1.,-0.69571209787897));
#20699=CARTESIAN_POINT('Ctrl Pts',(1.61974673471117,-1.,-0.699605146398837));
#20700=CARTESIAN_POINT('Ctrl Pts',(1.6321654166204,-1.,-0.705159151977294));
#20701=CARTESIAN_POINT('Ctrl Pts',(1.64752408828442,-1.,-0.711993139340448));
#20702=CARTESIAN_POINT('Ctrl Pts',(1.66472880551777,-1.,-0.71958543378795));
#20703=CARTESIAN_POINT('Ctrl Pts',(1.67996158451922,-1.,-0.726235967982445));
#20704=CARTESIAN_POINT('Ctrl Pts',(1.69326921972915,-1.,-0.731963238685357));
#20705=CARTESIAN_POINT('Ctrl Pts',(1.70473309004249,-1.,-0.736799665716932));
#20706=CARTESIAN_POINT('Ctrl Pts',(1.71447789751001,-1.,-0.74079516202821));
#20707=CARTESIAN_POINT('Ctrl Pts',(1.72268229916769,-1.,-0.744021445433094));
#20708=CARTESIAN_POINT('Ctrl Pts',(1.72958533647714,-1.,-0.746574710097752));
#20709=CARTESIAN_POINT('Ctrl Pts',(1.7355035168033,-1.,-0.74858246295687));
#20710=CARTESIAN_POINT('Ctrl Pts',(1.74080458267114,-1.,-0.75019343598125));
#20711=CARTESIAN_POINT('Ctrl Pts',(1.74585086852502,-1.,-0.751555614164483));
#20712=CARTESIAN_POINT('Ctrl Pts',(1.75095139468794,-1.,-0.752797683531314));
#20713=CARTESIAN_POINT('Ctrl Pts',(1.75631083600019,-1.,-0.754009254027829));
#20714=CARTESIAN_POINT('Ctrl Pts',(1.76197817240128,-1.,-0.755220979974462));
#20715=CARTESIAN_POINT('Ctrl Pts',(1.76789396002998,-1.,-0.75642189602781));
#20716=CARTESIAN_POINT('Ctrl Pts',(1.77394167108292,-1.,-0.757578264077029));
#20717=CARTESIAN_POINT('Ctrl Pts',(1.77999411220945,-1.,-0.758650626677519));
#20718=CARTESIAN_POINT('Ctrl Pts',(1.78596964884604,-1.,-0.75961440111019));
#20719=CARTESIAN_POINT('Ctrl Pts',(1.7918581561088,-1.,-0.760469555880749));
#20720=CARTESIAN_POINT('Ctrl Pts',(1.79768986997783,-1.,-0.761229695230558));
#20721=CARTESIAN_POINT('Ctrl Pts',(1.80351583877342,-1.,-0.761915336443547));
#20722=CARTESIAN_POINT('Ctrl Pts',(1.80938551463965,-1.,-0.762546129463938));
#20723=CARTESIAN_POINT('Ctrl Pts',(1.8153211840553,-1.,-0.763132003836634));
#20724=CARTESIAN_POINT('Ctrl Pts',(1.82131873145266,-1.,-0.763673465462727));
#20725=CARTESIAN_POINT('Ctrl Pts',(1.82735991200065,-1.,-0.764165902605995));
#20726=CARTESIAN_POINT('Ctrl Pts',(1.83342077227142,-1.,-0.764602549687853));
#20727=CARTESIAN_POINT('Ctrl Pts',(1.83948181064835,-1.,-0.764978057881738));
#20728=CARTESIAN_POINT('Ctrl Pts',(1.84553698875924,-1.,-0.765291664862029));
#20729=CARTESIAN_POINT('Ctrl Pts',(1.85158945130063,-1.,-0.765545710619063));
#20730=CARTESIAN_POINT('Ctrl Pts',(1.85764741390394,-1.,-0.765744212909319));
#20731=CARTESIAN_POINT('Ctrl Pts',(1.86372027063312,-1.,-0.765891519092547));
#20732=CARTESIAN_POINT('Ctrl Pts',(1.86981398314341,-1.,-0.765990708546091));
#20733=CARTESIAN_POINT('Ctrl Pts',(1.87592888967883,-1.,-0.766042837036744));
#20734=CARTESIAN_POINT('Ctrl Pts',(1.88206215302561,-1.,-0.766047794851865));
#20735=CARTESIAN_POINT('Ctrl Pts',(1.88820926433409,-1.,-0.766004837062091));
#20736=CARTESIAN_POINT('Ctrl Pts',(1.89436577771388,-1.,-0.765913193856978));
#20737=CARTESIAN_POINT('Ctrl Pts',(1.90052930393596,-1.,-0.765772772593386));
#20738=CARTESIAN_POINT('Ctrl Pts',(1.90669961402356,-1.,-0.765584196937919));
#20739=CARTESIAN_POINT('Ctrl Pts',(1.91287765805169,-1.,-0.765348465884722));
#20740=CARTESIAN_POINT('Ctrl Pts',(1.91906491634196,-1.,-0.765066729667089));
#20741=CARTESIAN_POINT('Ctrl Pts',(1.92526263537048,-1.,-0.764740025488212));
#20742=CARTESIAN_POINT('Ctrl Pts',(1.93147105496382,-1.,-0.764369010673941));
#20743=CARTESIAN_POINT('Ctrl Pts',(1.93768964875886,-1.,-0.763954049121459));
#20744=CARTESIAN_POINT('Ctrl Pts',(1.9439174661764,-1.,-0.763495333538629));
#20745=CARTESIAN_POINT('Ctrl Pts',(1.95015342590024,-1.,-0.762992990878769));
#20746=CARTESIAN_POINT('Ctrl Pts',(1.95639665309869,-1.,-0.762447203806179));
#20747=CARTESIAN_POINT('Ctrl Pts',(1.96264672744186,-1.,-0.761858300014424));
#20748=CARTESIAN_POINT('Ctrl Pts',(1.96890351582499,-1.,-0.761226690483821));
#20749=CARTESIAN_POINT('Ctrl Pts',(1.97516705321494,-1.,-0.760552825409757));
#20750=CARTESIAN_POINT('Ctrl Pts',(1.98143741418172,-1.,-0.75983714745219));
#20751=CARTESIAN_POINT('Ctrl Pts',(1.98771456680874,-1.,-0.759080037802488));
#20752=CARTESIAN_POINT('Ctrl Pts',(1.99399831098817,-1.,-0.758281796766761));
#20753=CARTESIAN_POINT('Ctrl Pts',(2.00028834739178,-1.,-0.757442676862724));
#20754=CARTESIAN_POINT('Ctrl Pts',(2.0065843158773,-1.,-0.756562904646671));
#20755=CARTESIAN_POINT('Ctrl Pts',(2.01288584328084,-1.,-0.755642704957865));
#20756=CARTESIAN_POINT('Ctrl Pts',(2.01919259405809,-1.,-0.754682330722816));
#20757=CARTESIAN_POINT('Ctrl Pts',(2.02550428623313,-1.,-0.753682061112768));
#20758=CARTESIAN_POINT('Ctrl Pts',(2.03182068456221,-1.,-0.752642180487211));
#20759=CARTESIAN_POINT('Ctrl Pts',(2.03814160092099,-1.,-0.751562963361115));
#20760=CARTESIAN_POINT('Ctrl Pts',(2.04446689147979,-1.,-0.750444657875576));
#20761=CARTESIAN_POINT('Ctrl Pts',(2.05079645592154,-1.,-0.749287468665046));
#20762=CARTESIAN_POINT('Ctrl Pts',(2.05713023031006,-1.,-0.748091554183803));
#20763=CARTESIAN_POINT('Ctrl Pts',(2.06220058927826,-1.,-0.74710393278792));
#20764=CARTESIAN_POINT('Ctrl Pts',(2.06600523016815,-1.,-0.746345871544201));
#20765=CARTESIAN_POINT('Ctrl Pts',(2.06854248895728,-1.,-0.745832791378367));
#20766=CARTESIAN_POINT('Ctrl Pts',(2.0698113262342,-1.,-0.745574324794401));
#20767=CARTESIAN_POINT('',(2.11275013067528,-1.,-0.61342227326009));
#20768=CARTESIAN_POINT('',(2.0698113262342,-1.,-0.745574324794401));
#20769=CARTESIAN_POINT('',(1.7075470150345,-1.,-0.383122945602004));
#20770=CARTESIAN_POINT('Ctrl Pts',(2.11275013067528,-1.,-0.61342227326009));
#20771=CARTESIAN_POINT('Ctrl Pts',(2.11187554259986,-1.,-0.6124673655618));
#20772=CARTESIAN_POINT('Ctrl Pts',(2.11012443807238,-1.,-0.610560911689899));
#20773=CARTESIAN_POINT('Ctrl Pts',(2.1074919961518,-1.,-0.607711315454876));
#20774=CARTESIAN_POINT('Ctrl Pts',(2.10397049886949,-1.,-0.60393203073603));
#20775=CARTESIAN_POINT('Ctrl Pts',(2.0995493086477,-1.,-0.599241616420534));
#20776=CARTESIAN_POINT('Ctrl Pts',(2.0951087622027,-1.,-0.594585006052162));
#20777=CARTESIAN_POINT('Ctrl Pts',(2.09064881812129,-1.,-0.589962365403406));
#20778=CARTESIAN_POINT('Ctrl Pts',(2.08616943727951,-1.,-0.585373918991617));
#20779=CARTESIAN_POINT('Ctrl Pts',(2.08167059018418,-1.,-0.580819952108064));
#20780=CARTESIAN_POINT('Ctrl Pts',(2.07715226767559,-1.,-0.576300797416845));
#20781=CARTESIAN_POINT('Ctrl Pts',(2.07261449292824,-1.,-0.571816823242603));
#20782=CARTESIAN_POINT('Ctrl Pts',(2.06805732997334,-1.,-0.567368421181087));
#20783=CARTESIAN_POINT('Ctrl Pts',(2.06348090160589,-1.,-0.562955993082262));
#20784=CARTESIAN_POINT('Ctrl Pts',(2.05888537756462,-1.,-0.558579940185152));
#20785=CARTESIAN_POINT('Ctrl Pts',(2.05427091604413,-1.,-0.554240657463906));
#20786=CARTESIAN_POINT('Ctrl Pts',(2.04963761077958,-1.,-0.549938525150295));
#20787=CARTESIAN_POINT('Ctrl Pts',(2.04498544714588,-1.,-0.54567390381743));
#20788=CARTESIAN_POINT('Ctrl Pts',(2.04031422690527,-1.,-0.541447120615659));
#20789=CARTESIAN_POINT('Ctrl Pts',(2.03562362954037,-1.,-0.537258489833262));
#20790=CARTESIAN_POINT('Ctrl Pts',(2.03091336214426,-1.,-0.533108355132977));
#20791=CARTESIAN_POINT('Ctrl Pts',(2.0261832908329,-1.,-0.528997127241914));
#20792=CARTESIAN_POINT('Ctrl Pts',(2.02143356304698,-1.,-0.524925318333476));
#20793=CARTESIAN_POINT('Ctrl Pts',(2.01666477917286,-1.,-0.520893590399371));
#20794=CARTESIAN_POINT('Ctrl Pts',(2.01187773939242,-1.,-0.516902681728687));
#20795=CARTESIAN_POINT('Ctrl Pts',(2.00707309946949,-1.,-0.512953306961793));
#20796=CARTESIAN_POINT('Ctrl Pts',(2.00225107134734,-1.,-0.509046069886157));
#20797=CARTESIAN_POINT('Ctrl Pts',(1.99741107463572,-1.,-0.505181361323026));
#20798=CARTESIAN_POINT('Ctrl Pts',(1.99255149126155,-1.,-0.501359287727146));
#20799=CARTESIAN_POINT('Ctrl Pts',(1.98767044752932,-1.,-0.497579909545574));
#20800=CARTESIAN_POINT('Ctrl Pts',(1.98276658761821,-1.,-0.493843476541495));
#20801=CARTESIAN_POINT('Ctrl Pts',(1.97783973019229,-1.,-0.490150627860953));
#20802=CARTESIAN_POINT('Ctrl Pts',(1.97289186263272,-1.,-0.486502692907659));
#20803=CARTESIAN_POINT('Ctrl Pts',(1.96792703422362,-1.,-0.482901662120691));
#20804=CARTESIAN_POINT('Ctrl Pts',(1.96294933055943,-1.,-0.479349583074855));
#20805=CARTESIAN_POINT('Ctrl Pts',(1.95796111148177,-1.,-0.475848034683176));
#20806=CARTESIAN_POINT('Ctrl Pts',(1.95296148278133,-1.,-0.472397672264072));
#20807=CARTESIAN_POINT('Ctrl Pts',(1.94794381136514,-1.,-0.468997482913135));
#20808=CARTESIAN_POINT('Ctrl Pts',(1.9428979419619,-1.,-0.46564546202603));
#20809=CARTESIAN_POINT('Ctrl Pts',(1.93781486640821,-1.,-0.462340031009057));
#20810=CARTESIAN_POINT('Ctrl Pts',(1.93269066517934,-1.,-0.459081234547926));
#20811=CARTESIAN_POINT('Ctrl Pts',(1.92753067150476,-1.,-0.455872005174371));
#20812=CARTESIAN_POINT('Ctrl Pts',(1.92235380648502,-1.,-0.452719478359433));
#20813=CARTESIAN_POINT('Ctrl Pts',(1.91718342555755,-1.,-0.449632260106662));
#20814=CARTESIAN_POINT('Ctrl Pts',(1.9120369998112,-1.,-0.446617343485711));
#20815=CARTESIAN_POINT('Ctrl Pts',(1.90691756144898,-1.,-0.443677556849151));
#20816=CARTESIAN_POINT('Ctrl Pts',(1.90180124389086,-1.,-0.440807833704038));
#20817=CARTESIAN_POINT('Ctrl Pts',(1.89663648956466,-1.,-0.437995003948244));
#20818=CARTESIAN_POINT('Ctrl Pts',(1.89136993975504,-1.,-0.435225660963383));
#20819=CARTESIAN_POINT('Ctrl Pts',(1.88596913666793,-1.,-0.432493038548748));
#20820=CARTESIAN_POINT('Ctrl Pts',(1.88044229001832,-1.,-0.429803062482345));
#20821=CARTESIAN_POINT('Ctrl Pts',(1.87486989291484,-1.,-0.427183828519102));
#20822=CARTESIAN_POINT('Ctrl Pts',(1.86937803944323,-1.,-0.424678177291359));
#20823=CARTESIAN_POINT('Ctrl Pts',(1.86408083334028,-1.,-0.422327307418275));
#20824=CARTESIAN_POINT('Ctrl Pts',(1.85903281096686,-1.,-0.42015728797562));
#20825=CARTESIAN_POINT('Ctrl Pts',(1.85417632856234,-1.,-0.418164129143534));
#20826=CARTESIAN_POINT('Ctrl Pts',(1.84929312929882,-1.,-0.416300022038864));
#20827=CARTESIAN_POINT('Ctrl Pts',(1.8440575707371,-1.,-0.41448743825434));
#20828=CARTESIAN_POINT('Ctrl Pts',(1.83808953475839,-1.,-0.412633125322162));
#20829=CARTESIAN_POINT('Ctrl Pts',(1.83100408895216,-1.,-0.410641256301675));
#20830=CARTESIAN_POINT('Ctrl Pts',(1.8224702267854,-1.,-0.408428948108534));
#20831=CARTESIAN_POINT('Ctrl Pts',(1.81223801813988,-1.,-0.405933518411838));
#20832=CARTESIAN_POINT('Ctrl Pts',(1.80012077176221,-1.,-0.403107976170441));
#20833=CARTESIAN_POINT('Ctrl Pts',(1.78598826347533,-1.,-0.399919403783081));
#20834=CARTESIAN_POINT('Ctrl Pts',(1.7697556004756,-1.,-0.39634619612042));
#20835=CARTESIAN_POINT('Ctrl Pts',(1.75137405313962,-1.,-0.392375812294307));
#20836=CARTESIAN_POINT('Ctrl Pts',(1.7349317097561,-1.,-0.388877023509192));
#20837=CARTESIAN_POINT('Ctrl Pts',(1.72162022246158,-1.,-0.38607079032701));
#20838=CARTESIAN_POINT('Ctrl Pts',(1.71231062891958,-1.,-0.384119047315542));
#20839=CARTESIAN_POINT('Ctrl Pts',(1.7075470150345,-1.,-0.383122945602004));
#20840=CARTESIAN_POINT('',(1.74236521665491,-1.,-0.163289472382896));
#20841=CARTESIAN_POINT('Origin',(0.,-1.,0.));
#20842=CARTESIAN_POINT('',(2.19890268624765,-1.,-0.0694764450219582));
#20843=CARTESIAN_POINT('Ctrl Pts',(1.74236521665491,-1.,-0.163289472382896));
#20844=CARTESIAN_POINT('Ctrl Pts',(1.7472034950333,-1.,-0.163814161002002));
#20845=CARTESIAN_POINT('Ctrl Pts',(1.75666056638427,-1.,-0.164834765707159));
#20846=CARTESIAN_POINT('Ctrl Pts',(1.77018771684844,-1.,-0.1662793551464));
#20847=CARTESIAN_POINT('Ctrl Pts',(1.7869064998507,-1.,-0.168032772805197));
#20848=CARTESIAN_POINT('Ctrl Pts',(1.80561530629706,-1.,-0.169936923904608));
#20849=CARTESIAN_POINT('Ctrl Pts',(1.82215766811545,-1.,-0.171554770204119));
#20850=CARTESIAN_POINT('Ctrl Pts',(1.83658380527692,-1.,-0.1728894428919));
#20851=CARTESIAN_POINT('Ctrl Pts',(1.8489811319852,-1.,-0.173946627587732));
#20852=CARTESIAN_POINT('Ctrl Pts',(1.85948367088837,-1.,-0.17473525927603));
#20853=CARTESIAN_POINT('Ctrl Pts',(1.86828349694799,-1.,-0.175268337590758));
#20854=CARTESIAN_POINT('Ctrl Pts',(1.87563767773588,-1.,-0.175563480746485));
#20855=CARTESIAN_POINT('Ctrl Pts',(1.88188663145367,-1.,-0.175644148889699));
#20856=CARTESIAN_POINT('Ctrl Pts',(1.88742606273259,-1.,-0.175538155840648));
#20857=CARTESIAN_POINT('Ctrl Pts',(1.892646301985,-1.,-0.175274276190844));
#20858=CARTESIAN_POINT('Ctrl Pts',(1.89788101117132,-1.,-0.174879405091263));
#20859=CARTESIAN_POINT('Ctrl Pts',(1.90335253862834,-1.,-0.174375518661085));
#20860=CARTESIAN_POINT('Ctrl Pts',(1.90911693975267,-1.,-0.173776635257817));
#20861=CARTESIAN_POINT('Ctrl Pts',(1.91511429159527,-1.,-0.173090695383496));
#20862=CARTESIAN_POINT('Ctrl Pts',(1.9212233439798,-1.,-0.172321621259514));
#20863=CARTESIAN_POINT('Ctrl Pts',(1.92731093582036,-1.,-0.171471191532988));
#20864=CARTESIAN_POINT('Ctrl Pts',(1.93329183155539,-1.,-0.170541253116202));
#20865=CARTESIAN_POINT('Ctrl Pts',(1.93915639211581,-1.,-0.169534904817491));
#20866=CARTESIAN_POINT('Ctrl Pts',(1.94493757756931,-1.,-0.168455741607556));
#20867=CARTESIAN_POINT('Ctrl Pts',(1.95069027794294,-1.,-0.167307501784476));
#20868=CARTESIAN_POINT('Ctrl Pts',(1.9564675971873,-1.,-0.166093592002813));
#20869=CARTESIAN_POINT('Ctrl Pts',(1.96229379940136,-1.,-0.164816568920269));
#20870=CARTESIAN_POINT('Ctrl Pts',(1.96816512677967,-1.,-0.163478185457734));
#20871=CARTESIAN_POINT('Ctrl Pts',(1.97406280235188,-1.,-0.162079693556289));
#20872=CARTESIAN_POINT('Ctrl Pts',(1.97996195437559,-1.,-0.160622060784611));
#20873=CARTESIAN_POINT('Ctrl Pts',(1.98584238283292,-1.,-0.159106226437299));
#20874=CARTESIAN_POINT('Ctrl Pts',(1.99169810931908,-1.,-0.157533331459227));
#20875=CARTESIAN_POINT('Ctrl Pts',(1.99753284771497,-1.,-0.155904629548784));
#20876=CARTESIAN_POINT('Ctrl Pts',(2.00335565310543,-1.,-0.154221403049722));
#20877=CARTESIAN_POINT('Ctrl Pts',(2.00917680318424,-1.,-0.15248488362145));
#20878=CARTESIAN_POINT('Ctrl Pts',(2.01500291940238,-1.,-0.150696157673078));
#20879=CARTESIAN_POINT('Ctrl Pts',(2.02083464969894,-1.,-0.148856124775337));
#20880=CARTESIAN_POINT('Ctrl Pts',(2.02666926182017,-1.,-0.146965557332583));
#20881=CARTESIAN_POINT('Ctrl Pts',(2.03250223739942,-1.,-0.145025140186058));
#20882=CARTESIAN_POINT('Ctrl Pts',(2.03832911025912,-1.,-0.143035515058209));
#20883=CARTESIAN_POINT('Ctrl Pts',(2.04414757947916,-1.,-0.140997332152546));
#20884=CARTESIAN_POINT('Ctrl Pts',(2.04995762001328,-1.,-0.138911255368966));
#20885=CARTESIAN_POINT('Ctrl Pts',(2.05576044414264,-1.,-0.136777941218044));
#20886=CARTESIAN_POINT('Ctrl Pts',(2.06155781517842,-1.,-0.134598026192106));
#20887=CARTESIAN_POINT('Ctrl Pts',(2.06735123910326,-1.,-0.132372111547711));
#20888=CARTESIAN_POINT('Ctrl Pts',(2.07314114713063,-1.,-0.130100748328404));
#20889=CARTESIAN_POINT('Ctrl Pts',(2.07892715110987,-1.,-0.12778444527612));
#20890=CARTESIAN_POINT('Ctrl Pts',(2.08470840653643,-1.,-0.125423679412062));
#20891=CARTESIAN_POINT('Ctrl Pts',(2.09048392424825,-1.,-0.123018905621083));
#20892=CARTESIAN_POINT('Ctrl Pts',(2.0962529286773,-1.,-0.120570567965122));
#20893=CARTESIAN_POINT('Ctrl Pts',(2.102015121329,-1.,-0.118079107988356));
#20894=CARTESIAN_POINT('Ctrl Pts',(2.10777050261309,-1.,-0.115544957687927));
#20895=CARTESIAN_POINT('Ctrl Pts',(2.11351924490306,-1.,-0.112968534419737));
#20896=CARTESIAN_POINT('Ctrl Pts',(2.11926155590865,-1.,-0.110350236135025));
#20897=CARTESIAN_POINT('Ctrl Pts',(2.12499752307,-1.,-0.10769043523109));
#20898=CARTESIAN_POINT('Ctrl Pts',(2.13072704887293,-1.,-0.10498947915274));
#20899=CARTESIAN_POINT('Ctrl Pts',(2.13644992667165,-1.,-0.102247700556101));
#20900=CARTESIAN_POINT('Ctrl Pts',(2.14216588396025,-1.,-0.0994654261990917));
#20901=CARTESIAN_POINT('Ctrl Pts',(2.14787463531795,-1.,-0.096642985230546));
#20902=CARTESIAN_POINT('Ctrl Pts',(2.1535759397817,-1.,-0.0937807218867645));
#20903=CARTESIAN_POINT('Ctrl Pts',(2.15926961544516,-1.,-0.0908789888107267));
#20904=CARTESIAN_POINT('Ctrl Pts',(2.16495552645014,-1.,-0.0879381291386924));
#20905=CARTESIAN_POINT('Ctrl Pts',(2.17063357870952,-1.,-0.0849584620835374));
#20906=CARTESIAN_POINT('Ctrl Pts',(2.176303712113,-1.,-0.0819402680872767));
#20907=CARTESIAN_POINT('Ctrl Pts',(2.18196589448887,-1.,-0.0788837727685244));
#20908=CARTESIAN_POINT('Ctrl Pts',(2.1876201139953,-1.,-0.0757891465836149));
#20909=CARTESIAN_POINT('Ctrl Pts',(2.19213712013662,-1.,-0.0732830357306726));
#20910=CARTESIAN_POINT('Ctrl Pts',(2.19552129484002,-1.,-0.0713863779526155));
#20911=CARTESIAN_POINT('Ctrl Pts',(2.19777582085423,-1.,-0.0701143536325491));
#20912=CARTESIAN_POINT('Ctrl Pts',(2.19890268624765,-1.,-0.0694764450219582));
#20913=CARTESIAN_POINT('',(2.19890268624765,-1.,0.0694764450219582));
#20914=CARTESIAN_POINT('',(2.19890268624765,-1.,-0.0694764450219582));
#20915=CARTESIAN_POINT('',(1.74236521665491,-1.,0.163289472382896));
#20916=CARTESIAN_POINT('Ctrl Pts',(2.19890268624765,-1.,0.0694764450219582));
#20917=CARTESIAN_POINT('Ctrl Pts',(2.19777582085261,-1.,0.0701143536324925));
#20918=CARTESIAN_POINT('Ctrl Pts',(2.19552129483562,-1.,0.0713863779524626));
#20919=CARTESIAN_POINT('Ctrl Pts',(2.19213712012956,-1.,0.0732830357304275));
#20920=CARTESIAN_POINT('Ctrl Pts',(2.1876201139874,-1.,0.075789146583341));
#20921=CARTESIAN_POINT('Ctrl Pts',(2.18196589448304,-1.,0.0788837727683226));
#20922=CARTESIAN_POINT('Ctrl Pts',(2.1763037121106,-1.,0.0819402680871938));
#20923=CARTESIAN_POINT('Ctrl Pts',(2.17063357871031,-1.,0.0849584620835642));
#20924=CARTESIAN_POINT('Ctrl Pts',(2.16495552645275,-1.,0.0879381291387821));
#20925=CARTESIAN_POINT('Ctrl Pts',(2.15926961544808,-1.,0.0908789888108265));
#20926=CARTESIAN_POINT('Ctrl Pts',(2.15357593978377,-1.,0.0937807218868344));
#20927=CARTESIAN_POINT('Ctrl Pts',(2.14787463531864,-1.,0.0966429852305688));
#20928=CARTESIAN_POINT('Ctrl Pts',(2.14216588395974,-1.,0.0994654261990741));
#20929=CARTESIAN_POINT('Ctrl Pts',(2.13644992667052,-1.,0.102247700556063));
#20930=CARTESIAN_POINT('Ctrl Pts',(2.1307270488718,-1.,0.104989479152703));
#20931=CARTESIAN_POINT('Ctrl Pts',(2.12499752306927,-1.,0.107690435231068));
#20932=CARTESIAN_POINT('Ctrl Pts',(2.11926155590849,-1.,0.11035023613502));
#20933=CARTESIAN_POINT('Ctrl Pts',(2.11351924490335,-1.,0.112968534419746));
#20934=CARTESIAN_POINT('Ctrl Pts',(2.10777050261359,-1.,0.11554495768794));
#20935=CARTESIAN_POINT('Ctrl Pts',(2.10201512132945,-1.,0.118079107988368));
#20936=CARTESIAN_POINT('Ctrl Pts',(2.09625292867756,-1.,0.120570567965129));
#20937=CARTESIAN_POINT('Ctrl Pts',(2.09048392424826,-1.,0.123018905621083));
#20938=CARTESIAN_POINT('Ctrl Pts',(2.08470840653628,-1.,0.125423679412058));
#20939=CARTESIAN_POINT('Ctrl Pts',(2.07892715110967,-1.,0.127784445276116));
#20940=CARTESIAN_POINT('Ctrl Pts',(2.07314114713047,-1.,0.1301007483284));
#20941=CARTESIAN_POINT('Ctrl Pts',(2.06735123910319,-1.,0.132372111547709));
#20942=CARTESIAN_POINT('Ctrl Pts',(2.06155781517844,-1.,0.134598026192107));
#20943=CARTESIAN_POINT('Ctrl Pts',(2.0557604441427,-1.,0.136777941218044));
#20944=CARTESIAN_POINT('Ctrl Pts',(2.04995762001333,-1.,0.138911255368966));
#20945=CARTESIAN_POINT('Ctrl Pts',(2.04414757947919,-1.,0.140997332152545));
#20946=CARTESIAN_POINT('Ctrl Pts',(2.03832911025913,-1.,0.143035515058208));
#20947=CARTESIAN_POINT('Ctrl Pts',(2.03250223739941,-1.,0.145025140186058));
#20948=CARTESIAN_POINT('Ctrl Pts',(2.02666926182017,-1.,0.146965557332586));
#20949=CARTESIAN_POINT('Ctrl Pts',(2.02083464969897,-1.,0.148856124775342));
#20950=CARTESIAN_POINT('Ctrl Pts',(2.01500291940243,-1.,0.150696157673084));
#20951=CARTESIAN_POINT('Ctrl Pts',(2.00917680318426,-1.,0.152484883621452));
#20952=CARTESIAN_POINT('Ctrl Pts',(2.00335565310539,-1.,0.154221403049719));
#20953=CARTESIAN_POINT('Ctrl Pts',(1.99753284771487,-1.,0.155904629548774));
#20954=CARTESIAN_POINT('Ctrl Pts',(1.99169810931893,-1.,0.157533331459215));
#20955=CARTESIAN_POINT('Ctrl Pts',(1.98584238283279,-1.,0.159106226437288));
#20956=CARTESIAN_POINT('Ctrl Pts',(1.97996195437557,-1.,0.16062206078461));
#20957=CARTESIAN_POINT('Ctrl Pts',(1.97406280235204,-1.,0.162079693556302));
#20958=CARTESIAN_POINT('Ctrl Pts',(1.96816512678,-1.,0.16347818545776));
#20959=CARTESIAN_POINT('Ctrl Pts',(1.96229379940174,-1.,0.1648165689203));
#20960=CARTESIAN_POINT('Ctrl Pts',(1.95646759718755,-1.,0.166093592002832));
#20961=CARTESIAN_POINT('Ctrl Pts',(1.95069027794286,-1.,0.167307501784469));
#20962=CARTESIAN_POINT('Ctrl Pts',(1.94493757756879,-1.,0.168455741607515));
#20963=CARTESIAN_POINT('Ctrl Pts',(1.93915639211497,-1.,0.169534904817425));
#20964=CARTESIAN_POINT('Ctrl Pts',(1.93329183155455,-1.,0.170541253116136));
#20965=CARTESIAN_POINT('Ctrl Pts',(1.92731093582,-1.,0.17147119153296));
#20966=CARTESIAN_POINT('Ctrl Pts',(1.92122334398034,-1.,0.172321621259556));
#20967=CARTESIAN_POINT('Ctrl Pts',(1.91511429159681,-1.,0.173090695383619));
#20968=CARTESIAN_POINT('Ctrl Pts',(1.90911693975475,-1.,0.173776635257983));
#20969=CARTESIAN_POINT('Ctrl Pts',(1.90335253863003,-1.,0.174375518661222));
#20970=CARTESIAN_POINT('Ctrl Pts',(1.89788101117148,-1.,0.174879405091277));
#20971=CARTESIAN_POINT('Ctrl Pts',(1.89264630198279,-1.,0.175274276190664));
#20972=CARTESIAN_POINT('Ctrl Pts',(1.88742606272818,-1.,0.175538155840286));
#20973=CARTESIAN_POINT('Ctrl Pts',(1.88188663144846,-1.,0.175644148889271));
#20974=CARTESIAN_POINT('Ctrl Pts',(1.87563767773249,-1.,0.175563480746205));
#20975=CARTESIAN_POINT('Ctrl Pts',(1.86828349694972,-1.,0.1752683375909));
#20976=CARTESIAN_POINT('Ctrl Pts',(1.85948367089838,-1.,0.174735259276856));
#20977=CARTESIAN_POINT('Ctrl Pts',(1.84898113200543,-1.,0.173946627589401));
#20978=CARTESIAN_POINT('Ctrl Pts',(1.83658380530747,-1.,0.17288944289442));
#20979=CARTESIAN_POINT('Ctrl Pts',(1.82215766815414,-1.,0.171554770207306));
#20980=CARTESIAN_POINT('Ctrl Pts',(1.80561530633924,-1.,0.169936923908078));
#20981=CARTESIAN_POINT('Ctrl Pts',(1.78690649988931,-1.,0.16803277280837));
#20982=CARTESIAN_POINT('Ctrl Pts',(1.77018771687692,-1.,0.166279355148738));
#20983=CARTESIAN_POINT('Ctrl Pts',(1.75666056640041,-1.,0.164834765708484));
#20984=CARTESIAN_POINT('Ctrl Pts',(1.74720349503904,-1.,0.163814161002474));
#20985=CARTESIAN_POINT('Ctrl Pts',(1.74236521665491,-1.,0.163289472382896));
#20986=CARTESIAN_POINT('',(1.7075470150345,-1.,0.383122945602004));
#20987=CARTESIAN_POINT('Origin',(0.,-1.,0.));
#20988=CARTESIAN_POINT('',(2.11275013067528,-1.,0.613422273260091));
#20989=CARTESIAN_POINT('Ctrl Pts',(1.7075470150345,-1.,0.383122945602004));
#20990=CARTESIAN_POINT('Ctrl Pts',(1.71231062891398,-1.,0.384119047314215));
#20991=CARTESIAN_POINT('Ctrl Pts',(1.72162022244582,-1.,0.386070790323281));
#20992=CARTESIAN_POINT('Ctrl Pts',(1.73493170972829,-1.,0.388877023502615));
#20993=CARTESIAN_POINT('Ctrl Pts',(1.75137405310193,-1.,0.392375812285396));
#20994=CARTESIAN_POINT('Ctrl Pts',(1.76975560043442,-1.,0.396346196110688));
#20995=CARTESIAN_POINT('Ctrl Pts',(1.78598826343754,-1.,0.399919403774156));
#20996=CARTESIAN_POINT('Ctrl Pts',(1.80012077173238,-1.,0.403107976163396));
#20997=CARTESIAN_POINT('Ctrl Pts',(1.81223801812013,-1.,0.405933518407176));
#20998=CARTESIAN_POINT('Ctrl Pts',(1.82247022677562,-1.,0.408428948106228));
#20999=CARTESIAN_POINT('Ctrl Pts',(1.83100408895047,-1.,0.410641256301276));
#21000=CARTESIAN_POINT('Ctrl Pts',(1.8380895347617,-1.,0.412633125322945));
#21001=CARTESIAN_POINT('Ctrl Pts',(1.84405757074218,-1.,0.414487438255542));
#21002=CARTESIAN_POINT('Ctrl Pts',(1.84929312930314,-1.,0.416300022039885));
#21003=CARTESIAN_POINT('Ctrl Pts',(1.8541763285645,-1.,0.418164129144046));
#21004=CARTESIAN_POINT('Ctrl Pts',(1.8590328109667,-1.,0.420157287975583));
#21005=CARTESIAN_POINT('Ctrl Pts',(1.86408083333863,-1.,0.422327307417885));
#21006=CARTESIAN_POINT('Ctrl Pts',(1.8693780394412,-1.,0.424678177290876));
#21007=CARTESIAN_POINT('Ctrl Pts',(1.87486989291333,-1.,0.427183828518743));
#21008=CARTESIAN_POINT('Ctrl Pts',(1.88044229001778,-1.,0.429803062482217));
#21009=CARTESIAN_POINT('Ctrl Pts',(1.88596913666828,-1.,0.432493038548833));
#21010=CARTESIAN_POINT('Ctrl Pts',(1.89136993975585,-1.,0.43522566096358));
#21011=CARTESIAN_POINT('Ctrl Pts',(1.89663648956549,-1.,0.437995003948443));
#21012=CARTESIAN_POINT('Ctrl Pts',(1.90180124389137,-1.,0.440807833704161));
#21013=CARTESIAN_POINT('Ctrl Pts',(1.90691756144906,-1.,0.443677556849171));
#21014=CARTESIAN_POINT('Ctrl Pts',(1.91203699981095,-1.,0.446617343485651));
#21015=CARTESIAN_POINT('Ctrl Pts',(1.91718342555717,-1.,0.449632260106572));
#21016=CARTESIAN_POINT('Ctrl Pts',(1.9223538064847,-1.,0.452719478359356));
#21017=CARTESIAN_POINT('Ctrl Pts',(1.92753067150461,-1.,0.455872005174336));
#21018=CARTESIAN_POINT('Ctrl Pts',(1.93269066517936,-1.,0.459081234547932));
#21019=CARTESIAN_POINT('Ctrl Pts',(1.93781486640834,-1.,0.462340031009087));
#21020=CARTESIAN_POINT('Ctrl Pts',(1.94289794196205,-1.,0.465645462026065));
#21021=CARTESIAN_POINT('Ctrl Pts',(1.94794381136524,-1.,0.468997482913158));
#21022=CARTESIAN_POINT('Ctrl Pts',(1.95296148278136,-1.,0.47239767226408));
#21023=CARTESIAN_POINT('Ctrl Pts',(1.95796111148175,-1.,0.475848034683172));
#21024=CARTESIAN_POINT('Ctrl Pts',(1.96294933055938,-1.,0.479349583074846));
#21025=CARTESIAN_POINT('Ctrl Pts',(1.96792703422358,-1.,0.482901662120687));
#21026=CARTESIAN_POINT('Ctrl Pts',(1.97289186263272,-1.,0.486502692907661));
#21027=CARTESIAN_POINT('Ctrl Pts',(1.97783973019229,-1.,0.490150627860955));
#21028=CARTESIAN_POINT('Ctrl Pts',(1.9827665876182,-1.,0.493843476541493));
#21029=CARTESIAN_POINT('Ctrl Pts',(1.98767044752929,-1.,0.497579909545564));
#21030=CARTESIAN_POINT('Ctrl Pts',(1.9925514912615,-1.,0.501359287727129));
#21031=CARTESIAN_POINT('Ctrl Pts',(1.99741107463567,-1.,0.505181361323011));
#21032=CARTESIAN_POINT('Ctrl Pts',(2.00225107134733,-1.,0.509046069886152));
#21033=CARTESIAN_POINT('Ctrl Pts',(2.00707309946955,-1.,0.512953306961814));
#21034=CARTESIAN_POINT('Ctrl Pts',(2.01187773939257,-1.,0.516902681728733));
#21035=CARTESIAN_POINT('Ctrl Pts',(2.01666477917305,-1.,0.520893590399429));
#21036=CARTESIAN_POINT('Ctrl Pts',(2.02143356304712,-1.,0.524925318333519));
#21037=CARTESIAN_POINT('Ctrl Pts',(2.02618329083289,-1.,0.528997127241911));
#21038=CARTESIAN_POINT('Ctrl Pts',(2.03091336214401,-1.,0.533108355132905));
#21039=CARTESIAN_POINT('Ctrl Pts',(2.03562362953993,-1.,0.537258489833135));
#21040=CARTESIAN_POINT('Ctrl Pts',(2.0403142269048,-1.,0.54144712061552));
#21041=CARTESIAN_POINT('Ctrl Pts',(2.0449854471456,-1.,0.545673903817349));
#21042=CARTESIAN_POINT('Ctrl Pts',(2.04963761077974,-1.,0.549938525150342));
#21043=CARTESIAN_POINT('Ctrl Pts',(2.05427091604482,-1.,0.55424065746411));
#21044=CARTESIAN_POINT('Ctrl Pts',(2.05888537756571,-1.,0.558579940185468));
#21045=CARTESIAN_POINT('Ctrl Pts',(2.06348090160697,-1.,0.562955993082574));
#21046=CARTESIAN_POINT('Ctrl Pts',(2.06805732997383,-1.,0.56736842118123));
#21047=CARTESIAN_POINT('Ctrl Pts',(2.07261449292757,-1.,0.571816823242411));
#21048=CARTESIAN_POINT('Ctrl Pts',(2.07715226767361,-1.,0.576300797416275));
#21049=CARTESIAN_POINT('Ctrl Pts',(2.08167059018138,-1.,0.580819952107257));
#21050=CARTESIAN_POINT('Ctrl Pts',(2.086169437277,-1.,0.585373918990895));
#21051=CARTESIAN_POINT('Ctrl Pts',(2.09064881812053,-1.,0.58996236540319));
#21052=CARTESIAN_POINT('Ctrl Pts',(2.09510876220501,-1.,0.594585006052824));
#21053=CARTESIAN_POINT('Ctrl Pts',(2.09954930865331,-1.,0.599241616422144));
#21054=CARTESIAN_POINT('Ctrl Pts',(2.10397049887709,-1.,0.603932030738212));
#21055=CARTESIAN_POINT('Ctrl Pts',(2.10749199615859,-1.,0.607711315456826));
#21056=CARTESIAN_POINT('Ctrl Pts',(2.11012443807661,-1.,0.610560911691114));
#21057=CARTESIAN_POINT('Ctrl Pts',(2.11187554260142,-1.,0.61246736556225));
#21058=CARTESIAN_POINT('Ctrl Pts',(2.11275013067528,-1.,0.613422273260091));
#21059=CARTESIAN_POINT('',(2.0698113262342,-1.,0.745574324794401));
#21060=CARTESIAN_POINT('',(2.11275013067528,-1.,0.613422273260091));
#21061=CARTESIAN_POINT('Ctrl Pts',(2.0698113262342,-1.,0.745574324794401));
#21062=CARTESIAN_POINT('Ctrl Pts',(2.06854248895575,-1.,0.74583279137781));
#21063=CARTESIAN_POINT('Ctrl Pts',(2.06600523016401,-1.,0.746345871542696));
#21064=CARTESIAN_POINT('Ctrl Pts',(2.06220058927162,-1.,0.747103932785504));
#21065=CARTESIAN_POINT('Ctrl Pts',(2.05713023030263,-1.,0.748091554181101));
#21066=CARTESIAN_POINT('Ctrl Pts',(2.05079645591606,-1.,0.749287468663053));
#21067=CARTESIAN_POINT('Ctrl Pts',(2.04446689147754,-1.,0.750444657874758));
#21068=CARTESIAN_POINT('Ctrl Pts',(2.03814160092173,-1.,0.751562963361384));
#21069=CARTESIAN_POINT('Ctrl Pts',(2.03182068456467,-1.,0.752642180488104));
#21070=CARTESIAN_POINT('Ctrl Pts',(2.02550428623587,-1.,0.753682061113766));
#21071=CARTESIAN_POINT('Ctrl Pts',(2.01919259406003,-1.,0.75468233072352));
#21072=CARTESIAN_POINT('Ctrl Pts',(2.01288584328149,-1.,0.755642704958101));
#21073=CARTESIAN_POINT('Ctrl Pts',(2.00658431587682,-1.,0.756562904646496));
#21074=CARTESIAN_POINT('Ctrl Pts',(2.00028834739072,-1.,0.757442676862342));
#21075=CARTESIAN_POINT('Ctrl Pts',(1.9939983109871,-1.,0.758281796766377));
#21076=CARTESIAN_POINT('Ctrl Pts',(1.98771456680806,-1.,0.759080037802243));
#21077=CARTESIAN_POINT('Ctrl Pts',(1.98143741418156,-1.,0.759837147452135));
#21078=CARTESIAN_POINT('Ctrl Pts',(1.97516705321521,-1.,0.760552825409856));
#21079=CARTESIAN_POINT('Ctrl Pts',(1.96890351582545,-1.,0.761226690483986));
#21080=CARTESIAN_POINT('Ctrl Pts',(1.96264672744229,-1.,0.761858300014575));
#21081=CARTESIAN_POINT('Ctrl Pts',(1.95639665309893,-1.,0.762447203806264));
#21082=CARTESIAN_POINT('Ctrl Pts',(1.95015342590025,-1.,0.762992990878774));
#21083=CARTESIAN_POINT('Ctrl Pts',(1.94391746617626,-1.,0.763495333538581));
#21084=CARTESIAN_POINT('Ctrl Pts',(1.93768964875867,-1.,0.763954049121394));
#21085=CARTESIAN_POINT('Ctrl Pts',(1.93147105496367,-1.,0.76436901067389));
#21086=CARTESIAN_POINT('Ctrl Pts',(1.92526263537041,-1.,0.764740025488189));
#21087=CARTESIAN_POINT('Ctrl Pts',(1.91906491634197,-1.,0.765066729667095));
#21088=CARTESIAN_POINT('Ctrl Pts',(1.91287765805174,-1.,0.765348465884739));
#21089=CARTESIAN_POINT('Ctrl Pts',(1.90669961402362,-1.,0.765584196937937));
#21090=CARTESIAN_POINT('Ctrl Pts',(1.90052930393599,-1.,0.765772772593395));
#21091=CARTESIAN_POINT('Ctrl Pts',(1.89436577771389,-1.,0.765913193856979));
#21092=CARTESIAN_POINT('Ctrl Pts',(1.88820926433409,-1.,0.76600483706209));
#21093=CARTESIAN_POINT('Ctrl Pts',(1.88206215302561,-1.,0.766047794851869));
#21094=CARTESIAN_POINT('Ctrl Pts',(1.87592888967886,-1.,0.766042837036759));
#21095=CARTESIAN_POINT('Ctrl Pts',(1.86981398314345,-1.,0.765990708546112));
#21096=CARTESIAN_POINT('Ctrl Pts',(1.86372027063314,-1.,0.765891519092557));
#21097=CARTESIAN_POINT('Ctrl Pts',(1.85764741390391,-1.,0.765744212909305));
#21098=CARTESIAN_POINT('Ctrl Pts',(1.85158945130054,-1.,0.765545710619023));
#21099=CARTESIAN_POINT('Ctrl Pts',(1.8455369887591,-1.,0.765291664861972));
#21100=CARTESIAN_POINT('Ctrl Pts',(1.83948181064823,-1.,0.764978057881688));
#21101=CARTESIAN_POINT('Ctrl Pts',(1.8334207722714,-1.,0.764602549687846));
#21102=CARTESIAN_POINT('Ctrl Pts',(1.8273599120008,-1.,0.764165902606056));
#21103=CARTESIAN_POINT('Ctrl Pts',(1.82131873145297,-1.,0.763673465462854));
#21104=CARTESIAN_POINT('Ctrl Pts',(1.81532118405566,-1.,0.763132003836783));
#21105=CARTESIAN_POINT('Ctrl Pts',(1.80938551463989,-1.,0.762546129464036));
#21106=CARTESIAN_POINT('Ctrl Pts',(1.80351583877334,-1.,0.761915336443516));
#21107=CARTESIAN_POINT('Ctrl Pts',(1.79768986997735,-1.,0.761229695230359));
#21108=CARTESIAN_POINT('Ctrl Pts',(1.79185815610802,-1.,0.760469555880425));
#21109=CARTESIAN_POINT('Ctrl Pts',(1.78596964884526,-1.,0.759614401109868));
#21110=CARTESIAN_POINT('Ctrl Pts',(1.77999411220912,-1.,0.75865062667738));
#21111=CARTESIAN_POINT('Ctrl Pts',(1.77394167108342,-1.,0.757578264077238));
#21112=CARTESIAN_POINT('Ctrl Pts',(1.76789396003141,-1.,0.756421896028403));
#21113=CARTESIAN_POINT('Ctrl Pts',(1.7619781724032,-1.,0.755220979975262));
#21114=CARTESIAN_POINT('Ctrl Pts',(1.75631083600175,-1.,0.75400925402848));
#21115=CARTESIAN_POINT('Ctrl Pts',(1.75095139468809,-1.,0.752797683531377));
#21116=CARTESIAN_POINT('Ctrl Pts',(1.74585086852298,-1.,0.751555614163629));
#21117=CARTESIAN_POINT('Ctrl Pts',(1.74080458266705,-1.,0.750193435979541));
#21118=CARTESIAN_POINT('Ctrl Pts',(1.73550351679848,-1.,0.748582462954855));
#21119=CARTESIAN_POINT('Ctrl Pts',(1.72958533647399,-1.,0.746574710096437));
#21120=CARTESIAN_POINT('Ctrl Pts',(1.7226822991693,-1.,0.744021445433765));
#21121=CARTESIAN_POINT('Ctrl Pts',(1.71447789751927,-1.,0.740795162032088));
#21122=CARTESIAN_POINT('Ctrl Pts',(1.70473309006121,-1.,0.736799665724771));
#21123=CARTESIAN_POINT('Ctrl Pts',(1.69326921975743,-1.,0.731963238697195));
#21124=CARTESIAN_POINT('Ctrl Pts',(1.67996158455503,-1.,0.726235967997433));
#21125=CARTESIAN_POINT('Ctrl Pts',(1.6647288055568,-1.,0.719585433804282));
#21126=CARTESIAN_POINT('Ctrl Pts',(1.64752408832016,-1.,0.711993139355394));
#21127=CARTESIAN_POINT('Ctrl Pts',(1.63216541664676,-1.,0.705159151988319));
#21128=CARTESIAN_POINT('Ctrl Pts',(1.61974673472612,-1.,0.699605146405088));
#21129=CARTESIAN_POINT('Ctrl Pts',(1.61106790958151,-1.,0.695712097881194));
#21130=CARTESIAN_POINT('Ctrl Pts',(1.60662857109684,-1.,0.693717979106306));
#21131=CARTESIAN_POINT('Origin',(0.,-1.,0.));
#21132=CARTESIAN_POINT('Origin',(0.,0.,0.));
#21133=CARTESIAN_POINT('Origin',(0.,2.2,0.));
#21134=CARTESIAN_POINT('Origin',(0.,1.,0.));
#21135=CARTESIAN_POINT('',(-1.4,2.2,1.71450551880629E-16));
#21136=CARTESIAN_POINT('Origin',(0.,2.2,0.));
#21137=CARTESIAN_POINT('',(-1.4,1.,1.71450551880629E-16));
#21138=CARTESIAN_POINT('',(-1.4,1.,1.71450551880629E-16));
#21139=CARTESIAN_POINT('Origin',(0.,1.,0.));
#21140=CARTESIAN_POINT('Origin',(0.,2.2,0.));
#21141=CARTESIAN_POINT('Ctrl Pts',(2.11275013067528,-1.,0.613422273260091));
#21142=CARTESIAN_POINT('Ctrl Pts',(2.11275013067528,1.,0.613422273260091));
#21143=CARTESIAN_POINT('Ctrl Pts',(2.11187554260142,-1.,0.61246736556225));
#21144=CARTESIAN_POINT('Ctrl Pts',(2.11187554260142,1.,0.61246736556225));
#21145=CARTESIAN_POINT('Ctrl Pts',(2.11012443807661,-1.,0.610560911691114));
#21146=CARTESIAN_POINT('Ctrl Pts',(2.11012443807661,1.,0.610560911691114));
#21147=CARTESIAN_POINT('Ctrl Pts',(2.10749199615859,-1.,0.607711315456826));
#21148=CARTESIAN_POINT('Ctrl Pts',(2.10749199615859,1.,0.607711315456826));
#21149=CARTESIAN_POINT('Ctrl Pts',(2.10397049887709,-1.,0.603932030738212));
#21150=CARTESIAN_POINT('Ctrl Pts',(2.10397049887709,1.,0.603932030738212));
#21151=CARTESIAN_POINT('Ctrl Pts',(2.09954930865331,-1.,0.599241616422144));
#21152=CARTESIAN_POINT('Ctrl Pts',(2.09954930865331,1.,0.599241616422144));
#21153=CARTESIAN_POINT('Ctrl Pts',(2.09510876220501,-1.,0.594585006052824));
#21154=CARTESIAN_POINT('Ctrl Pts',(2.09510876220501,1.,0.594585006052824));
#21155=CARTESIAN_POINT('Ctrl Pts',(2.09064881812053,-1.,0.58996236540319));
#21156=CARTESIAN_POINT('Ctrl Pts',(2.09064881812053,1.,0.58996236540319));
#21157=CARTESIAN_POINT('Ctrl Pts',(2.086169437277,-1.,0.585373918990895));
#21158=CARTESIAN_POINT('Ctrl Pts',(2.086169437277,1.,0.585373918990895));
#21159=CARTESIAN_POINT('Ctrl Pts',(2.08167059018138,-1.,0.580819952107257));
#21160=CARTESIAN_POINT('Ctrl Pts',(2.08167059018138,1.,0.580819952107257));
#21161=CARTESIAN_POINT('Ctrl Pts',(2.07715226767361,-1.,0.576300797416275));
#21162=CARTESIAN_POINT('Ctrl Pts',(2.07715226767361,1.,0.576300797416275));
#21163=CARTESIAN_POINT('Ctrl Pts',(2.07261449292757,-1.,0.571816823242411));
#21164=CARTESIAN_POINT('Ctrl Pts',(2.07261449292757,1.,0.571816823242411));
#21165=CARTESIAN_POINT('Ctrl Pts',(2.06805732997383,-1.,0.56736842118123));
#21166=CARTESIAN_POINT('Ctrl Pts',(2.06805732997383,1.,0.56736842118123));
#21167=CARTESIAN_POINT('Ctrl Pts',(2.06348090160697,-1.,0.562955993082574));
#21168=CARTESIAN_POINT('Ctrl Pts',(2.06348090160697,1.,0.562955993082574));
#21169=CARTESIAN_POINT('Ctrl Pts',(2.05888537756571,-1.,0.558579940185468));
#21170=CARTESIAN_POINT('Ctrl Pts',(2.05888537756571,1.,0.558579940185468));
#21171=CARTESIAN_POINT('Ctrl Pts',(2.05427091604482,-1.,0.55424065746411));
#21172=CARTESIAN_POINT('Ctrl Pts',(2.05427091604482,1.,0.55424065746411));
#21173=CARTESIAN_POINT('Ctrl Pts',(2.04963761077974,-1.,0.549938525150342));
#21174=CARTESIAN_POINT('Ctrl Pts',(2.04963761077974,1.,0.549938525150342));
#21175=CARTESIAN_POINT('Ctrl Pts',(2.0449854471456,-1.,0.545673903817349));
#21176=CARTESIAN_POINT('Ctrl Pts',(2.0449854471456,1.,0.545673903817349));
#21177=CARTESIAN_POINT('Ctrl Pts',(2.0403142269048,-1.,0.54144712061552));
#21178=CARTESIAN_POINT('Ctrl Pts',(2.0403142269048,1.,0.54144712061552));
#21179=CARTESIAN_POINT('Ctrl Pts',(2.03562362953993,-1.,0.537258489833135));
#21180=CARTESIAN_POINT('Ctrl Pts',(2.03562362953993,1.,0.537258489833135));
#21181=CARTESIAN_POINT('Ctrl Pts',(2.03091336214401,-1.,0.533108355132905));
#21182=CARTESIAN_POINT('Ctrl Pts',(2.03091336214401,1.,0.533108355132905));
#21183=CARTESIAN_POINT('Ctrl Pts',(2.02618329083289,-1.,0.528997127241911));
#21184=CARTESIAN_POINT('Ctrl Pts',(2.02618329083289,1.,0.528997127241911));
#21185=CARTESIAN_POINT('Ctrl Pts',(2.02143356304712,-1.,0.524925318333519));
#21186=CARTESIAN_POINT('Ctrl Pts',(2.02143356304712,1.,0.524925318333519));
#21187=CARTESIAN_POINT('Ctrl Pts',(2.01666477917305,-1.,0.520893590399429));
#21188=CARTESIAN_POINT('Ctrl Pts',(2.01666477917305,1.,0.520893590399429));
#21189=CARTESIAN_POINT('Ctrl Pts',(2.01187773939257,-1.,0.516902681728733));
#21190=CARTESIAN_POINT('Ctrl Pts',(2.01187773939257,1.,0.516902681728733));
#21191=CARTESIAN_POINT('Ctrl Pts',(2.00707309946955,-1.,0.512953306961814));
#21192=CARTESIAN_POINT('Ctrl Pts',(2.00707309946955,1.,0.512953306961814));
#21193=CARTESIAN_POINT('Ctrl Pts',(2.00225107134733,-1.,0.509046069886152));
#21194=CARTESIAN_POINT('Ctrl Pts',(2.00225107134733,1.,0.509046069886152));
#21195=CARTESIAN_POINT('Ctrl Pts',(1.99741107463567,-1.,0.505181361323011));
#21196=CARTESIAN_POINT('Ctrl Pts',(1.99741107463567,1.,0.505181361323011));
#21197=CARTESIAN_POINT('Ctrl Pts',(1.9925514912615,-1.,0.501359287727129));
#21198=CARTESIAN_POINT('Ctrl Pts',(1.9925514912615,1.,0.501359287727129));
#21199=CARTESIAN_POINT('Ctrl Pts',(1.98767044752929,-1.,0.497579909545564));
#21200=CARTESIAN_POINT('Ctrl Pts',(1.98767044752929,1.,0.497579909545564));
#21201=CARTESIAN_POINT('Ctrl Pts',(1.9827665876182,-1.,0.493843476541493));
#21202=CARTESIAN_POINT('Ctrl Pts',(1.9827665876182,1.,0.493843476541493));
#21203=CARTESIAN_POINT('Ctrl Pts',(1.97783973019229,-1.,0.490150627860955));
#21204=CARTESIAN_POINT('Ctrl Pts',(1.97783973019229,1.,0.490150627860955));
#21205=CARTESIAN_POINT('Ctrl Pts',(1.97289186263272,-1.,0.486502692907661));
#21206=CARTESIAN_POINT('Ctrl Pts',(1.97289186263272,1.,0.486502692907661));
#21207=CARTESIAN_POINT('Ctrl Pts',(1.96792703422358,-1.,0.482901662120687));
#21208=CARTESIAN_POINT('Ctrl Pts',(1.96792703422358,1.,0.482901662120687));
#21209=CARTESIAN_POINT('Ctrl Pts',(1.96294933055938,-1.,0.479349583074846));
#21210=CARTESIAN_POINT('Ctrl Pts',(1.96294933055938,1.,0.479349583074846));
#21211=CARTESIAN_POINT('Ctrl Pts',(1.95796111148175,-1.,0.475848034683172));
#21212=CARTESIAN_POINT('Ctrl Pts',(1.95796111148175,1.,0.475848034683172));
#21213=CARTESIAN_POINT('Ctrl Pts',(1.95296148278136,-1.,0.47239767226408));
#21214=CARTESIAN_POINT('Ctrl Pts',(1.95296148278136,1.,0.47239767226408));
#21215=CARTESIAN_POINT('Ctrl Pts',(1.94794381136524,-1.,0.468997482913158));
#21216=CARTESIAN_POINT('Ctrl Pts',(1.94794381136524,1.,0.468997482913158));
#21217=CARTESIAN_POINT('Ctrl Pts',(1.94289794196205,-1.,0.465645462026065));
#21218=CARTESIAN_POINT('Ctrl Pts',(1.94289794196205,1.,0.465645462026065));
#21219=CARTESIAN_POINT('Ctrl Pts',(1.93781486640834,-1.,0.462340031009087));
#21220=CARTESIAN_POINT('Ctrl Pts',(1.93781486640834,1.,0.462340031009087));
#21221=CARTESIAN_POINT('Ctrl Pts',(1.93269066517936,-1.,0.459081234547932));
#21222=CARTESIAN_POINT('Ctrl Pts',(1.93269066517936,1.,0.459081234547932));
#21223=CARTESIAN_POINT('Ctrl Pts',(1.92753067150461,-1.,0.455872005174336));
#21224=CARTESIAN_POINT('Ctrl Pts',(1.92753067150461,1.,0.455872005174336));
#21225=CARTESIAN_POINT('Ctrl Pts',(1.9223538064847,-1.,0.452719478359356));
#21226=CARTESIAN_POINT('Ctrl Pts',(1.9223538064847,1.,0.452719478359356));
#21227=CARTESIAN_POINT('Ctrl Pts',(1.91718342555717,-1.,0.449632260106572));
#21228=CARTESIAN_POINT('Ctrl Pts',(1.91718342555717,1.,0.449632260106572));
#21229=CARTESIAN_POINT('Ctrl Pts',(1.91203699981095,-1.,0.446617343485651));
#21230=CARTESIAN_POINT('Ctrl Pts',(1.91203699981095,1.,0.446617343485651));
#21231=CARTESIAN_POINT('Ctrl Pts',(1.90691756144906,-1.,0.443677556849171));
#21232=CARTESIAN_POINT('Ctrl Pts',(1.90691756144906,1.,0.443677556849171));
#21233=CARTESIAN_POINT('Ctrl Pts',(1.90180124389137,-1.,0.440807833704161));
#21234=CARTESIAN_POINT('Ctrl Pts',(1.90180124389137,1.,0.440807833704161));
#21235=CARTESIAN_POINT('Ctrl Pts',(1.89663648956549,-1.,0.437995003948443));
#21236=CARTESIAN_POINT('Ctrl Pts',(1.89663648956549,1.,0.437995003948443));
#21237=CARTESIAN_POINT('Ctrl Pts',(1.89136993975585,-1.,0.43522566096358));
#21238=CARTESIAN_POINT('Ctrl Pts',(1.89136993975585,1.,0.43522566096358));
#21239=CARTESIAN_POINT('Ctrl Pts',(1.88596913666828,-1.,0.432493038548833));
#21240=CARTESIAN_POINT('Ctrl Pts',(1.88596913666828,1.,0.432493038548833));
#21241=CARTESIAN_POINT('Ctrl Pts',(1.88044229001778,-1.,0.429803062482217));
#21242=CARTESIAN_POINT('Ctrl Pts',(1.88044229001778,1.,0.429803062482217));
#21243=CARTESIAN_POINT('Ctrl Pts',(1.87486989291333,-1.,0.427183828518743));
#21244=CARTESIAN_POINT('Ctrl Pts',(1.87486989291333,1.,0.427183828518743));
#21245=CARTESIAN_POINT('Ctrl Pts',(1.8693780394412,-1.,0.424678177290876));
#21246=CARTESIAN_POINT('Ctrl Pts',(1.8693780394412,1.,0.424678177290876));
#21247=CARTESIAN_POINT('Ctrl Pts',(1.86408083333863,-1.,0.422327307417885));
#21248=CARTESIAN_POINT('Ctrl Pts',(1.86408083333863,1.,0.422327307417885));
#21249=CARTESIAN_POINT('Ctrl Pts',(1.8590328109667,-1.,0.420157287975583));
#21250=CARTESIAN_POINT('Ctrl Pts',(1.8590328109667,1.,0.420157287975583));
#21251=CARTESIAN_POINT('Ctrl Pts',(1.8541763285645,-1.,0.418164129144046));
#21252=CARTESIAN_POINT('Ctrl Pts',(1.8541763285645,1.,0.418164129144046));
#21253=CARTESIAN_POINT('Ctrl Pts',(1.84929312930314,-1.,0.416300022039885));
#21254=CARTESIAN_POINT('Ctrl Pts',(1.84929312930314,1.,0.416300022039885));
#21255=CARTESIAN_POINT('Ctrl Pts',(1.84405757074218,-1.,0.414487438255542));
#21256=CARTESIAN_POINT('Ctrl Pts',(1.84405757074218,1.,0.414487438255542));
#21257=CARTESIAN_POINT('Ctrl Pts',(1.8380895347617,-1.,0.412633125322945));
#21258=CARTESIAN_POINT('Ctrl Pts',(1.8380895347617,1.,0.412633125322945));
#21259=CARTESIAN_POINT('Ctrl Pts',(1.83100408895047,-1.,0.410641256301276));
#21260=CARTESIAN_POINT('Ctrl Pts',(1.83100408895047,1.,0.410641256301276));
#21261=CARTESIAN_POINT('Ctrl Pts',(1.82247022677562,-1.,0.408428948106228));
#21262=CARTESIAN_POINT('Ctrl Pts',(1.82247022677562,1.,0.408428948106228));
#21263=CARTESIAN_POINT('Ctrl Pts',(1.81223801812013,-1.,0.405933518407176));
#21264=CARTESIAN_POINT('Ctrl Pts',(1.81223801812013,1.,0.405933518407176));
#21265=CARTESIAN_POINT('Ctrl Pts',(1.80012077173238,-1.,0.403107976163396));
#21266=CARTESIAN_POINT('Ctrl Pts',(1.80012077173238,1.,0.403107976163396));
#21267=CARTESIAN_POINT('Ctrl Pts',(1.78598826343754,-1.,0.399919403774156));
#21268=CARTESIAN_POINT('Ctrl Pts',(1.78598826343754,1.,0.399919403774156));
#21269=CARTESIAN_POINT('Ctrl Pts',(1.76975560043442,-1.,0.396346196110688));
#21270=CARTESIAN_POINT('Ctrl Pts',(1.76975560043442,1.,0.396346196110688));
#21271=CARTESIAN_POINT('Ctrl Pts',(1.75137405310193,-1.,0.392375812285396));
#21272=CARTESIAN_POINT('Ctrl Pts',(1.75137405310193,1.,0.392375812285396));
#21273=CARTESIAN_POINT('Ctrl Pts',(1.73493170972829,-1.,0.388877023502615));
#21274=CARTESIAN_POINT('Ctrl Pts',(1.73493170972829,1.,0.388877023502615));
#21275=CARTESIAN_POINT('Ctrl Pts',(1.72162022244582,-1.,0.386070790323281));
#21276=CARTESIAN_POINT('Ctrl Pts',(1.72162022244582,1.,0.386070790323281));
#21277=CARTESIAN_POINT('Ctrl Pts',(1.71231062891398,-1.,0.384119047314215));
#21278=CARTESIAN_POINT('Ctrl Pts',(1.71231062891398,1.,0.384119047314215));
#21279=CARTESIAN_POINT('Ctrl Pts',(1.7075470150345,-1.,0.383122945602004));
#21280=CARTESIAN_POINT('Ctrl Pts',(1.7075470150345,1.,0.383122945602004));
#21281=CARTESIAN_POINT('',(1.7075470150345,1.,0.383122945602004));
#21282=CARTESIAN_POINT('',(1.7075470150345,0.,0.383122945602005));
#21283=CARTESIAN_POINT('',(2.11275013067528,1.,0.613422273260091));
#21284=CARTESIAN_POINT('Ctrl Pts',(2.11275013067528,1.,0.613422273260091));
#21285=CARTESIAN_POINT('Ctrl Pts',(2.11187554260142,1.,0.61246736556225));
#21286=CARTESIAN_POINT('Ctrl Pts',(2.11012443807661,1.,0.610560911691114));
#21287=CARTESIAN_POINT('Ctrl Pts',(2.10749199615859,1.,0.607711315456826));
#21288=CARTESIAN_POINT('Ctrl Pts',(2.10397049887709,1.,0.603932030738212));
#21289=CARTESIAN_POINT('Ctrl Pts',(2.09954930865331,1.,0.599241616422144));
#21290=CARTESIAN_POINT('Ctrl Pts',(2.09510876220501,1.,0.594585006052824));
#21291=CARTESIAN_POINT('Ctrl Pts',(2.09064881812053,1.,0.58996236540319));
#21292=CARTESIAN_POINT('Ctrl Pts',(2.086169437277,1.,0.585373918990895));
#21293=CARTESIAN_POINT('Ctrl Pts',(2.08167059018138,1.,0.580819952107257));
#21294=CARTESIAN_POINT('Ctrl Pts',(2.07715226767361,1.,0.576300797416275));
#21295=CARTESIAN_POINT('Ctrl Pts',(2.07261449292757,1.,0.571816823242411));
#21296=CARTESIAN_POINT('Ctrl Pts',(2.06805732997383,1.,0.56736842118123));
#21297=CARTESIAN_POINT('Ctrl Pts',(2.06348090160697,1.,0.562955993082574));
#21298=CARTESIAN_POINT('Ctrl Pts',(2.05888537756571,1.,0.558579940185468));
#21299=CARTESIAN_POINT('Ctrl Pts',(2.05427091604482,1.,0.55424065746411));
#21300=CARTESIAN_POINT('Ctrl Pts',(2.04963761077974,1.,0.549938525150342));
#21301=CARTESIAN_POINT('Ctrl Pts',(2.0449854471456,1.,0.545673903817349));
#21302=CARTESIAN_POINT('Ctrl Pts',(2.0403142269048,1.,0.54144712061552));
#21303=CARTESIAN_POINT('Ctrl Pts',(2.03562362953993,1.,0.537258489833135));
#21304=CARTESIAN_POINT('Ctrl Pts',(2.03091336214401,1.,0.533108355132905));
#21305=CARTESIAN_POINT('Ctrl Pts',(2.02618329083289,1.,0.528997127241911));
#21306=CARTESIAN_POINT('Ctrl Pts',(2.02143356304712,1.,0.524925318333519));
#21307=CARTESIAN_POINT('Ctrl Pts',(2.01666477917305,1.,0.520893590399429));
#21308=CARTESIAN_POINT('Ctrl Pts',(2.01187773939257,1.,0.516902681728733));
#21309=CARTESIAN_POINT('Ctrl Pts',(2.00707309946955,1.,0.512953306961814));
#21310=CARTESIAN_POINT('Ctrl Pts',(2.00225107134733,1.,0.509046069886152));
#21311=CARTESIAN_POINT('Ctrl Pts',(1.99741107463567,1.,0.505181361323011));
#21312=CARTESIAN_POINT('Ctrl Pts',(1.9925514912615,1.,0.501359287727129));
#21313=CARTESIAN_POINT('Ctrl Pts',(1.98767044752929,1.,0.497579909545564));
#21314=CARTESIAN_POINT('Ctrl Pts',(1.9827665876182,1.,0.493843476541493));
#21315=CARTESIAN_POINT('Ctrl Pts',(1.97783973019229,1.,0.490150627860955));
#21316=CARTESIAN_POINT('Ctrl Pts',(1.97289186263272,1.,0.486502692907661));
#21317=CARTESIAN_POINT('Ctrl Pts',(1.96792703422358,1.,0.482901662120687));
#21318=CARTESIAN_POINT('Ctrl Pts',(1.96294933055938,1.,0.479349583074846));
#21319=CARTESIAN_POINT('Ctrl Pts',(1.95796111148175,1.,0.475848034683172));
#21320=CARTESIAN_POINT('Ctrl Pts',(1.95296148278136,1.,0.47239767226408));
#21321=CARTESIAN_POINT('Ctrl Pts',(1.94794381136524,1.,0.468997482913158));
#21322=CARTESIAN_POINT('Ctrl Pts',(1.94289794196205,1.,0.465645462026065));
#21323=CARTESIAN_POINT('Ctrl Pts',(1.93781486640834,1.,0.462340031009087));
#21324=CARTESIAN_POINT('Ctrl Pts',(1.93269066517936,1.,0.459081234547932));
#21325=CARTESIAN_POINT('Ctrl Pts',(1.92753067150461,1.,0.455872005174336));
#21326=CARTESIAN_POINT('Ctrl Pts',(1.9223538064847,1.,0.452719478359356));
#21327=CARTESIAN_POINT('Ctrl Pts',(1.91718342555717,1.,0.449632260106572));
#21328=CARTESIAN_POINT('Ctrl Pts',(1.91203699981095,1.,0.446617343485651));
#21329=CARTESIAN_POINT('Ctrl Pts',(1.90691756144906,1.,0.443677556849171));
#21330=CARTESIAN_POINT('Ctrl Pts',(1.90180124389137,1.,0.440807833704161));
#21331=CARTESIAN_POINT('Ctrl Pts',(1.89663648956549,1.,0.437995003948443));
#21332=CARTESIAN_POINT('Ctrl Pts',(1.89136993975585,1.,0.43522566096358));
#21333=CARTESIAN_POINT('Ctrl Pts',(1.88596913666828,1.,0.432493038548833));
#21334=CARTESIAN_POINT('Ctrl Pts',(1.88044229001778,1.,0.429803062482217));
#21335=CARTESIAN_POINT('Ctrl Pts',(1.87486989291333,1.,0.427183828518743));
#21336=CARTESIAN_POINT('Ctrl Pts',(1.8693780394412,1.,0.424678177290876));
#21337=CARTESIAN_POINT('Ctrl Pts',(1.86408083333863,1.,0.422327307417885));
#21338=CARTESIAN_POINT('Ctrl Pts',(1.8590328109667,1.,0.420157287975583));
#21339=CARTESIAN_POINT('Ctrl Pts',(1.8541763285645,1.,0.418164129144046));
#21340=CARTESIAN_POINT('Ctrl Pts',(1.84929312930314,1.,0.416300022039885));
#21341=CARTESIAN_POINT('Ctrl Pts',(1.84405757074218,1.,0.414487438255542));
#21342=CARTESIAN_POINT('Ctrl Pts',(1.8380895347617,1.,0.412633125322945));
#21343=CARTESIAN_POINT('Ctrl Pts',(1.83100408895047,1.,0.410641256301276));
#21344=CARTESIAN_POINT('Ctrl Pts',(1.82247022677562,1.,0.408428948106228));
#21345=CARTESIAN_POINT('Ctrl Pts',(1.81223801812013,1.,0.405933518407176));
#21346=CARTESIAN_POINT('Ctrl Pts',(1.80012077173238,1.,0.403107976163396));
#21347=CARTESIAN_POINT('Ctrl Pts',(1.78598826343754,1.,0.399919403774156));
#21348=CARTESIAN_POINT('Ctrl Pts',(1.76975560043442,1.,0.396346196110688));
#21349=CARTESIAN_POINT('Ctrl Pts',(1.75137405310193,1.,0.392375812285396));
#21350=CARTESIAN_POINT('Ctrl Pts',(1.73493170972829,1.,0.388877023502615));
#21351=CARTESIAN_POINT('Ctrl Pts',(1.72162022244582,1.,0.386070790323281));
#21352=CARTESIAN_POINT('Ctrl Pts',(1.71231062891398,1.,0.384119047314215));
#21353=CARTESIAN_POINT('Ctrl Pts',(1.7075470150345,1.,0.383122945602004));
#21354=CARTESIAN_POINT('',(2.11275013067528,0.,0.613422273260091));
#21355=CARTESIAN_POINT('Origin',(2.0698113262342,0.,0.745574324794401));
#21356=CARTESIAN_POINT('',(2.0698113262342,1.,0.745574324794401));
#21357=CARTESIAN_POINT('',(2.11275013067528,1.,0.613422273260091));
#21358=CARTESIAN_POINT('',(2.0698113262342,0.,0.745574324794401));
#21359=CARTESIAN_POINT('Ctrl Pts',(1.60662857109684,-1.,0.693717979106306));
#21360=CARTESIAN_POINT('Ctrl Pts',(1.60662857109684,1.,0.693717979106306));
#21361=CARTESIAN_POINT('Ctrl Pts',(1.61106790958151,-1.,0.695712097881194));
#21362=CARTESIAN_POINT('Ctrl Pts',(1.61106790958151,1.,0.695712097881194));
#21363=CARTESIAN_POINT('Ctrl Pts',(1.61974673472612,-1.,0.699605146405088));
#21364=CARTESIAN_POINT('Ctrl Pts',(1.61974673472612,1.,0.699605146405088));
#21365=CARTESIAN_POINT('Ctrl Pts',(1.63216541664676,-1.,0.705159151988319));
#21366=CARTESIAN_POINT('Ctrl Pts',(1.63216541664676,1.,0.705159151988319));
#21367=CARTESIAN_POINT('Ctrl Pts',(1.64752408832016,-1.,0.711993139355394));
#21368=CARTESIAN_POINT('Ctrl Pts',(1.64752408832016,1.,0.711993139355394));
#21369=CARTESIAN_POINT('Ctrl Pts',(1.6647288055568,-1.,0.719585433804282));
#21370=CARTESIAN_POINT('Ctrl Pts',(1.6647288055568,1.,0.719585433804282));
#21371=CARTESIAN_POINT('Ctrl Pts',(1.67996158455503,-1.,0.726235967997433));
#21372=CARTESIAN_POINT('Ctrl Pts',(1.67996158455503,1.,0.726235967997433));
#21373=CARTESIAN_POINT('Ctrl Pts',(1.69326921975743,-1.,0.731963238697195));
#21374=CARTESIAN_POINT('Ctrl Pts',(1.69326921975743,1.,0.731963238697195));
#21375=CARTESIAN_POINT('Ctrl Pts',(1.70473309006121,-1.,0.736799665724771));
#21376=CARTESIAN_POINT('Ctrl Pts',(1.70473309006121,1.,0.736799665724771));
#21377=CARTESIAN_POINT('Ctrl Pts',(1.71447789751927,-1.,0.740795162032088));
#21378=CARTESIAN_POINT('Ctrl Pts',(1.71447789751927,1.,0.740795162032088));
#21379=CARTESIAN_POINT('Ctrl Pts',(1.7226822991693,-1.,0.744021445433765));
#21380=CARTESIAN_POINT('Ctrl Pts',(1.7226822991693,1.,0.744021445433765));
#21381=CARTESIAN_POINT('Ctrl Pts',(1.72958533647399,-1.,0.746574710096437));
#21382=CARTESIAN_POINT('Ctrl Pts',(1.72958533647399,1.,0.746574710096437));
#21383=CARTESIAN_POINT('Ctrl Pts',(1.73550351679848,-1.,0.748582462954855));
#21384=CARTESIAN_POINT('Ctrl Pts',(1.73550351679848,1.,0.748582462954855));
#21385=CARTESIAN_POINT('Ctrl Pts',(1.74080458266705,-1.,0.750193435979541));
#21386=CARTESIAN_POINT('Ctrl Pts',(1.74080458266705,1.,0.750193435979541));
#21387=CARTESIAN_POINT('Ctrl Pts',(1.74585086852298,-1.,0.751555614163629));
#21388=CARTESIAN_POINT('Ctrl Pts',(1.74585086852298,1.,0.751555614163629));
#21389=CARTESIAN_POINT('Ctrl Pts',(1.75095139468809,-1.,0.752797683531377));
#21390=CARTESIAN_POINT('Ctrl Pts',(1.75095139468809,1.,0.752797683531377));
#21391=CARTESIAN_POINT('Ctrl Pts',(1.75631083600175,-1.,0.75400925402848));
#21392=CARTESIAN_POINT('Ctrl Pts',(1.75631083600175,1.,0.75400925402848));
#21393=CARTESIAN_POINT('Ctrl Pts',(1.7619781724032,-1.,0.755220979975262));
#21394=CARTESIAN_POINT('Ctrl Pts',(1.7619781724032,1.,0.755220979975262));
#21395=CARTESIAN_POINT('Ctrl Pts',(1.76789396003141,-1.,0.756421896028403));
#21396=CARTESIAN_POINT('Ctrl Pts',(1.76789396003141,1.,0.756421896028403));
#21397=CARTESIAN_POINT('Ctrl Pts',(1.77394167108342,-1.,0.757578264077238));
#21398=CARTESIAN_POINT('Ctrl Pts',(1.77394167108342,1.,0.757578264077238));
#21399=CARTESIAN_POINT('Ctrl Pts',(1.77999411220912,-1.,0.75865062667738));
#21400=CARTESIAN_POINT('Ctrl Pts',(1.77999411220912,1.,0.75865062667738));
#21401=CARTESIAN_POINT('Ctrl Pts',(1.78596964884526,-1.,0.759614401109868));
#21402=CARTESIAN_POINT('Ctrl Pts',(1.78596964884526,1.,0.759614401109868));
#21403=CARTESIAN_POINT('Ctrl Pts',(1.79185815610802,-1.,0.760469555880425));
#21404=CARTESIAN_POINT('Ctrl Pts',(1.79185815610802,1.,0.760469555880425));
#21405=CARTESIAN_POINT('Ctrl Pts',(1.79768986997735,-1.,0.761229695230359));
#21406=CARTESIAN_POINT('Ctrl Pts',(1.79768986997735,1.,0.761229695230359));
#21407=CARTESIAN_POINT('Ctrl Pts',(1.80351583877334,-1.,0.761915336443516));
#21408=CARTESIAN_POINT('Ctrl Pts',(1.80351583877334,1.,0.761915336443516));
#21409=CARTESIAN_POINT('Ctrl Pts',(1.80938551463989,-1.,0.762546129464036));
#21410=CARTESIAN_POINT('Ctrl Pts',(1.80938551463989,1.,0.762546129464036));
#21411=CARTESIAN_POINT('Ctrl Pts',(1.81532118405566,-1.,0.763132003836783));
#21412=CARTESIAN_POINT('Ctrl Pts',(1.81532118405566,1.,0.763132003836783));
#21413=CARTESIAN_POINT('Ctrl Pts',(1.82131873145297,-1.,0.763673465462854));
#21414=CARTESIAN_POINT('Ctrl Pts',(1.82131873145297,1.,0.763673465462854));
#21415=CARTESIAN_POINT('Ctrl Pts',(1.8273599120008,-1.,0.764165902606056));
#21416=CARTESIAN_POINT('Ctrl Pts',(1.8273599120008,1.,0.764165902606056));
#21417=CARTESIAN_POINT('Ctrl Pts',(1.8334207722714,-1.,0.764602549687846));
#21418=CARTESIAN_POINT('Ctrl Pts',(1.8334207722714,1.,0.764602549687846));
#21419=CARTESIAN_POINT('Ctrl Pts',(1.83948181064823,-1.,0.764978057881688));
#21420=CARTESIAN_POINT('Ctrl Pts',(1.83948181064823,1.,0.764978057881688));
#21421=CARTESIAN_POINT('Ctrl Pts',(1.8455369887591,-1.,0.765291664861972));
#21422=CARTESIAN_POINT('Ctrl Pts',(1.8455369887591,1.,0.765291664861972));
#21423=CARTESIAN_POINT('Ctrl Pts',(1.85158945130054,-1.,0.765545710619023));
#21424=CARTESIAN_POINT('Ctrl Pts',(1.85158945130054,1.,0.765545710619023));
#21425=CARTESIAN_POINT('Ctrl Pts',(1.85764741390391,-1.,0.765744212909305));
#21426=CARTESIAN_POINT('Ctrl Pts',(1.85764741390391,1.,0.765744212909305));
#21427=CARTESIAN_POINT('Ctrl Pts',(1.86372027063314,-1.,0.765891519092557));
#21428=CARTESIAN_POINT('Ctrl Pts',(1.86372027063314,1.,0.765891519092557));
#21429=CARTESIAN_POINT('Ctrl Pts',(1.86981398314345,-1.,0.765990708546112));
#21430=CARTESIAN_POINT('Ctrl Pts',(1.86981398314345,1.,0.765990708546112));
#21431=CARTESIAN_POINT('Ctrl Pts',(1.87592888967886,-1.,0.766042837036759));
#21432=CARTESIAN_POINT('Ctrl Pts',(1.87592888967886,1.,0.766042837036759));
#21433=CARTESIAN_POINT('Ctrl Pts',(1.88206215302561,-1.,0.766047794851869));
#21434=CARTESIAN_POINT('Ctrl Pts',(1.88206215302561,1.,0.766047794851869));
#21435=CARTESIAN_POINT('Ctrl Pts',(1.88820926433409,-1.,0.76600483706209));
#21436=CARTESIAN_POINT('Ctrl Pts',(1.88820926433409,1.,0.76600483706209));
#21437=CARTESIAN_POINT('Ctrl Pts',(1.89436577771389,-1.,0.765913193856979));
#21438=CARTESIAN_POINT('Ctrl Pts',(1.89436577771389,1.,0.765913193856979));
#21439=CARTESIAN_POINT('Ctrl Pts',(1.90052930393599,-1.,0.765772772593395));
#21440=CARTESIAN_POINT('Ctrl Pts',(1.90052930393599,1.,0.765772772593395));
#21441=CARTESIAN_POINT('Ctrl Pts',(1.90669961402362,-1.,0.765584196937937));
#21442=CARTESIAN_POINT('Ctrl Pts',(1.90669961402362,1.,0.765584196937937));
#21443=CARTESIAN_POINT('Ctrl Pts',(1.91287765805174,-1.,0.765348465884739));
#21444=CARTESIAN_POINT('Ctrl Pts',(1.91287765805174,1.,0.765348465884739));
#21445=CARTESIAN_POINT('Ctrl Pts',(1.91906491634197,-1.,0.765066729667095));
#21446=CARTESIAN_POINT('Ctrl Pts',(1.91906491634197,1.,0.765066729667095));
#21447=CARTESIAN_POINT('Ctrl Pts',(1.92526263537041,-1.,0.764740025488189));
#21448=CARTESIAN_POINT('Ctrl Pts',(1.92526263537041,1.,0.764740025488189));
#21449=CARTESIAN_POINT('Ctrl Pts',(1.93147105496367,-1.,0.76436901067389));
#21450=CARTESIAN_POINT('Ctrl Pts',(1.93147105496367,1.,0.76436901067389));
#21451=CARTESIAN_POINT('Ctrl Pts',(1.93768964875867,-1.,0.763954049121394));
#21452=CARTESIAN_POINT('Ctrl Pts',(1.93768964875867,1.,0.763954049121394));
#21453=CARTESIAN_POINT('Ctrl Pts',(1.94391746617626,-1.,0.763495333538581));
#21454=CARTESIAN_POINT('Ctrl Pts',(1.94391746617626,1.,0.763495333538581));
#21455=CARTESIAN_POINT('Ctrl Pts',(1.95015342590025,-1.,0.762992990878774));
#21456=CARTESIAN_POINT('Ctrl Pts',(1.95015342590025,1.,0.762992990878774));
#21457=CARTESIAN_POINT('Ctrl Pts',(1.95639665309893,-1.,0.762447203806264));
#21458=CARTESIAN_POINT('Ctrl Pts',(1.95639665309893,1.,0.762447203806264));
#21459=CARTESIAN_POINT('Ctrl Pts',(1.96264672744229,-1.,0.761858300014575));
#21460=CARTESIAN_POINT('Ctrl Pts',(1.96264672744229,1.,0.761858300014575));
#21461=CARTESIAN_POINT('Ctrl Pts',(1.96890351582545,-1.,0.761226690483986));
#21462=CARTESIAN_POINT('Ctrl Pts',(1.96890351582545,1.,0.761226690483986));
#21463=CARTESIAN_POINT('Ctrl Pts',(1.97516705321521,-1.,0.760552825409856));
#21464=CARTESIAN_POINT('Ctrl Pts',(1.97516705321521,1.,0.760552825409856));
#21465=CARTESIAN_POINT('Ctrl Pts',(1.98143741418156,-1.,0.759837147452135));
#21466=CARTESIAN_POINT('Ctrl Pts',(1.98143741418156,1.,0.759837147452135));
#21467=CARTESIAN_POINT('Ctrl Pts',(1.98771456680806,-1.,0.759080037802243));
#21468=CARTESIAN_POINT('Ctrl Pts',(1.98771456680806,1.,0.759080037802243));
#21469=CARTESIAN_POINT('Ctrl Pts',(1.9939983109871,-1.,0.758281796766377));
#21470=CARTESIAN_POINT('Ctrl Pts',(1.9939983109871,1.,0.758281796766377));
#21471=CARTESIAN_POINT('Ctrl Pts',(2.00028834739072,-1.,0.757442676862342));
#21472=CARTESIAN_POINT('Ctrl Pts',(2.00028834739072,1.,0.757442676862342));
#21473=CARTESIAN_POINT('Ctrl Pts',(2.00658431587682,-1.,0.756562904646496));
#21474=CARTESIAN_POINT('Ctrl Pts',(2.00658431587682,1.,0.756562904646496));
#21475=CARTESIAN_POINT('Ctrl Pts',(2.01288584328149,-1.,0.755642704958101));
#21476=CARTESIAN_POINT('Ctrl Pts',(2.01288584328149,1.,0.755642704958101));
#21477=CARTESIAN_POINT('Ctrl Pts',(2.01919259406003,-1.,0.75468233072352));
#21478=CARTESIAN_POINT('Ctrl Pts',(2.01919259406003,1.,0.75468233072352));
#21479=CARTESIAN_POINT('Ctrl Pts',(2.02550428623587,-1.,0.753682061113766));
#21480=CARTESIAN_POINT('Ctrl Pts',(2.02550428623587,1.,0.753682061113766));
#21481=CARTESIAN_POINT('Ctrl Pts',(2.03182068456467,-1.,0.752642180488104));
#21482=CARTESIAN_POINT('Ctrl Pts',(2.03182068456467,1.,0.752642180488104));
#21483=CARTESIAN_POINT('Ctrl Pts',(2.03814160092173,-1.,0.751562963361384));
#21484=CARTESIAN_POINT('Ctrl Pts',(2.03814160092173,1.,0.751562963361384));
#21485=CARTESIAN_POINT('Ctrl Pts',(2.04446689147754,-1.,0.750444657874758));
#21486=CARTESIAN_POINT('Ctrl Pts',(2.04446689147754,1.,0.750444657874758));
#21487=CARTESIAN_POINT('Ctrl Pts',(2.05079645591606,-1.,0.749287468663053));
#21488=CARTESIAN_POINT('Ctrl Pts',(2.05079645591606,1.,0.749287468663053));
#21489=CARTESIAN_POINT('Ctrl Pts',(2.05713023030263,-1.,0.748091554181101));
#21490=CARTESIAN_POINT('Ctrl Pts',(2.05713023030263,1.,0.748091554181101));
#21491=CARTESIAN_POINT('Ctrl Pts',(2.06220058927162,-1.,0.747103932785504));
#21492=CARTESIAN_POINT('Ctrl Pts',(2.06220058927162,1.,0.747103932785504));
#21493=CARTESIAN_POINT('Ctrl Pts',(2.06600523016401,-1.,0.746345871542696));
#21494=CARTESIAN_POINT('Ctrl Pts',(2.06600523016401,1.,0.746345871542696));
#21495=CARTESIAN_POINT('Ctrl Pts',(2.06854248895575,-1.,0.74583279137781));
#21496=CARTESIAN_POINT('Ctrl Pts',(2.06854248895575,1.,0.74583279137781));
#21497=CARTESIAN_POINT('Ctrl Pts',(2.0698113262342,-1.,0.745574324794401));
#21498=CARTESIAN_POINT('Ctrl Pts',(2.0698113262342,1.,0.745574324794401));
#21499=CARTESIAN_POINT('',(1.60662857109684,1.,0.693717979106306));
#21500=CARTESIAN_POINT('Ctrl Pts',(1.60662857109684,1.,0.693717979106306));
#21501=CARTESIAN_POINT('Ctrl Pts',(1.61106790958151,1.,0.695712097881194));
#21502=CARTESIAN_POINT('Ctrl Pts',(1.61974673472612,1.,0.699605146405088));
#21503=CARTESIAN_POINT('Ctrl Pts',(1.63216541664676,1.,0.705159151988319));
#21504=CARTESIAN_POINT('Ctrl Pts',(1.64752408832016,1.,0.711993139355394));
#21505=CARTESIAN_POINT('Ctrl Pts',(1.6647288055568,1.,0.719585433804282));
#21506=CARTESIAN_POINT('Ctrl Pts',(1.67996158455503,1.,0.726235967997433));
#21507=CARTESIAN_POINT('Ctrl Pts',(1.69326921975743,1.,0.731963238697195));
#21508=CARTESIAN_POINT('Ctrl Pts',(1.70473309006121,1.,0.736799665724771));
#21509=CARTESIAN_POINT('Ctrl Pts',(1.71447789751927,1.,0.740795162032088));
#21510=CARTESIAN_POINT('Ctrl Pts',(1.7226822991693,1.,0.744021445433765));
#21511=CARTESIAN_POINT('Ctrl Pts',(1.72958533647399,1.,0.746574710096437));
#21512=CARTESIAN_POINT('Ctrl Pts',(1.73550351679848,1.,0.748582462954855));
#21513=CARTESIAN_POINT('Ctrl Pts',(1.74080458266705,1.,0.750193435979541));
#21514=CARTESIAN_POINT('Ctrl Pts',(1.74585086852298,1.,0.751555614163629));
#21515=CARTESIAN_POINT('Ctrl Pts',(1.75095139468809,1.,0.752797683531377));
#21516=CARTESIAN_POINT('Ctrl Pts',(1.75631083600175,1.,0.75400925402848));
#21517=CARTESIAN_POINT('Ctrl Pts',(1.7619781724032,1.,0.755220979975262));
#21518=CARTESIAN_POINT('Ctrl Pts',(1.76789396003141,1.,0.756421896028403));
#21519=CARTESIAN_POINT('Ctrl Pts',(1.77394167108342,1.,0.757578264077238));
#21520=CARTESIAN_POINT('Ctrl Pts',(1.77999411220912,1.,0.75865062667738));
#21521=CARTESIAN_POINT('Ctrl Pts',(1.78596964884526,1.,0.759614401109868));
#21522=CARTESIAN_POINT('Ctrl Pts',(1.79185815610802,1.,0.760469555880425));
#21523=CARTESIAN_POINT('Ctrl Pts',(1.79768986997735,1.,0.761229695230359));
#21524=CARTESIAN_POINT('Ctrl Pts',(1.80351583877334,1.,0.761915336443516));
#21525=CARTESIAN_POINT('Ctrl Pts',(1.80938551463989,1.,0.762546129464036));
#21526=CARTESIAN_POINT('Ctrl Pts',(1.81532118405566,1.,0.763132003836783));
#21527=CARTESIAN_POINT('Ctrl Pts',(1.82131873145297,1.,0.763673465462854));
#21528=CARTESIAN_POINT('Ctrl Pts',(1.8273599120008,1.,0.764165902606056));
#21529=CARTESIAN_POINT('Ctrl Pts',(1.8334207722714,1.,0.764602549687846));
#21530=CARTESIAN_POINT('Ctrl Pts',(1.83948181064823,1.,0.764978057881688));
#21531=CARTESIAN_POINT('Ctrl Pts',(1.8455369887591,1.,0.765291664861972));
#21532=CARTESIAN_POINT('Ctrl Pts',(1.85158945130054,1.,0.765545710619023));
#21533=CARTESIAN_POINT('Ctrl Pts',(1.85764741390391,1.,0.765744212909305));
#21534=CARTESIAN_POINT('Ctrl Pts',(1.86372027063314,1.,0.765891519092557));
#21535=CARTESIAN_POINT('Ctrl Pts',(1.86981398314345,1.,0.765990708546112));
#21536=CARTESIAN_POINT('Ctrl Pts',(1.87592888967886,1.,0.766042837036759));
#21537=CARTESIAN_POINT('Ctrl Pts',(1.88206215302561,1.,0.766047794851869));
#21538=CARTESIAN_POINT('Ctrl Pts',(1.88820926433409,1.,0.76600483706209));
#21539=CARTESIAN_POINT('Ctrl Pts',(1.89436577771389,1.,0.765913193856979));
#21540=CARTESIAN_POINT('Ctrl Pts',(1.90052930393599,1.,0.765772772593395));
#21541=CARTESIAN_POINT('Ctrl Pts',(1.90669961402362,1.,0.765584196937937));
#21542=CARTESIAN_POINT('Ctrl Pts',(1.91287765805174,1.,0.765348465884739));
#21543=CARTESIAN_POINT('Ctrl Pts',(1.91906491634197,1.,0.765066729667095));
#21544=CARTESIAN_POINT('Ctrl Pts',(1.92526263537041,1.,0.764740025488189));
#21545=CARTESIAN_POINT('Ctrl Pts',(1.93147105496367,1.,0.76436901067389));
#21546=CARTESIAN_POINT('Ctrl Pts',(1.93768964875867,1.,0.763954049121394));
#21547=CARTESIAN_POINT('Ctrl Pts',(1.94391746617626,1.,0.763495333538581));
#21548=CARTESIAN_POINT('Ctrl Pts',(1.95015342590025,1.,0.762992990878774));
#21549=CARTESIAN_POINT('Ctrl Pts',(1.95639665309893,1.,0.762447203806264));
#21550=CARTESIAN_POINT('Ctrl Pts',(1.96264672744229,1.,0.761858300014575));
#21551=CARTESIAN_POINT('Ctrl Pts',(1.96890351582545,1.,0.761226690483986));
#21552=CARTESIAN_POINT('Ctrl Pts',(1.97516705321521,1.,0.760552825409856));
#21553=CARTESIAN_POINT('Ctrl Pts',(1.98143741418156,1.,0.759837147452135));
#21554=CARTESIAN_POINT('Ctrl Pts',(1.98771456680806,1.,0.759080037802243));
#21555=CARTESIAN_POINT('Ctrl Pts',(1.9939983109871,1.,0.758281796766377));
#21556=CARTESIAN_POINT('Ctrl Pts',(2.00028834739072,1.,0.757442676862342));
#21557=CARTESIAN_POINT('Ctrl Pts',(2.00658431587682,1.,0.756562904646496));
#21558=CARTESIAN_POINT('Ctrl Pts',(2.01288584328149,1.,0.755642704958101));
#21559=CARTESIAN_POINT('Ctrl Pts',(2.01919259406003,1.,0.75468233072352));
#21560=CARTESIAN_POINT('Ctrl Pts',(2.02550428623587,1.,0.753682061113766));
#21561=CARTESIAN_POINT('Ctrl Pts',(2.03182068456467,1.,0.752642180488104));
#21562=CARTESIAN_POINT('Ctrl Pts',(2.03814160092173,1.,0.751562963361384));
#21563=CARTESIAN_POINT('Ctrl Pts',(2.04446689147754,1.,0.750444657874758));
#21564=CARTESIAN_POINT('Ctrl Pts',(2.05079645591606,1.,0.749287468663053));
#21565=CARTESIAN_POINT('Ctrl Pts',(2.05713023030263,1.,0.748091554181101));
#21566=CARTESIAN_POINT('Ctrl Pts',(2.06220058927162,1.,0.747103932785504));
#21567=CARTESIAN_POINT('Ctrl Pts',(2.06600523016401,1.,0.746345871542696));
#21568=CARTESIAN_POINT('Ctrl Pts',(2.06854248895575,1.,0.74583279137781));
#21569=CARTESIAN_POINT('Ctrl Pts',(2.0698113262342,1.,0.745574324794401));
#21570=CARTESIAN_POINT('',(1.60662857109684,0.,0.693717979106305));
#21571=CARTESIAN_POINT('Origin',(0.,0.,0.));
#21572=CARTESIAN_POINT('',(1.5055822144029,1.,0.892032620296856));
#21573=CARTESIAN_POINT('Origin',(0.,1.,0.));
#21574=CARTESIAN_POINT('',(1.5055822144029,0.,0.892032620296855));
#21575=CARTESIAN_POINT('Ctrl Pts',(1.81978687191668,-1.,1.23627494547115));
#21576=CARTESIAN_POINT('Ctrl Pts',(1.81978687191668,1.,1.23627494547115));
#21577=CARTESIAN_POINT('Ctrl Pts',(1.81925017193666,-1.,1.23509651170476));
#21578=CARTESIAN_POINT('Ctrl Pts',(1.81925017193666,1.,1.23509651170476));
#21579=CARTESIAN_POINT('Ctrl Pts',(1.81817389921279,-1.,1.2327422452705));
#21580=CARTESIAN_POINT('Ctrl Pts',(1.81817389921279,1.,1.2327422452705));
#21581=CARTESIAN_POINT('Ctrl Pts',(1.8165508718364,-1.,1.2292186489137));
#21582=CARTESIAN_POINT('Ctrl Pts',(1.8165508718364,1.,1.2292186489137));
#21583=CARTESIAN_POINT('Ctrl Pts',(1.81436959210434,-1.,1.2245361330495));
#21584=CARTESIAN_POINT('Ctrl Pts',(1.81436959210434,1.,1.2245361330495));
#21585=CARTESIAN_POINT('Ctrl Pts',(1.81161420806656,-1.,1.21870906103557));
#21586=CARTESIAN_POINT('Ctrl Pts',(1.81161420806656,1.,1.21870906103557));
#21587=CARTESIAN_POINT('Ctrl Pts',(1.80882996917129,-1.,1.21290815708314));
#21588=CARTESIAN_POINT('Ctrl Pts',(1.80882996917129,1.,1.21290815708314));
#21589=CARTESIAN_POINT('Ctrl Pts',(1.80601678480707,-1.,1.20713356605475));
#21590=CARTESIAN_POINT('Ctrl Pts',(1.80601678480707,1.,1.20713356605475));
#21591=CARTESIAN_POINT('Ctrl Pts',(1.80317454838603,-1.,1.20138548938974));
#21592=CARTESIAN_POINT('Ctrl Pts',(1.80317454838603,1.,1.20138548938974));
#21593=CARTESIAN_POINT('Ctrl Pts',(1.80030314369879,-1.,1.19566418930242));
#21594=CARTESIAN_POINT('Ctrl Pts',(1.80030314369879,1.,1.19566418930242));
#21595=CARTESIAN_POINT('Ctrl Pts',(1.79740245923478,-1.,1.18996997934445));
#21596=CARTESIAN_POINT('Ctrl Pts',(1.79740245923478,1.,1.18996997934445));
#21597=CARTESIAN_POINT('Ctrl Pts',(1.79447240321515,-1.,1.18430321697432));
#21598=CARTESIAN_POINT('Ctrl Pts',(1.79447240321515,1.,1.18430321697432));
#21599=CARTESIAN_POINT('Ctrl Pts',(1.79151291552689,-1.,1.17866429440809));
#21600=CARTESIAN_POINT('Ctrl Pts',(1.79151291552689,1.,1.17866429440809));
#21601=CARTESIAN_POINT('Ctrl Pts',(1.78852398877616,-1.,1.17305363177328));
#21602=CARTESIAN_POINT('Ctrl Pts',(1.78852398877616,1.,1.17305363177328));
#21603=CARTESIAN_POINT('Ctrl Pts',(1.78550566040443,-1.,1.16747166312303));
#21604=CARTESIAN_POINT('Ctrl Pts',(1.78550566040443,1.,1.16747166312303));
#21605=CARTESIAN_POINT('Ctrl Pts',(1.78245795881009,-1.,1.16191881298499));
#21606=CARTESIAN_POINT('Ctrl Pts',(1.78245795881009,1.,1.16191881298499));
#21607=CARTESIAN_POINT('Ctrl Pts',(1.77938085564275,-1.,1.15639547194698));
#21608=CARTESIAN_POINT('Ctrl Pts',(1.77938085564275,1.,1.15639547194698));
#21609=CARTESIAN_POINT('Ctrl Pts',(1.7762742255701,-1.,1.15090197841515));
#21610=CARTESIAN_POINT('Ctrl Pts',(1.7762742255701,1.,1.15090197841515));
#21611=CARTESIAN_POINT('Ctrl Pts',(1.77313777896194,-1.,1.1454385822692));
#21612=CARTESIAN_POINT('Ctrl Pts',(1.77313777896194,1.,1.1454385822692));
#21613=CARTESIAN_POINT('Ctrl Pts',(1.76997111386769,-1.,1.14000548336975));
#21614=CARTESIAN_POINT('Ctrl Pts',(1.76997111386769,1.,1.14000548336975));
#21615=CARTESIAN_POINT('Ctrl Pts',(1.76677384551862,-1.,1.1346029180462));
#21616=CARTESIAN_POINT('Ctrl Pts',(1.76677384551862,1.,1.1346029180462));
#21617=CARTESIAN_POINT('Ctrl Pts',(1.7635457196617,-1.,1.12923123555075));
#21618=CARTESIAN_POINT('Ctrl Pts',(1.7635457196617,1.,1.12923123555075));
#21619=CARTESIAN_POINT('Ctrl Pts',(1.76028671825096,-1.,1.12389096855086));
#21620=CARTESIAN_POINT('Ctrl Pts',(1.76028671825096,1.,1.12389096855086));
#21621=CARTESIAN_POINT('Ctrl Pts',(1.75699720772105,-1.,1.11858293216763));
#21622=CARTESIAN_POINT('Ctrl Pts',(1.75699720772105,1.,1.11858293216763));
#21623=CARTESIAN_POINT('Ctrl Pts',(1.7536777209463,-1.,1.11330807582551));
#21624=CARTESIAN_POINT('Ctrl Pts',(1.7536777209463,1.,1.11330807582551));
#21625=CARTESIAN_POINT('Ctrl Pts',(1.7503286607592,-1.,1.10806728183007));
#21626=CARTESIAN_POINT('Ctrl Pts',(1.7503286607592,1.,1.10806728183007));
#21627=CARTESIAN_POINT('Ctrl Pts',(1.74695004214923,-1.,1.10286118991143));
#21628=CARTESIAN_POINT('Ctrl Pts',(1.74695004214923,1.,1.10286118991143));
#21629=CARTESIAN_POINT('Ctrl Pts',(1.74354119236208,-1.,1.09768999241226));
#21630=CARTESIAN_POINT('Ctrl Pts',(1.74354119236208,1.,1.09768999241226));
#21631=CARTESIAN_POINT('Ctrl Pts',(1.74010053962247,-1.,1.09255329056493));
#21632=CARTESIAN_POINT('Ctrl Pts',(1.74010053962247,1.,1.09255329056493));
#21633=CARTESIAN_POINT('Ctrl Pts',(1.73662628326091,-1.,1.08745056285427));
#21634=CARTESIAN_POINT('Ctrl Pts',(1.73662628326091,1.,1.08745056285427));
#21635=CARTESIAN_POINT('Ctrl Pts',(1.73311705663407,-1.,1.08238162784749));
#21636=CARTESIAN_POINT('Ctrl Pts',(1.73311705663407,1.,1.08238162784749));
#21637=CARTESIAN_POINT('Ctrl Pts',(1.72957248977424,-1.,1.0773470373727));
#21638=CARTESIAN_POINT('Ctrl Pts',(1.72957248977424,1.,1.0773470373727));
#21639=CARTESIAN_POINT('Ctrl Pts',(1.72599406198488,-1.,1.07234866990252));
#21640=CARTESIAN_POINT('Ctrl Pts',(1.72599406198488,1.,1.07234866990252));
#21641=CARTESIAN_POINT('Ctrl Pts',(1.72238500928453,-1.,1.06738966975462));
#21642=CARTESIAN_POINT('Ctrl Pts',(1.72238500928453,1.,1.06738966975462));
#21643=CARTESIAN_POINT('Ctrl Pts',(1.71874858456904,-1.,1.06247324680647));
#21644=CARTESIAN_POINT('Ctrl Pts',(1.71874858456904,1.,1.06247324680647));
#21645=CARTESIAN_POINT('Ctrl Pts',(1.7150865442702,-1.,1.05760163192479));
#21646=CARTESIAN_POINT('Ctrl Pts',(1.7150865442702,1.,1.05760163192479));
#21647=CARTESIAN_POINT('Ctrl Pts',(1.71139783543989,-1.,1.05277517202855));
#21648=CARTESIAN_POINT('Ctrl Pts',(1.71139783543989,1.,1.05277517202855));
#21649=CARTESIAN_POINT('Ctrl Pts',(1.70767646263649,-1.,1.04799085404995));
#21650=CARTESIAN_POINT('Ctrl Pts',(1.70767646263649,1.,1.04799085404995));
#21651=CARTESIAN_POINT('Ctrl Pts',(1.70391338707982,-1.,1.04324363334554));
#21652=CARTESIAN_POINT('Ctrl Pts',(1.70391338707982,1.,1.04324363334554));
#21653=CARTESIAN_POINT('Ctrl Pts',(1.70010052930962,-1.,1.03852922490789));
#21654=CARTESIAN_POINT('Ctrl Pts',(1.70010052930962,1.,1.03852922490789));
#21655=CARTESIAN_POINT('Ctrl Pts',(1.69623414782771,-1.,1.03384646003588));
#21656=CARTESIAN_POINT('Ctrl Pts',(1.69623414782771,1.,1.03384646003588));
#21657=CARTESIAN_POINT('Ctrl Pts',(1.69231840863458,-1.,1.02919977579147));
#21658=CARTESIAN_POINT('Ctrl Pts',(1.69231840863458,1.,1.02919977579147));
#21659=CARTESIAN_POINT('Ctrl Pts',(1.68836910178447,-1.,1.02460180535255));
#21660=CARTESIAN_POINT('Ctrl Pts',(1.68836910178447,1.,1.02460180535255));
#21661=CARTESIAN_POINT('Ctrl Pts',(1.68440578021706,-1.,1.02006795074201));
#21662=CARTESIAN_POINT('Ctrl Pts',(1.68440578021706,1.,1.02006795074201));
#21663=CARTESIAN_POINT('Ctrl Pts',(1.68044289894798,-1.,1.01561026162773));
#21664=CARTESIAN_POINT('Ctrl Pts',(1.68044289894798,1.,1.01561026162773));
#21665=CARTESIAN_POINT('Ctrl Pts',(1.67648246776464,-1.,1.01123236493511));
#21666=CARTESIAN_POINT('Ctrl Pts',(1.67648246776464,1.,1.01123236493511));
#21667=CARTESIAN_POINT('Ctrl Pts',(1.67250335383293,-1.,1.00692206696414));
#21668=CARTESIAN_POINT('Ctrl Pts',(1.67250335383293,1.,1.00692206696414));
#21669=CARTESIAN_POINT('Ctrl Pts',(1.66846059277303,-1.,1.00265091003727));
#21670=CARTESIAN_POINT('Ctrl Pts',(1.66846059277303,1.,1.00265091003727));
#21671=CARTESIAN_POINT('Ctrl Pts',(1.66430758030376,-1.,0.998389654952758));
#21672=CARTESIAN_POINT('Ctrl Pts',(1.66430758030376,1.,0.998389654952758));
#21673=CARTESIAN_POINT('Ctrl Pts',(1.66001553809947,-1.,0.994121836661306));
#21674=CARTESIAN_POINT('Ctrl Pts',(1.66001553809947,1.,0.994121836661306));
#21675=CARTESIAN_POINT('Ctrl Pts',(1.65559044289699,-1.,0.989855627854165));
#21676=CARTESIAN_POINT('Ctrl Pts',(1.65559044289699,1.,0.989855627854165));
#21677=CARTESIAN_POINT('Ctrl Pts',(1.65110016612638,-1.,0.985642622920821));
#21678=CARTESIAN_POINT('Ctrl Pts',(1.65110016612638,1.,0.985642622920821));
#21679=CARTESIAN_POINT('Ctrl Pts',(1.64665139190656,-1.,0.981562530939489));
#21680=CARTESIAN_POINT('Ctrl Pts',(1.64665139190656,1.,0.981562530939489));
#21681=CARTESIAN_POINT('Ctrl Pts',(1.64233990826687,-1.,0.977689794119417));
#21682=CARTESIAN_POINT('Ctrl Pts',(1.64233990826687,1.,0.977689794119417));
#21683=CARTESIAN_POINT('Ctrl Pts',(1.63820952658144,-1.,0.974066058287419));
#21684=CARTESIAN_POINT('Ctrl Pts',(1.63820952658144,1.,0.974066058287419));
#21685=CARTESIAN_POINT('Ctrl Pts',(1.63420665729798,-1.,0.970669715997509));
#21686=CARTESIAN_POINT('Ctrl Pts',(1.63420665729798,1.,0.970669715997509));
#21687=CARTESIAN_POINT('Ctrl Pts',(1.63013849959461,-1.,0.967387853230345));
#21688=CARTESIAN_POINT('Ctrl Pts',(1.63013849959461,1.,0.967387853230345));
#21689=CARTESIAN_POINT('Ctrl Pts',(1.62571930670187,-1.,0.964046107040536));
#21690=CARTESIAN_POINT('Ctrl Pts',(1.62571930670187,1.,0.964046107040536));
#21691=CARTESIAN_POINT('Ctrl Pts',(1.62061638140221,-1.,0.960438326101729));
#21692=CARTESIAN_POINT('Ctrl Pts',(1.62061638140221,1.,0.960438326101729));
#21693=CARTESIAN_POINT('Ctrl Pts',(1.61449324337085,-1.,0.956354422920671));
#21694=CARTESIAN_POINT('Ctrl Pts',(1.61449324337085,1.,0.956354422920671));
#21695=CARTESIAN_POINT('Ctrl Pts',(1.60706069896936,-1.,0.951613284356035));
#21696=CARTESIAN_POINT('Ctrl Pts',(1.60706069896936,1.,0.951613284356035));
#21697=CARTESIAN_POINT('Ctrl Pts',(1.59810042043673,-1.,0.946078063315257));
#21698=CARTESIAN_POINT('Ctrl Pts',(1.59810042043673,1.,0.946078063315257));
#21699=CARTESIAN_POINT('Ctrl Pts',(1.58744937487176,-1.,0.939646377893399));
#21700=CARTESIAN_POINT('Ctrl Pts',(1.58744937487176,1.,0.939646377893399));
#21701=CARTESIAN_POINT('Ctrl Pts',(1.57499388382243,-1.,0.932246680108685));
#21702=CARTESIAN_POINT('Ctrl Pts',(1.57499388382243,1.,0.932246680108685));
#21703=CARTESIAN_POINT('Ctrl Pts',(1.56065988578893,-1.,0.923832188944341));
#21704=CARTESIAN_POINT('Ctrl Pts',(1.56065988578893,1.,0.923832188944341));
#21705=CARTESIAN_POINT('Ctrl Pts',(1.54440491149498,-1.,0.914375919026456));
#21706=CARTESIAN_POINT('Ctrl Pts',(1.54440491149498,1.,0.914375919026456));
#21707=CARTESIAN_POINT('Ctrl Pts',(1.52984849887993,-1.,0.905967409625651));
#21708=CARTESIAN_POINT('Ctrl Pts',(1.52984849887993,1.,0.905967409625651));
#21709=CARTESIAN_POINT('Ctrl Pts',(1.51805569590094,-1.,0.899185047483511));
#21710=CARTESIAN_POINT('Ctrl Pts',(1.51805569590094,1.,0.899185047483511));
#21711=CARTESIAN_POINT('Ctrl Pts',(1.50980486806688,-1.,0.894452006964544));
#21712=CARTESIAN_POINT('Ctrl Pts',(1.50980486806688,1.,0.894452006964544));
#21713=CARTESIAN_POINT('Ctrl Pts',(1.5055822144029,-1.,0.892032620296856));
#21714=CARTESIAN_POINT('Ctrl Pts',(1.5055822144029,1.,0.892032620296856));
#21715=CARTESIAN_POINT('',(1.81978687191668,1.,1.23627494547115));
#21716=CARTESIAN_POINT('Ctrl Pts',(1.81978687191668,1.,1.23627494547115));
#21717=CARTESIAN_POINT('Ctrl Pts',(1.81925017193666,1.,1.23509651170476));
#21718=CARTESIAN_POINT('Ctrl Pts',(1.81817389921279,1.,1.2327422452705));
#21719=CARTESIAN_POINT('Ctrl Pts',(1.8165508718364,1.,1.2292186489137));
#21720=CARTESIAN_POINT('Ctrl Pts',(1.81436959210434,1.,1.2245361330495));
#21721=CARTESIAN_POINT('Ctrl Pts',(1.81161420806656,1.,1.21870906103557));
#21722=CARTESIAN_POINT('Ctrl Pts',(1.80882996917129,1.,1.21290815708314));
#21723=CARTESIAN_POINT('Ctrl Pts',(1.80601678480707,1.,1.20713356605475));
#21724=CARTESIAN_POINT('Ctrl Pts',(1.80317454838603,1.,1.20138548938974));
#21725=CARTESIAN_POINT('Ctrl Pts',(1.80030314369879,1.,1.19566418930242));
#21726=CARTESIAN_POINT('Ctrl Pts',(1.79740245923478,1.,1.18996997934445));
#21727=CARTESIAN_POINT('Ctrl Pts',(1.79447240321515,1.,1.18430321697432));
#21728=CARTESIAN_POINT('Ctrl Pts',(1.79151291552689,1.,1.17866429440809));
#21729=CARTESIAN_POINT('Ctrl Pts',(1.78852398877616,1.,1.17305363177328));
#21730=CARTESIAN_POINT('Ctrl Pts',(1.78550566040443,1.,1.16747166312303));
#21731=CARTESIAN_POINT('Ctrl Pts',(1.78245795881009,1.,1.16191881298499));
#21732=CARTESIAN_POINT('Ctrl Pts',(1.77938085564275,1.,1.15639547194698));
#21733=CARTESIAN_POINT('Ctrl Pts',(1.7762742255701,1.,1.15090197841515));
#21734=CARTESIAN_POINT('Ctrl Pts',(1.77313777896194,1.,1.1454385822692));
#21735=CARTESIAN_POINT('Ctrl Pts',(1.76997111386769,1.,1.14000548336975));
#21736=CARTESIAN_POINT('Ctrl Pts',(1.76677384551862,1.,1.1346029180462));
#21737=CARTESIAN_POINT('Ctrl Pts',(1.7635457196617,1.,1.12923123555075));
#21738=CARTESIAN_POINT('Ctrl Pts',(1.76028671825096,1.,1.12389096855086));
#21739=CARTESIAN_POINT('Ctrl Pts',(1.75699720772105,1.,1.11858293216763));
#21740=CARTESIAN_POINT('Ctrl Pts',(1.7536777209463,1.,1.11330807582551));
#21741=CARTESIAN_POINT('Ctrl Pts',(1.7503286607592,1.,1.10806728183007));
#21742=CARTESIAN_POINT('Ctrl Pts',(1.74695004214923,1.,1.10286118991143));
#21743=CARTESIAN_POINT('Ctrl Pts',(1.74354119236208,1.,1.09768999241226));
#21744=CARTESIAN_POINT('Ctrl Pts',(1.74010053962247,1.,1.09255329056493));
#21745=CARTESIAN_POINT('Ctrl Pts',(1.73662628326091,1.,1.08745056285427));
#21746=CARTESIAN_POINT('Ctrl Pts',(1.73311705663407,1.,1.08238162784749));
#21747=CARTESIAN_POINT('Ctrl Pts',(1.72957248977424,1.,1.0773470373727));
#21748=CARTESIAN_POINT('Ctrl Pts',(1.72599406198488,1.,1.07234866990252));
#21749=CARTESIAN_POINT('Ctrl Pts',(1.72238500928453,1.,1.06738966975462));
#21750=CARTESIAN_POINT('Ctrl Pts',(1.71874858456904,1.,1.06247324680647));
#21751=CARTESIAN_POINT('Ctrl Pts',(1.7150865442702,1.,1.05760163192479));
#21752=CARTESIAN_POINT('Ctrl Pts',(1.71139783543989,1.,1.05277517202855));
#21753=CARTESIAN_POINT('Ctrl Pts',(1.70767646263649,1.,1.04799085404995));
#21754=CARTESIAN_POINT('Ctrl Pts',(1.70391338707982,1.,1.04324363334554));
#21755=CARTESIAN_POINT('Ctrl Pts',(1.70010052930962,1.,1.03852922490789));
#21756=CARTESIAN_POINT('Ctrl Pts',(1.69623414782771,1.,1.03384646003588));
#21757=CARTESIAN_POINT('Ctrl Pts',(1.69231840863458,1.,1.02919977579147));
#21758=CARTESIAN_POINT('Ctrl Pts',(1.68836910178447,1.,1.02460180535255));
#21759=CARTESIAN_POINT('Ctrl Pts',(1.68440578021706,1.,1.02006795074201));
#21760=CARTESIAN_POINT('Ctrl Pts',(1.68044289894798,1.,1.01561026162773));
#21761=CARTESIAN_POINT('Ctrl Pts',(1.67648246776464,1.,1.01123236493511));
#21762=CARTESIAN_POINT('Ctrl Pts',(1.67250335383293,1.,1.00692206696414));
#21763=CARTESIAN_POINT('Ctrl Pts',(1.66846059277303,1.,1.00265091003727));
#21764=CARTESIAN_POINT('Ctrl Pts',(1.66430758030376,1.,0.998389654952758));
#21765=CARTESIAN_POINT('Ctrl Pts',(1.66001553809947,1.,0.994121836661306));
#21766=CARTESIAN_POINT('Ctrl Pts',(1.65559044289699,1.,0.989855627854165));
#21767=CARTESIAN_POINT('Ctrl Pts',(1.65110016612638,1.,0.985642622920821));
#21768=CARTESIAN_POINT('Ctrl Pts',(1.64665139190656,1.,0.981562530939489));
#21769=CARTESIAN_POINT('Ctrl Pts',(1.64233990826687,1.,0.977689794119417));
#21770=CARTESIAN_POINT('Ctrl Pts',(1.63820952658144,1.,0.974066058287419));
#21771=CARTESIAN_POINT('Ctrl Pts',(1.63420665729798,1.,0.970669715997509));
#21772=CARTESIAN_POINT('Ctrl Pts',(1.63013849959461,1.,0.967387853230345));
#21773=CARTESIAN_POINT('Ctrl Pts',(1.62571930670187,1.,0.964046107040536));
#21774=CARTESIAN_POINT('Ctrl Pts',(1.62061638140221,1.,0.960438326101729));
#21775=CARTESIAN_POINT('Ctrl Pts',(1.61449324337085,1.,0.956354422920671));
#21776=CARTESIAN_POINT('Ctrl Pts',(1.60706069896936,1.,0.951613284356035));
#21777=CARTESIAN_POINT('Ctrl Pts',(1.59810042043673,1.,0.946078063315257));
#21778=CARTESIAN_POINT('Ctrl Pts',(1.58744937487176,1.,0.939646377893399));
#21779=CARTESIAN_POINT('Ctrl Pts',(1.57499388382243,1.,0.932246680108685));
#21780=CARTESIAN_POINT('Ctrl Pts',(1.56065988578893,1.,0.923832188944341));
#21781=CARTESIAN_POINT('Ctrl Pts',(1.54440491149498,1.,0.914375919026456));
#21782=CARTESIAN_POINT('Ctrl Pts',(1.52984849887993,1.,0.905967409625651));
#21783=CARTESIAN_POINT('Ctrl Pts',(1.51805569590094,1.,0.899185047483511));
#21784=CARTESIAN_POINT('Ctrl Pts',(1.50980486806688,1.,0.894452006964544));
#21785=CARTESIAN_POINT('Ctrl Pts',(1.5055822144029,1.,0.892032620296856));
#21786=CARTESIAN_POINT('',(1.81978687191668,0.,1.23627494547115));
#21787=CARTESIAN_POINT('Origin',(1.73811241238545,0.,1.34869019493419));
#21788=CARTESIAN_POINT('',(1.73811241238545,1.,1.34869019493419));
#21789=CARTESIAN_POINT('',(1.81978687191668,1.,1.23627494547115));
#21790=CARTESIAN_POINT('',(1.73811241238545,0.,1.34869019493419));
#21791=CARTESIAN_POINT('Ctrl Pts',(1.31362392696032,-1.,1.15624053661742));
#21792=CARTESIAN_POINT('Ctrl Pts',(1.31362392696032,1.,1.15624053661742));
#21793=CARTESIAN_POINT('Ctrl Pts',(1.31722977216397,-1.,1.15950888730809));
#21794=CARTESIAN_POINT('Ctrl Pts',(1.31722977216397,1.,1.15950888730809));
#21795=CARTESIAN_POINT('Ctrl Pts',(1.32428080721772,-1.,1.16589330093588));
#21796=CARTESIAN_POINT('Ctrl Pts',(1.32428080721772,1.,1.16589330093588));
#21797=CARTESIAN_POINT('Ctrl Pts',(1.33437539347008,-1.,1.17501305789857));
#21798=CARTESIAN_POINT('Ctrl Pts',(1.33437539347008,1.,1.17501305789857));
#21799=CARTESIAN_POINT('Ctrl Pts',(1.34687054001093,-1.,1.18625865667441));
#21800=CARTESIAN_POINT('Ctrl Pts',(1.34687054001093,1.,1.18625865667441));
#21801=CARTESIAN_POINT('Ctrl Pts',(1.36088705043885,-1.,1.1987959077932));
#21802=CARTESIAN_POINT('Ctrl Pts',(1.36088705043885,1.,1.1987959077932));
#21803=CARTESIAN_POINT('Ctrl Pts',(1.37331915607905,-1.,1.20982812925645));
#21804=CARTESIAN_POINT('Ctrl Pts',(1.37331915607905,1.,1.20982812925645));
#21805=CARTESIAN_POINT('Ctrl Pts',(1.38420564527715,-1.,1.21938737280852));
#21806=CARTESIAN_POINT('Ctrl Pts',(1.38420564527715,1.,1.21938737280852));
#21807=CARTESIAN_POINT('Ctrl Pts',(1.39361389568796,-1.,1.22752961899387));
#21808=CARTESIAN_POINT('Ctrl Pts',(1.39361389568796,1.,1.22752961899387));
#21809=CARTESIAN_POINT('Ctrl Pts',(1.40164708206106,-1.,1.23434087290423));
#21810=CARTESIAN_POINT('Ctrl Pts',(1.40164708206106,1.,1.23434087290423));
#21811=CARTESIAN_POINT('Ctrl Pts',(1.40845295531283,-1.,1.23994455029534));
#21812=CARTESIAN_POINT('Ctrl Pts',(1.40845295531283,1.,1.23994455029534));
#21813=CARTESIAN_POINT('Ctrl Pts',(1.41422913175179,-1.,1.24450600513056));
#21814=CARTESIAN_POINT('Ctrl Pts',(1.41422913175179,1.,1.24450600513056));
#21815=CARTESIAN_POINT('Ctrl Pts',(1.41923722596025,-1.,1.24824430986571));
#21816=CARTESIAN_POINT('Ctrl Pts',(1.41923722596025,1.,1.24824430986571));
#21817=CARTESIAN_POINT('Ctrl Pts',(1.42378102115575,-1.,1.2514145557001));
#21818=CARTESIAN_POINT('Ctrl Pts',(1.42378102115575,1.,1.2514145557001));
#21819=CARTESIAN_POINT('Ctrl Pts',(1.42815938799387,-1.,1.25426945222639));
#21820=CARTESIAN_POINT('Ctrl Pts',(1.42815938799387,1.,1.25426945222639));
#21821=CARTESIAN_POINT('Ctrl Pts',(1.43262645609691,-1.,1.25702687965755));
#21822=CARTESIAN_POINT('Ctrl Pts',(1.43262645609691,1.,1.25702687965755));
#21823=CARTESIAN_POINT('Ctrl Pts',(1.43734919180847,-1.,1.25983531012005));
#21824=CARTESIAN_POINT('Ctrl Pts',(1.43734919180847,1.,1.25983531012005));
#21825=CARTESIAN_POINT('Ctrl Pts',(1.44236470511303,-1.,1.26273903323859));
#21826=CARTESIAN_POINT('Ctrl Pts',(1.44236470511303,1.,1.26273903323859));
#21827=CARTESIAN_POINT('Ctrl Pts',(1.44761985001662,-1.,1.26570925118868));
#21828=CARTESIAN_POINT('Ctrl Pts',(1.44761985001662,1.,1.26570925118868));
#21829=CARTESIAN_POINT('Ctrl Pts',(1.45301422764247,-1.,1.2686778680489));
#21830=CARTESIAN_POINT('Ctrl Pts',(1.45301422764247,1.,1.2686778680489));
#21831=CARTESIAN_POINT('Ctrl Pts',(1.45843906294697,-1.,1.27156805265289));
#21832=CARTESIAN_POINT('Ctrl Pts',(1.45843906294697,1.,1.27156805265289));
#21833=CARTESIAN_POINT('Ctrl Pts',(1.46382431332476,-1.,1.27433119897822));
#21834=CARTESIAN_POINT('Ctrl Pts',(1.46382431332476,1.,1.27433119897822));
#21835=CARTESIAN_POINT('Ctrl Pts',(1.46916035917133,-1.,1.2769641483109));
#21836=CARTESIAN_POINT('Ctrl Pts',(1.46916035917133,1.,1.2769641483109));
#21837=CARTESIAN_POINT('Ctrl Pts',(1.4744717526707,-1.,1.2794891824849));
#21838=CARTESIAN_POINT('Ctrl Pts',(1.4744717526707,1.,1.2794891824849));
#21839=CARTESIAN_POINT('Ctrl Pts',(1.47980070347095,-1.,1.28194158939517));
#21840=CARTESIAN_POINT('Ctrl Pts',(1.47980070347095,1.,1.28194158939517));
#21841=CARTESIAN_POINT('Ctrl Pts',(1.4851881711891,-1.,1.28435533880201));
#21842=CARTESIAN_POINT('Ctrl Pts',(1.4851881711891,1.,1.28435533880201));
#21843=CARTESIAN_POINT('Ctrl Pts',(1.4906522831278,-1.,1.2867467611644));
#21844=CARTESIAN_POINT('Ctrl Pts',(1.4906522831278,1.,1.2867467611644));
#21845=CARTESIAN_POINT('Ctrl Pts',(1.49618896881754,-1.,1.28911506584254));
#21846=CARTESIAN_POINT('Ctrl Pts',(1.49618896881754,1.,1.28911506584254));
#21847=CARTESIAN_POINT('Ctrl Pts',(1.50178230149776,-1.,1.29145022885181));
#21848=CARTESIAN_POINT('Ctrl Pts',(1.50178230149776,1.,1.29145022885181));
#21849=CARTESIAN_POINT('Ctrl Pts',(1.50741159078365,-1.,1.29373841372842));
#21850=CARTESIAN_POINT('Ctrl Pts',(1.50741159078365,1.,1.29373841372842));
#21851=CARTESIAN_POINT('Ctrl Pts',(1.51305994241402,-1.,1.29596850710509));
#21852=CARTESIAN_POINT('Ctrl Pts',(1.51305994241402,1.,1.29596850710509));
#21853=CARTESIAN_POINT('Ctrl Pts',(1.51872184912724,-1.,1.29813791800747));
#21854=CARTESIAN_POINT('Ctrl Pts',(1.51872184912724,1.,1.29813791800747));
#21855=CARTESIAN_POINT('Ctrl Pts',(1.52439957861062,-1.,1.30024984366328));
#21856=CARTESIAN_POINT('Ctrl Pts',(1.52439957861062,1.,1.30024984366328));
#21857=CARTESIAN_POINT('Ctrl Pts',(1.53009970283891,-1.,1.30231064395568));
#21858=CARTESIAN_POINT('Ctrl Pts',(1.53009970283891,1.,1.30231064395568));
#21859=CARTESIAN_POINT('Ctrl Pts',(1.53582981268977,-1.,1.30432735639489));
#21860=CARTESIAN_POINT('Ctrl Pts',(1.53582981268977,1.,1.30432735639489));
#21861=CARTESIAN_POINT('Ctrl Pts',(1.54159462645432,-1.,1.30630475189556));
#21862=CARTESIAN_POINT('Ctrl Pts',(1.54159462645432,1.,1.30630475189556));
#21863=CARTESIAN_POINT('Ctrl Pts',(1.54739413957185,-1.,1.30824393907473));
#21864=CARTESIAN_POINT('Ctrl Pts',(1.54739413957185,1.,1.30824393907473));
#21865=CARTESIAN_POINT('Ctrl Pts',(1.55322568759481,-1.,1.31014393684222));
#21866=CARTESIAN_POINT('Ctrl Pts',(1.55322568759481,1.,1.31014393684222));
#21867=CARTESIAN_POINT('Ctrl Pts',(1.55908521254821,-1.,1.31200264341696));
#21868=CARTESIAN_POINT('Ctrl Pts',(1.55908521254821,1.,1.31200264341696));
#21869=CARTESIAN_POINT('Ctrl Pts',(1.56496872402353,-1.,1.31381795281002));
#21870=CARTESIAN_POINT('Ctrl Pts',(1.56496872402353,1.,1.31381795281002));
#21871=CARTESIAN_POINT('Ctrl Pts',(1.57087397835723,-1.,1.31558903860016));
#21872=CARTESIAN_POINT('Ctrl Pts',(1.57087397835723,1.,1.31558903860016));
#21873=CARTESIAN_POINT('Ctrl Pts',(1.5768005650559,-1.,1.31731642317187));
#21874=CARTESIAN_POINT('Ctrl Pts',(1.5768005650559,1.,1.31731642317187));
#21875=CARTESIAN_POINT('Ctrl Pts',(1.58274907898834,-1.,1.31900135021432));
#21876=CARTESIAN_POINT('Ctrl Pts',(1.58274907898834,1.,1.31900135021432));
#21877=CARTESIAN_POINT('Ctrl Pts',(1.58872057258245,-1.,1.32064537110892));
#21878=CARTESIAN_POINT('Ctrl Pts',(1.58872057258245,1.,1.32064537110892));
#21879=CARTESIAN_POINT('Ctrl Pts',(1.59471591079403,-1.,1.32224985747682));
#21880=CARTESIAN_POINT('Ctrl Pts',(1.59471591079403,1.,1.32224985747682));
#21881=CARTESIAN_POINT('Ctrl Pts',(1.60073511858687,-1.,1.32381550858256));
#21882=CARTESIAN_POINT('Ctrl Pts',(1.60073511858687,1.,1.32381550858256));
#21883=CARTESIAN_POINT('Ctrl Pts',(1.60677758290954,-1.,1.32534250785782));
#21884=CARTESIAN_POINT('Ctrl Pts',(1.60677758290954,1.,1.32534250785782));
#21885=CARTESIAN_POINT('Ctrl Pts',(1.6128423401575,-1.,1.32683074483356));
#21886=CARTESIAN_POINT('Ctrl Pts',(1.6128423401575,1.,1.32683074483356));
#21887=CARTESIAN_POINT('Ctrl Pts',(1.61892832270724,-1.,1.32828000610449));
#21888=CARTESIAN_POINT('Ctrl Pts',(1.61892832270724,1.,1.32828000610449));
#21889=CARTESIAN_POINT('Ctrl Pts',(1.62503464209797,-1.,1.3296901950568));
#21890=CARTESIAN_POINT('Ctrl Pts',(1.62503464209797,1.,1.3296901950568));
#21891=CARTESIAN_POINT('Ctrl Pts',(1.63116079730923,-1.,1.33106149345645));
#21892=CARTESIAN_POINT('Ctrl Pts',(1.63116079730923,1.,1.33106149345645));
#21893=CARTESIAN_POINT('Ctrl Pts',(1.63730653475089,-1.,1.33239425103724));
#21894=CARTESIAN_POINT('Ctrl Pts',(1.63730653475089,1.,1.33239425103724));
#21895=CARTESIAN_POINT('Ctrl Pts',(1.6434717485603,-1.,1.33368890676572));
#21896=CARTESIAN_POINT('Ctrl Pts',(1.6434717485603,1.,1.33368890676572));
#21897=CARTESIAN_POINT('Ctrl Pts',(1.6496563728683,-1.,1.33494590467993));
#21898=CARTESIAN_POINT('Ctrl Pts',(1.6496563728683,1.,1.33494590467993));
#21899=CARTESIAN_POINT('Ctrl Pts',(1.65586025952593,-1.,1.33616559745172));
#21900=CARTESIAN_POINT('Ctrl Pts',(1.65586025952593,1.,1.33616559745172));
#21901=CARTESIAN_POINT('Ctrl Pts',(1.66208312541983,-1.,1.33734820885262));
#21902=CARTESIAN_POINT('Ctrl Pts',(1.66208312541983,1.,1.33734820885262));
#21903=CARTESIAN_POINT('Ctrl Pts',(1.66832460783989,-1.,1.33849388654388));
#21904=CARTESIAN_POINT('Ctrl Pts',(1.66832460783989,1.,1.33849388654388));
#21905=CARTESIAN_POINT('Ctrl Pts',(1.67458429426086,-1.,1.3396027347034));
#21906=CARTESIAN_POINT('Ctrl Pts',(1.67458429426086,1.,1.3396027347034));
#21907=CARTESIAN_POINT('Ctrl Pts',(1.68086176030362,-1.,1.34067485185203));
#21908=CARTESIAN_POINT('Ctrl Pts',(1.68086176030362,1.,1.34067485185203));
#21909=CARTESIAN_POINT('Ctrl Pts',(1.68715660868764,-1.,1.341710374848));
#21910=CARTESIAN_POINT('Ctrl Pts',(1.68715660868764,1.,1.341710374848));
#21911=CARTESIAN_POINT('Ctrl Pts',(1.6934684849687,-1.,1.34270948206319));
#21912=CARTESIAN_POINT('Ctrl Pts',(1.6934684849687,1.,1.34270948206319));
#21913=CARTESIAN_POINT('Ctrl Pts',(1.69979707754427,-1.,1.34367237124483));
#21914=CARTESIAN_POINT('Ctrl Pts',(1.69979707754427,1.,1.34367237124483));
#21915=CARTESIAN_POINT('Ctrl Pts',(1.70614212266738,-1.,1.34459924533831));
#21916=CARTESIAN_POINT('Ctrl Pts',(1.70614212266738,1.,1.34459924533831));
#21917=CARTESIAN_POINT('Ctrl Pts',(1.71250340686822,-1.,1.34549029589416));
#21918=CARTESIAN_POINT('Ctrl Pts',(1.71250340686822,1.,1.34549029589416));
#21919=CARTESIAN_POINT('Ctrl Pts',(1.7188807715049,-1.,1.34634568653227));
#21920=CARTESIAN_POINT('Ctrl Pts',(1.7188807715049,1.,1.34634568653227));
#21921=CARTESIAN_POINT('Ctrl Pts',(1.72527410680674,-1.,1.34716554819527));
#21922=CARTESIAN_POINT('Ctrl Pts',(1.72527410680674,1.,1.34716554819527));
#21923=CARTESIAN_POINT('Ctrl Pts',(1.7304014965394,-1.,1.34779309152035));
#21924=CARTESIAN_POINT('Ctrl Pts',(1.7304014965394,1.,1.34779309152035));
#21925=CARTESIAN_POINT('Ctrl Pts',(1.73425417885907,-1.,1.34824783112887));
#21926=CARTESIAN_POINT('Ctrl Pts',(1.73425417885907,1.,1.34824783112887));
#21927=CARTESIAN_POINT('Ctrl Pts',(1.73682580585691,-1.,1.34854391898045));
#21928=CARTESIAN_POINT('Ctrl Pts',(1.73682580585691,1.,1.34854391898045));
#21929=CARTESIAN_POINT('Ctrl Pts',(1.73811241238545,-1.,1.34869019493419));
#21930=CARTESIAN_POINT('Ctrl Pts',(1.73811241238545,1.,1.34869019493419));
#21931=CARTESIAN_POINT('',(1.31362392696032,1.,1.15624053661742));
#21932=CARTESIAN_POINT('Ctrl Pts',(1.31362392696032,1.,1.15624053661742));
#21933=CARTESIAN_POINT('Ctrl Pts',(1.31722977216397,1.,1.15950888730809));
#21934=CARTESIAN_POINT('Ctrl Pts',(1.32428080721772,1.,1.16589330093588));
#21935=CARTESIAN_POINT('Ctrl Pts',(1.33437539347008,1.,1.17501305789857));
#21936=CARTESIAN_POINT('Ctrl Pts',(1.34687054001093,1.,1.18625865667441));
#21937=CARTESIAN_POINT('Ctrl Pts',(1.36088705043885,1.,1.1987959077932));
#21938=CARTESIAN_POINT('Ctrl Pts',(1.37331915607905,1.,1.20982812925645));
#21939=CARTESIAN_POINT('Ctrl Pts',(1.38420564527715,1.,1.21938737280852));
#21940=CARTESIAN_POINT('Ctrl Pts',(1.39361389568796,1.,1.22752961899387));
#21941=CARTESIAN_POINT('Ctrl Pts',(1.40164708206106,1.,1.23434087290423));
#21942=CARTESIAN_POINT('Ctrl Pts',(1.40845295531283,1.,1.23994455029534));
#21943=CARTESIAN_POINT('Ctrl Pts',(1.41422913175179,1.,1.24450600513056));
#21944=CARTESIAN_POINT('Ctrl Pts',(1.41923722596025,1.,1.24824430986571));
#21945=CARTESIAN_POINT('Ctrl Pts',(1.42378102115575,1.,1.2514145557001));
#21946=CARTESIAN_POINT('Ctrl Pts',(1.42815938799387,1.,1.25426945222639));
#21947=CARTESIAN_POINT('Ctrl Pts',(1.43262645609691,1.,1.25702687965755));
#21948=CARTESIAN_POINT('Ctrl Pts',(1.43734919180847,1.,1.25983531012005));
#21949=CARTESIAN_POINT('Ctrl Pts',(1.44236470511303,1.,1.26273903323859));
#21950=CARTESIAN_POINT('Ctrl Pts',(1.44761985001662,1.,1.26570925118868));
#21951=CARTESIAN_POINT('Ctrl Pts',(1.45301422764247,1.,1.2686778680489));
#21952=CARTESIAN_POINT('Ctrl Pts',(1.45843906294697,1.,1.27156805265289));
#21953=CARTESIAN_POINT('Ctrl Pts',(1.46382431332476,1.,1.27433119897822));
#21954=CARTESIAN_POINT('Ctrl Pts',(1.46916035917133,1.,1.2769641483109));
#21955=CARTESIAN_POINT('Ctrl Pts',(1.4744717526707,1.,1.2794891824849));
#21956=CARTESIAN_POINT('Ctrl Pts',(1.47980070347095,1.,1.28194158939517));
#21957=CARTESIAN_POINT('Ctrl Pts',(1.4851881711891,1.,1.28435533880201));
#21958=CARTESIAN_POINT('Ctrl Pts',(1.4906522831278,1.,1.2867467611644));
#21959=CARTESIAN_POINT('Ctrl Pts',(1.49618896881754,1.,1.28911506584254));
#21960=CARTESIAN_POINT('Ctrl Pts',(1.50178230149776,1.,1.29145022885181));
#21961=CARTESIAN_POINT('Ctrl Pts',(1.50741159078365,1.,1.29373841372842));
#21962=CARTESIAN_POINT('Ctrl Pts',(1.51305994241402,1.,1.29596850710509));
#21963=CARTESIAN_POINT('Ctrl Pts',(1.51872184912724,1.,1.29813791800747));
#21964=CARTESIAN_POINT('Ctrl Pts',(1.52439957861062,1.,1.30024984366328));
#21965=CARTESIAN_POINT('Ctrl Pts',(1.53009970283891,1.,1.30231064395568));
#21966=CARTESIAN_POINT('Ctrl Pts',(1.53582981268977,1.,1.30432735639489));
#21967=CARTESIAN_POINT('Ctrl Pts',(1.54159462645432,1.,1.30630475189556));
#21968=CARTESIAN_POINT('Ctrl Pts',(1.54739413957185,1.,1.30824393907473));
#21969=CARTESIAN_POINT('Ctrl Pts',(1.55322568759481,1.,1.31014393684222));
#21970=CARTESIAN_POINT('Ctrl Pts',(1.55908521254821,1.,1.31200264341696));
#21971=CARTESIAN_POINT('Ctrl Pts',(1.56496872402353,1.,1.31381795281002));
#21972=CARTESIAN_POINT('Ctrl Pts',(1.57087397835723,1.,1.31558903860016));
#21973=CARTESIAN_POINT('Ctrl Pts',(1.5768005650559,1.,1.31731642317187));
#21974=CARTESIAN_POINT('Ctrl Pts',(1.58274907898834,1.,1.31900135021432));
#21975=CARTESIAN_POINT('Ctrl Pts',(1.58872057258245,1.,1.32064537110892));
#21976=CARTESIAN_POINT('Ctrl Pts',(1.59471591079403,1.,1.32224985747682));
#21977=CARTESIAN_POINT('Ctrl Pts',(1.60073511858687,1.,1.32381550858256));
#21978=CARTESIAN_POINT('Ctrl Pts',(1.60677758290954,1.,1.32534250785782));
#21979=CARTESIAN_POINT('Ctrl Pts',(1.6128423401575,1.,1.32683074483356));
#21980=CARTESIAN_POINT('Ctrl Pts',(1.61892832270724,1.,1.32828000610449));
#21981=CARTESIAN_POINT('Ctrl Pts',(1.62503464209797,1.,1.3296901950568));
#21982=CARTESIAN_POINT('Ctrl Pts',(1.63116079730923,1.,1.33106149345645));
#21983=CARTESIAN_POINT('Ctrl Pts',(1.63730653475089,1.,1.33239425103724));
#21984=CARTESIAN_POINT('Ctrl Pts',(1.6434717485603,1.,1.33368890676572));
#21985=CARTESIAN_POINT('Ctrl Pts',(1.6496563728683,1.,1.33494590467993));
#21986=CARTESIAN_POINT('Ctrl Pts',(1.65586025952593,1.,1.33616559745172));
#21987=CARTESIAN_POINT('Ctrl Pts',(1.66208312541983,1.,1.33734820885262));
#21988=CARTESIAN_POINT('Ctrl Pts',(1.66832460783989,1.,1.33849388654388));
#21989=CARTESIAN_POINT('Ctrl Pts',(1.67458429426086,1.,1.3396027347034));
#21990=CARTESIAN_POINT('Ctrl Pts',(1.68086176030362,1.,1.34067485185203));
#21991=CARTESIAN_POINT('Ctrl Pts',(1.68715660868764,1.,1.341710374848));
#21992=CARTESIAN_POINT('Ctrl Pts',(1.6934684849687,1.,1.34270948206319));
#21993=CARTESIAN_POINT('Ctrl Pts',(1.69979707754427,1.,1.34367237124483));
#21994=CARTESIAN_POINT('Ctrl Pts',(1.70614212266738,1.,1.34459924533831));
#21995=CARTESIAN_POINT('Ctrl Pts',(1.71250340686822,1.,1.34549029589416));
#21996=CARTESIAN_POINT('Ctrl Pts',(1.7188807715049,1.,1.34634568653227));
#21997=CARTESIAN_POINT('Ctrl Pts',(1.72527410680674,1.,1.34716554819527));
#21998=CARTESIAN_POINT('Ctrl Pts',(1.7304014965394,1.,1.34779309152035));
#21999=CARTESIAN_POINT('Ctrl Pts',(1.73425417885907,1.,1.34824783112887));
#22000=CARTESIAN_POINT('Ctrl Pts',(1.73682580585691,1.,1.34854391898045));
#22001=CARTESIAN_POINT('Ctrl Pts',(1.73811241238545,1.,1.34869019493419));
#22002=CARTESIAN_POINT('',(1.31362392696032,0.,1.15624053661742));
#22003=CARTESIAN_POINT('Origin',(0.,0.,0.));
#22004=CARTESIAN_POINT('',(1.15624053661742,1.,1.31362392696033));
#22005=CARTESIAN_POINT('Origin',(0.,1.,0.));
#22006=CARTESIAN_POINT('',(1.15624053661742,0.,1.31362392696032));
#22007=CARTESIAN_POINT('Ctrl Pts',(1.34869019493419,-1.,1.73811241238545));
#22008=CARTESIAN_POINT('Ctrl Pts',(1.34869019493419,1.,1.73811241238545));
#22009=CARTESIAN_POINT('Ctrl Pts',(1.34854391898145,-1.,1.73682580585819));
#22010=CARTESIAN_POINT('Ctrl Pts',(1.34854391898145,1.,1.73682580585819));
#22011=CARTESIAN_POINT('Ctrl Pts',(1.34824783113158,-1.,1.73425417886255));
#22012=CARTESIAN_POINT('Ctrl Pts',(1.34824783113158,1.,1.73425417886255));
#22013=CARTESIAN_POINT('Ctrl Pts',(1.3477930915247,-1.,1.73040149654497));
#22014=CARTESIAN_POINT('Ctrl Pts',(1.3477930915247,1.,1.73040149654497));
#22015=CARTESIAN_POINT('Ctrl Pts',(1.34716554820013,-1.,1.72527410681298));
#22016=CARTESIAN_POINT('Ctrl Pts',(1.34716554820013,1.,1.72527410681298));
#22017=CARTESIAN_POINT('Ctrl Pts',(1.34634568653586,-1.,1.7188807715095));
#22018=CARTESIAN_POINT('Ctrl Pts',(1.34634568653586,1.,1.7188807715095));
#22019=CARTESIAN_POINT('Ctrl Pts',(1.34549029589563,-1.,1.71250340687011));
#22020=CARTESIAN_POINT('Ctrl Pts',(1.34549029589563,1.,1.71250340687011));
#22021=CARTESIAN_POINT('Ctrl Pts',(1.34459924533783,-1.,1.70614212266676));
#22022=CARTESIAN_POINT('Ctrl Pts',(1.34459924533783,1.,1.70614212266676));
#22023=CARTESIAN_POINT('Ctrl Pts',(1.34367237124322,-1.,1.69979707754221));
#22024=CARTESIAN_POINT('Ctrl Pts',(1.34367237124322,1.,1.69979707754221));
#22025=CARTESIAN_POINT('Ctrl Pts',(1.34270948206139,-1.,1.6934684849664));
#22026=CARTESIAN_POINT('Ctrl Pts',(1.34270948206139,1.,1.6934684849664));
#22027=CARTESIAN_POINT('Ctrl Pts',(1.34171037484673,-1.,1.68715660868602));
#22028=CARTESIAN_POINT('Ctrl Pts',(1.34171037484673,1.,1.68715660868602));
#22029=CARTESIAN_POINT('Ctrl Pts',(1.3406748518516,-1.,1.68086176030308));
#22030=CARTESIAN_POINT('Ctrl Pts',(1.3406748518516,1.,1.68086176030308));
#22031=CARTESIAN_POINT('Ctrl Pts',(1.33960273470372,-1.,1.67458429426126));
#22032=CARTESIAN_POINT('Ctrl Pts',(1.33960273470372,1.,1.67458429426126));
#22033=CARTESIAN_POINT('Ctrl Pts',(1.33849388654458,-1.,1.66832460784078));
#22034=CARTESIAN_POINT('Ctrl Pts',(1.33849388654458,1.,1.66832460784078));
#22035=CARTESIAN_POINT('Ctrl Pts',(1.33734820885331,-1.,1.66208312542073));
#22036=CARTESIAN_POINT('Ctrl Pts',(1.33734820885331,1.,1.66208312542073));
#22037=CARTESIAN_POINT('Ctrl Pts',(1.33616559745217,-1.,1.65586025952651));
#22038=CARTESIAN_POINT('Ctrl Pts',(1.33616559745217,1.,1.65586025952651));
#22039=CARTESIAN_POINT('Ctrl Pts',(1.33494590468003,-1.,1.64965637286843));
#22040=CARTESIAN_POINT('Ctrl Pts',(1.33494590468003,1.,1.64965637286843));
#22041=CARTESIAN_POINT('Ctrl Pts',(1.33368890676554,-1.,1.64347174856007));
#22042=CARTESIAN_POINT('Ctrl Pts',(1.33368890676554,1.,1.64347174856007));
#22043=CARTESIAN_POINT('Ctrl Pts',(1.33239425103694,-1.,1.6373065347505));
#22044=CARTESIAN_POINT('Ctrl Pts',(1.33239425103694,1.,1.6373065347505));
#22045=CARTESIAN_POINT('Ctrl Pts',(1.33106149345618,-1.,1.63116079730887));
#22046=CARTESIAN_POINT('Ctrl Pts',(1.33106149345618,1.,1.63116079730887));
#22047=CARTESIAN_POINT('Ctrl Pts',(1.32969019505665,-1.,1.62503464209777));
#22048=CARTESIAN_POINT('Ctrl Pts',(1.32969019505665,1.,1.62503464209777));
#22049=CARTESIAN_POINT('Ctrl Pts',(1.32828000610448,-1.,1.61892832270723));
#22050=CARTESIAN_POINT('Ctrl Pts',(1.32828000610448,1.,1.61892832270723));
#22051=CARTESIAN_POINT('Ctrl Pts',(1.32683074483365,-1.,1.61284234015762));
#22052=CARTESIAN_POINT('Ctrl Pts',(1.32683074483365,1.,1.61284234015762));
#22053=CARTESIAN_POINT('Ctrl Pts',(1.32534250785794,-1.,1.6067775829097));
#22054=CARTESIAN_POINT('Ctrl Pts',(1.32534250785794,1.,1.6067775829097));
#22055=CARTESIAN_POINT('Ctrl Pts',(1.32381550858266,-1.,1.600735118587));
#22056=CARTESIAN_POINT('Ctrl Pts',(1.32381550858266,1.,1.600735118587));
#22057=CARTESIAN_POINT('Ctrl Pts',(1.32224985747686,-1.,1.59471591079408));
#22058=CARTESIAN_POINT('Ctrl Pts',(1.32224985747686,1.,1.59471591079408));
#22059=CARTESIAN_POINT('Ctrl Pts',(1.32064537110891,-1.,1.58872057258244));
#22060=CARTESIAN_POINT('Ctrl Pts',(1.32064537110891,1.,1.58872057258244));
#22061=CARTESIAN_POINT('Ctrl Pts',(1.31900135021428,-1.,1.58274907898829));
#22062=CARTESIAN_POINT('Ctrl Pts',(1.31900135021428,1.,1.58274907898829));
#22063=CARTESIAN_POINT('Ctrl Pts',(1.31731642317183,-1.,1.57680056505585));
#22064=CARTESIAN_POINT('Ctrl Pts',(1.31731642317183,1.,1.57680056505585));
#22065=CARTESIAN_POINT('Ctrl Pts',(1.31558903860015,-1.,1.57087397835721));
#22066=CARTESIAN_POINT('Ctrl Pts',(1.31558903860015,1.,1.57087397835721));
#22067=CARTESIAN_POINT('Ctrl Pts',(1.31381795281002,-1.,1.56496872402352));
#22068=CARTESIAN_POINT('Ctrl Pts',(1.31381795281002,1.,1.56496872402352));
#22069=CARTESIAN_POINT('Ctrl Pts',(1.31200264341696,-1.,1.55908521254822));
#22070=CARTESIAN_POINT('Ctrl Pts',(1.31200264341696,1.,1.55908521254822));
#22071=CARTESIAN_POINT('Ctrl Pts',(1.31014393684221,-1.,1.55322568759481));
#22072=CARTESIAN_POINT('Ctrl Pts',(1.31014393684221,1.,1.55322568759481));
#22073=CARTESIAN_POINT('Ctrl Pts',(1.30824393907471,-1.,1.54739413957183));
#22074=CARTESIAN_POINT('Ctrl Pts',(1.30824393907471,1.,1.54739413957183));
#22075=CARTESIAN_POINT('Ctrl Pts',(1.30630475189553,-1.,1.54159462645428));
#22076=CARTESIAN_POINT('Ctrl Pts',(1.30630475189553,1.,1.54159462645428));
#22077=CARTESIAN_POINT('Ctrl Pts',(1.30432735639487,-1.,1.53582981268976));
#22078=CARTESIAN_POINT('Ctrl Pts',(1.30432735639487,1.,1.53582981268976));
#22079=CARTESIAN_POINT('Ctrl Pts',(1.3023106439557,-1.,1.53009970283893));
#22080=CARTESIAN_POINT('Ctrl Pts',(1.3023106439557,1.,1.53009970283893));
#22081=CARTESIAN_POINT('Ctrl Pts',(1.30024984366334,-1.,1.5243995786107));
#22082=CARTESIAN_POINT('Ctrl Pts',(1.30024984366334,1.,1.5243995786107));
#22083=CARTESIAN_POINT('Ctrl Pts',(1.29813791800757,-1.,1.51872184912735));
#22084=CARTESIAN_POINT('Ctrl Pts',(1.29813791800757,1.,1.51872184912735));
#22085=CARTESIAN_POINT('Ctrl Pts',(1.29596850710518,-1.,1.51305994241412));
#22086=CARTESIAN_POINT('Ctrl Pts',(1.29596850710518,1.,1.51305994241412));
#22087=CARTESIAN_POINT('Ctrl Pts',(1.29373841372843,-1.,1.50741159078367));
#22088=CARTESIAN_POINT('Ctrl Pts',(1.29373841372843,1.,1.50741159078367));
#22089=CARTESIAN_POINT('Ctrl Pts',(1.29145022885171,-1.,1.50178230149764));
#22090=CARTESIAN_POINT('Ctrl Pts',(1.29145022885171,1.,1.50178230149764));
#22091=CARTESIAN_POINT('Ctrl Pts',(1.28911506584232,-1.,1.49618896881729));
#22092=CARTESIAN_POINT('Ctrl Pts',(1.28911506584232,1.,1.49618896881729));
#22093=CARTESIAN_POINT('Ctrl Pts',(1.28674676116415,-1.,1.4906522831275));
#22094=CARTESIAN_POINT('Ctrl Pts',(1.28674676116415,1.,1.4906522831275));
#22095=CARTESIAN_POINT('Ctrl Pts',(1.28435533880184,-1.,1.48518817118891));
#22096=CARTESIAN_POINT('Ctrl Pts',(1.28435533880184,1.,1.48518817118891));
#22097=CARTESIAN_POINT('Ctrl Pts',(1.28194158939522,-1.,1.47980070347102));
#22098=CARTESIAN_POINT('Ctrl Pts',(1.28194158939522,1.,1.47980070347102));
#22099=CARTESIAN_POINT('Ctrl Pts',(1.27948918248524,-1.,1.4744717526711));
#22100=CARTESIAN_POINT('Ctrl Pts',(1.27948918248524,1.,1.4744717526711));
#22101=CARTESIAN_POINT('Ctrl Pts',(1.27696414831144,-1.,1.46916035917197));
#22102=CARTESIAN_POINT('Ctrl Pts',(1.27696414831144,1.,1.46916035917197));
#22103=CARTESIAN_POINT('Ctrl Pts',(1.27433119897877,-1.,1.4638243133254));
#22104=CARTESIAN_POINT('Ctrl Pts',(1.27433119897877,1.,1.4638243133254));
#22105=CARTESIAN_POINT('Ctrl Pts',(1.27156805265312,-1.,1.45843906294725));
#22106=CARTESIAN_POINT('Ctrl Pts',(1.27156805265312,1.,1.45843906294725));
#22107=CARTESIAN_POINT('Ctrl Pts',(1.26867786804854,-1.,1.45301422764205));
#22108=CARTESIAN_POINT('Ctrl Pts',(1.26867786804854,1.,1.45301422764205));
#22109=CARTESIAN_POINT('Ctrl Pts',(1.26570925118767,-1.,1.44761985001544));
#22110=CARTESIAN_POINT('Ctrl Pts',(1.26570925118767,1.,1.44761985001544));
#22111=CARTESIAN_POINT('Ctrl Pts',(1.26273903323723,-1.,1.44236470511145));
#22112=CARTESIAN_POINT('Ctrl Pts',(1.26273903323723,1.,1.44236470511145));
#22113=CARTESIAN_POINT('Ctrl Pts',(1.25983531011894,-1.,1.43734919180719));
#22114=CARTESIAN_POINT('Ctrl Pts',(1.25983531011894,1.,1.43734919180719));
#22115=CARTESIAN_POINT('Ctrl Pts',(1.25702687965744,-1.,1.43262645609679));
#22116=CARTESIAN_POINT('Ctrl Pts',(1.25702687965744,1.,1.43262645609679));
#22117=CARTESIAN_POINT('Ctrl Pts',(1.25426945222783,-1.,1.42815938799555));
#22118=CARTESIAN_POINT('Ctrl Pts',(1.25426945222783,1.,1.42815938799555));
#22119=CARTESIAN_POINT('Ctrl Pts',(1.25141455570299,-1.,1.42378102115911));
#22120=CARTESIAN_POINT('Ctrl Pts',(1.25141455570299,1.,1.42378102115911));
#22121=CARTESIAN_POINT('Ctrl Pts',(1.24824430986911,-1.,1.41923722596421));
#22122=CARTESIAN_POINT('Ctrl Pts',(1.24824430986911,1.,1.41923722596421));
#22123=CARTESIAN_POINT('Ctrl Pts',(1.24450600513278,-1.,1.41422913175437));
#22124=CARTESIAN_POINT('Ctrl Pts',(1.24450600513278,1.,1.41422913175437));
#22125=CARTESIAN_POINT('Ctrl Pts',(1.23994455029421,-1.,1.40845295531151));
#22126=CARTESIAN_POINT('Ctrl Pts',(1.23994455029421,1.,1.40845295531151));
#22127=CARTESIAN_POINT('Ctrl Pts',(1.23434087289768,-1.,1.40164708205345));
#22128=CARTESIAN_POINT('Ctrl Pts',(1.23434087289768,1.,1.40164708205345));
#22129=CARTESIAN_POINT('Ctrl Pts',(1.22752961898063,-1.,1.39361389567257));
#22130=CARTESIAN_POINT('Ctrl Pts',(1.22752961898063,1.,1.39361389567257));
#22131=CARTESIAN_POINT('Ctrl Pts',(1.21938737278853,-1.,1.38420564525391));
#22132=CARTESIAN_POINT('Ctrl Pts',(1.21938737278853,1.,1.38420564525391));
#22133=CARTESIAN_POINT('Ctrl Pts',(1.20982812923113,-1.,1.37331915604962));
#22134=CARTESIAN_POINT('Ctrl Pts',(1.20982812923113,1.,1.37331915604962));
#22135=CARTESIAN_POINT('Ctrl Pts',(1.1987959077656,-1.,1.36088705040677));
#22136=CARTESIAN_POINT('Ctrl Pts',(1.1987959077656,1.,1.36088705040677));
#22137=CARTESIAN_POINT('Ctrl Pts',(1.18625865664915,-1.,1.34687053998157));
#22138=CARTESIAN_POINT('Ctrl Pts',(1.18625865664915,1.,1.34687053998157));
#22139=CARTESIAN_POINT('Ctrl Pts',(1.17501305787994,-1.,1.33437539344842));
#22140=CARTESIAN_POINT('Ctrl Pts',(1.17501305787994,1.,1.33437539344842));
#22141=CARTESIAN_POINT('Ctrl Pts',(1.16589330092532,-1.,1.32428080720544));
#22142=CARTESIAN_POINT('Ctrl Pts',(1.16589330092532,1.,1.32428080720544));
#22143=CARTESIAN_POINT('Ctrl Pts',(1.15950888730433,-1.,1.3172297721596));
#22144=CARTESIAN_POINT('Ctrl Pts',(1.15950888730433,1.,1.3172297721596));
#22145=CARTESIAN_POINT('Ctrl Pts',(1.15624053661742,-1.,1.31362392696033));
#22146=CARTESIAN_POINT('Ctrl Pts',(1.15624053661742,1.,1.31362392696033));
#22147=CARTESIAN_POINT('',(1.34869019493419,1.,1.73811241238545));
#22148=CARTESIAN_POINT('Ctrl Pts',(1.34869019493419,1.,1.73811241238545));
#22149=CARTESIAN_POINT('Ctrl Pts',(1.34854391898145,1.,1.73682580585819));
#22150=CARTESIAN_POINT('Ctrl Pts',(1.34824783113158,1.,1.73425417886255));
#22151=CARTESIAN_POINT('Ctrl Pts',(1.3477930915247,1.,1.73040149654497));
#22152=CARTESIAN_POINT('Ctrl Pts',(1.34716554820013,1.,1.72527410681298));
#22153=CARTESIAN_POINT('Ctrl Pts',(1.34634568653586,1.,1.7188807715095));
#22154=CARTESIAN_POINT('Ctrl Pts',(1.34549029589563,1.,1.71250340687011));
#22155=CARTESIAN_POINT('Ctrl Pts',(1.34459924533783,1.,1.70614212266676));
#22156=CARTESIAN_POINT('Ctrl Pts',(1.34367237124322,1.,1.69979707754221));
#22157=CARTESIAN_POINT('Ctrl Pts',(1.34270948206139,1.,1.6934684849664));
#22158=CARTESIAN_POINT('Ctrl Pts',(1.34171037484673,1.,1.68715660868602));
#22159=CARTESIAN_POINT('Ctrl Pts',(1.3406748518516,1.,1.68086176030308));
#22160=CARTESIAN_POINT('Ctrl Pts',(1.33960273470372,1.,1.67458429426126));
#22161=CARTESIAN_POINT('Ctrl Pts',(1.33849388654458,1.,1.66832460784078));
#22162=CARTESIAN_POINT('Ctrl Pts',(1.33734820885331,1.,1.66208312542073));
#22163=CARTESIAN_POINT('Ctrl Pts',(1.33616559745217,1.,1.65586025952651));
#22164=CARTESIAN_POINT('Ctrl Pts',(1.33494590468003,1.,1.64965637286843));
#22165=CARTESIAN_POINT('Ctrl Pts',(1.33368890676554,1.,1.64347174856007));
#22166=CARTESIAN_POINT('Ctrl Pts',(1.33239425103694,1.,1.6373065347505));
#22167=CARTESIAN_POINT('Ctrl Pts',(1.33106149345618,1.,1.63116079730887));
#22168=CARTESIAN_POINT('Ctrl Pts',(1.32969019505665,1.,1.62503464209777));
#22169=CARTESIAN_POINT('Ctrl Pts',(1.32828000610448,1.,1.61892832270723));
#22170=CARTESIAN_POINT('Ctrl Pts',(1.32683074483365,1.,1.61284234015762));
#22171=CARTESIAN_POINT('Ctrl Pts',(1.32534250785794,1.,1.6067775829097));
#22172=CARTESIAN_POINT('Ctrl Pts',(1.32381550858266,1.,1.600735118587));
#22173=CARTESIAN_POINT('Ctrl Pts',(1.32224985747686,1.,1.59471591079408));
#22174=CARTESIAN_POINT('Ctrl Pts',(1.32064537110891,1.,1.58872057258244));
#22175=CARTESIAN_POINT('Ctrl Pts',(1.31900135021428,1.,1.58274907898829));
#22176=CARTESIAN_POINT('Ctrl Pts',(1.31731642317183,1.,1.57680056505585));
#22177=CARTESIAN_POINT('Ctrl Pts',(1.31558903860015,1.,1.57087397835721));
#22178=CARTESIAN_POINT('Ctrl Pts',(1.31381795281002,1.,1.56496872402352));
#22179=CARTESIAN_POINT('Ctrl Pts',(1.31200264341696,1.,1.55908521254822));
#22180=CARTESIAN_POINT('Ctrl Pts',(1.31014393684221,1.,1.55322568759481));
#22181=CARTESIAN_POINT('Ctrl Pts',(1.30824393907471,1.,1.54739413957183));
#22182=CARTESIAN_POINT('Ctrl Pts',(1.30630475189553,1.,1.54159462645428));
#22183=CARTESIAN_POINT('Ctrl Pts',(1.30432735639487,1.,1.53582981268976));
#22184=CARTESIAN_POINT('Ctrl Pts',(1.3023106439557,1.,1.53009970283893));
#22185=CARTESIAN_POINT('Ctrl Pts',(1.30024984366334,1.,1.5243995786107));
#22186=CARTESIAN_POINT('Ctrl Pts',(1.29813791800757,1.,1.51872184912735));
#22187=CARTESIAN_POINT('Ctrl Pts',(1.29596850710518,1.,1.51305994241412));
#22188=CARTESIAN_POINT('Ctrl Pts',(1.29373841372843,1.,1.50741159078367));
#22189=CARTESIAN_POINT('Ctrl Pts',(1.29145022885171,1.,1.50178230149764));
#22190=CARTESIAN_POINT('Ctrl Pts',(1.28911506584232,1.,1.49618896881729));
#22191=CARTESIAN_POINT('Ctrl Pts',(1.28674676116415,1.,1.4906522831275));
#22192=CARTESIAN_POINT('Ctrl Pts',(1.28435533880184,1.,1.48518817118891));
#22193=CARTESIAN_POINT('Ctrl Pts',(1.28194158939522,1.,1.47980070347102));
#22194=CARTESIAN_POINT('Ctrl Pts',(1.27948918248524,1.,1.4744717526711));
#22195=CARTESIAN_POINT('Ctrl Pts',(1.27696414831144,1.,1.46916035917197));
#22196=CARTESIAN_POINT('Ctrl Pts',(1.27433119897877,1.,1.4638243133254));
#22197=CARTESIAN_POINT('Ctrl Pts',(1.27156805265312,1.,1.45843906294725));
#22198=CARTESIAN_POINT('Ctrl Pts',(1.26867786804854,1.,1.45301422764205));
#22199=CARTESIAN_POINT('Ctrl Pts',(1.26570925118767,1.,1.44761985001544));
#22200=CARTESIAN_POINT('Ctrl Pts',(1.26273903323723,1.,1.44236470511145));
#22201=CARTESIAN_POINT('Ctrl Pts',(1.25983531011894,1.,1.43734919180719));
#22202=CARTESIAN_POINT('Ctrl Pts',(1.25702687965744,1.,1.43262645609679));
#22203=CARTESIAN_POINT('Ctrl Pts',(1.25426945222783,1.,1.42815938799555));
#22204=CARTESIAN_POINT('Ctrl Pts',(1.25141455570299,1.,1.42378102115911));
#22205=CARTESIAN_POINT('Ctrl Pts',(1.24824430986911,1.,1.41923722596421));
#22206=CARTESIAN_POINT('Ctrl Pts',(1.24450600513278,1.,1.41422913175437));
#22207=CARTESIAN_POINT('Ctrl Pts',(1.23994455029421,1.,1.40845295531151));
#22208=CARTESIAN_POINT('Ctrl Pts',(1.23434087289768,1.,1.40164708205345));
#22209=CARTESIAN_POINT('Ctrl Pts',(1.22752961898063,1.,1.39361389567257));
#22210=CARTESIAN_POINT('Ctrl Pts',(1.21938737278853,1.,1.38420564525391));
#22211=CARTESIAN_POINT('Ctrl Pts',(1.20982812923113,1.,1.37331915604962));
#22212=CARTESIAN_POINT('Ctrl Pts',(1.1987959077656,1.,1.36088705040677));
#22213=CARTESIAN_POINT('Ctrl Pts',(1.18625865664915,1.,1.34687053998157));
#22214=CARTESIAN_POINT('Ctrl Pts',(1.17501305787994,1.,1.33437539344842));
#22215=CARTESIAN_POINT('Ctrl Pts',(1.16589330092532,1.,1.32428080720544));
#22216=CARTESIAN_POINT('Ctrl Pts',(1.15950888730433,1.,1.3172297721596));
#22217=CARTESIAN_POINT('Ctrl Pts',(1.15624053661742,1.,1.31362392696033));
#22218=CARTESIAN_POINT('',(1.34869019493419,0.,1.73811241238545));
#22219=CARTESIAN_POINT('Origin',(1.23627494547115,0.,1.81978687191668));
#22220=CARTESIAN_POINT('',(1.23627494547115,1.,1.81978687191668));
#22221=CARTESIAN_POINT('',(1.34869019493419,1.,1.73811241238545));
#22222=CARTESIAN_POINT('',(1.23627494547115,0.,1.81978687191668));
#22223=CARTESIAN_POINT('Ctrl Pts',(0.892032620296855,-1.,1.5055822144029));
#22224=CARTESIAN_POINT('Ctrl Pts',(0.892032620296855,1.,1.5055822144029));
#22225=CARTESIAN_POINT('Ctrl Pts',(0.894452006967538,-1.,1.50980486807181));
#22226=CARTESIAN_POINT('Ctrl Pts',(0.894452006967538,1.,1.50980486807181));
#22227=CARTESIAN_POINT('Ctrl Pts',(0.89918504749193,-1.,1.51805569591479));
#22228=CARTESIAN_POINT('Ctrl Pts',(0.89918504749193,1.,1.51805569591479));
#22229=CARTESIAN_POINT('Ctrl Pts',(0.905967409640498,-1.,1.52984849890434));
#22230=CARTESIAN_POINT('Ctrl Pts',(0.905967409640498,1.,1.52984849890434));
#22231=CARTESIAN_POINT('Ctrl Pts',(0.914375919046579,-1.,1.54440491152808));
#22232=CARTESIAN_POINT('Ctrl Pts',(0.914375919046579,1.,1.54440491152808));
#22233=CARTESIAN_POINT('Ctrl Pts',(0.923832188966322,-1.,1.56065988582509));
#22234=CARTESIAN_POINT('Ctrl Pts',(0.923832188966322,1.,1.56065988582509));
#22235=CARTESIAN_POINT('Ctrl Pts',(0.932246680128848,-1.,1.57499388385561));
#22236=CARTESIAN_POINT('Ctrl Pts',(0.932246680128848,1.,1.57499388385561));
#22237=CARTESIAN_POINT('Ctrl Pts',(0.939646377909319,-1.,1.58744937489796));
#22238=CARTESIAN_POINT('Ctrl Pts',(0.939646377909319,1.,1.58744937489796));
#22239=CARTESIAN_POINT('Ctrl Pts',(0.946078063325795,-1.,1.59810042045408));
#22240=CARTESIAN_POINT('Ctrl Pts',(0.946078063325795,1.,1.59810042045408));
#22241=CARTESIAN_POINT('Ctrl Pts',(0.951613284361247,-1.,1.60706069897794));
#22242=CARTESIAN_POINT('Ctrl Pts',(0.951613284361247,1.,1.60706069897794));
#22243=CARTESIAN_POINT('Ctrl Pts',(0.956354422921572,-1.,1.61449324337233));
#22244=CARTESIAN_POINT('Ctrl Pts',(0.956354422921572,1.,1.61449324337233));
#22245=CARTESIAN_POINT('Ctrl Pts',(0.960438326099958,-1.,1.62061638139929));
#22246=CARTESIAN_POINT('Ctrl Pts',(0.960438326099958,1.,1.62061638139929));
#22247=CARTESIAN_POINT('Ctrl Pts',(0.964046107037821,-1.,1.6257193066974));
#22248=CARTESIAN_POINT('Ctrl Pts',(0.964046107037821,1.,1.6257193066974));
#22249=CARTESIAN_POINT('Ctrl Pts',(0.967387853228041,-1.,1.63013849959083));
#22250=CARTESIAN_POINT('Ctrl Pts',(0.967387853228041,1.,1.63013849959083));
#22251=CARTESIAN_POINT('Ctrl Pts',(0.970669715996356,-1.,1.63420665729609));
#22252=CARTESIAN_POINT('Ctrl Pts',(0.970669715996356,1.,1.63420665729609));
#22253=CARTESIAN_POINT('Ctrl Pts',(0.974066058287501,-1.,1.63820952658157));
#22254=CARTESIAN_POINT('Ctrl Pts',(0.974066058287501,1.,1.63820952658157));
#22255=CARTESIAN_POINT('Ctrl Pts',(0.977689794120296,-1.,1.64233990826831));
#22256=CARTESIAN_POINT('Ctrl Pts',(0.977689794120296,1.,1.64233990826831));
#22257=CARTESIAN_POINT('Ctrl Pts',(0.981562530940574,-1.,1.64665139190834));
#22258=CARTESIAN_POINT('Ctrl Pts',(0.981562530940574,1.,1.64665139190834));
#22259=CARTESIAN_POINT('Ctrl Pts',(0.985642622921626,-1.,1.6511001661277));
#22260=CARTESIAN_POINT('Ctrl Pts',(0.985642622921626,1.,1.6511001661277));
#22261=CARTESIAN_POINT('Ctrl Pts',(0.98985562785445,-1.,1.65559044289746));
#22262=CARTESIAN_POINT('Ctrl Pts',(0.98985562785445,1.,1.65559044289746));
#22263=CARTESIAN_POINT('Ctrl Pts',(0.994121836661115,-1.,1.66001553809916));
#22264=CARTESIAN_POINT('Ctrl Pts',(0.994121836661115,1.,1.66001553809916));
#22265=CARTESIAN_POINT('Ctrl Pts',(0.998389654952317,-1.,1.66430758030304));
#22266=CARTESIAN_POINT('Ctrl Pts',(0.998389654952317,1.,1.66430758030304));
#22267=CARTESIAN_POINT('Ctrl Pts',(1.00265091003682,-1.,1.66846059277231));
#22268=CARTESIAN_POINT('Ctrl Pts',(1.00265091003682,1.,1.66846059277231));
#22269=CARTESIAN_POINT('Ctrl Pts',(1.00692206696387,-1.,1.67250335383248));
#22270=CARTESIAN_POINT('Ctrl Pts',(1.00692206696387,1.,1.67250335383248));
#22271=CARTESIAN_POINT('Ctrl Pts',(1.01123236493507,-1.,1.67648246776457));
#22272=CARTESIAN_POINT('Ctrl Pts',(1.01123236493507,1.,1.67648246776457));
#22273=CARTESIAN_POINT('Ctrl Pts',(1.01561026162786,-1.,1.6804428989482));
#22274=CARTESIAN_POINT('Ctrl Pts',(1.01561026162786,1.,1.6804428989482));
#22275=CARTESIAN_POINT('Ctrl Pts',(1.02006795074222,-1.,1.68440578021739));
#22276=CARTESIAN_POINT('Ctrl Pts',(1.02006795074222,1.,1.68440578021739));
#22277=CARTESIAN_POINT('Ctrl Pts',(1.02460180535272,-1.,1.68836910178475));
#22278=CARTESIAN_POINT('Ctrl Pts',(1.02460180535272,1.,1.68836910178475));
#22279=CARTESIAN_POINT('Ctrl Pts',(1.02919977579155,-1.,1.69231840863471));
#22280=CARTESIAN_POINT('Ctrl Pts',(1.02919977579155,1.,1.69231840863471));
#22281=CARTESIAN_POINT('Ctrl Pts',(1.03384646003587,-1.,1.69623414782769));
#22282=CARTESIAN_POINT('Ctrl Pts',(1.03384646003587,1.,1.69623414782769));
#22283=CARTESIAN_POINT('Ctrl Pts',(1.03852922490782,-1.,1.70010052930951));
#22284=CARTESIAN_POINT('Ctrl Pts',(1.03852922490782,1.,1.70010052930951));
#22285=CARTESIAN_POINT('Ctrl Pts',(1.04324363334546,-1.,1.70391338707969));
#22286=CARTESIAN_POINT('Ctrl Pts',(1.04324363334546,1.,1.70391338707969));
#22287=CARTESIAN_POINT('Ctrl Pts',(1.0479908540499,-1.,1.70767646263641));
#22288=CARTESIAN_POINT('Ctrl Pts',(1.0479908540499,1.,1.70767646263641));
#22289=CARTESIAN_POINT('Ctrl Pts',(1.05277517202853,-1.,1.71139783543986));
#22290=CARTESIAN_POINT('Ctrl Pts',(1.05277517202853,1.,1.71139783543986));
#22291=CARTESIAN_POINT('Ctrl Pts',(1.05760163192481,-1.,1.71508654427022));
#22292=CARTESIAN_POINT('Ctrl Pts',(1.05760163192481,1.,1.71508654427022));
#22293=CARTESIAN_POINT('Ctrl Pts',(1.06247324680649,-1.,1.71874858456908));
#22294=CARTESIAN_POINT('Ctrl Pts',(1.06247324680649,1.,1.71874858456908));
#22295=CARTESIAN_POINT('Ctrl Pts',(1.06738966975463,-1.,1.72238500928456));
#22296=CARTESIAN_POINT('Ctrl Pts',(1.06738966975463,1.,1.72238500928456));
#22297=CARTESIAN_POINT('Ctrl Pts',(1.07234866990252,-1.,1.72599406198489));
#22298=CARTESIAN_POINT('Ctrl Pts',(1.07234866990252,1.,1.72599406198489));
#22299=CARTESIAN_POINT('Ctrl Pts',(1.0773470373727,-1.,1.72957248977424));
#22300=CARTESIAN_POINT('Ctrl Pts',(1.0773470373727,1.,1.72957248977424));
#22301=CARTESIAN_POINT('Ctrl Pts',(1.08238162784749,-1.,1.73311705663407));
#22302=CARTESIAN_POINT('Ctrl Pts',(1.08238162784749,1.,1.73311705663407));
#22303=CARTESIAN_POINT('Ctrl Pts',(1.08745056285429,-1.,1.73662628326093));
#22304=CARTESIAN_POINT('Ctrl Pts',(1.08745056285429,1.,1.73662628326093));
#22305=CARTESIAN_POINT('Ctrl Pts',(1.09255329056496,-1.,1.74010053962252));
#22306=CARTESIAN_POINT('Ctrl Pts',(1.09255329056496,1.,1.74010053962252));
#22307=CARTESIAN_POINT('Ctrl Pts',(1.09768999241229,-1.,1.74354119236212));
#22308=CARTESIAN_POINT('Ctrl Pts',(1.09768999241229,1.,1.74354119236212));
#22309=CARTESIAN_POINT('Ctrl Pts',(1.10286118991144,-1.,1.74695004214924));
#22310=CARTESIAN_POINT('Ctrl Pts',(1.10286118991144,1.,1.74695004214924));
#22311=CARTESIAN_POINT('Ctrl Pts',(1.10806728183003,-1.,1.75032866075914));
#22312=CARTESIAN_POINT('Ctrl Pts',(1.10806728183003,1.,1.75032866075914));
#22313=CARTESIAN_POINT('Ctrl Pts',(1.11330807582542,-1.,1.75367772094617));
#22314=CARTESIAN_POINT('Ctrl Pts',(1.11330807582542,1.,1.75367772094617));
#22315=CARTESIAN_POINT('Ctrl Pts',(1.11858293216752,-1.,1.75699720772089));
#22316=CARTESIAN_POINT('Ctrl Pts',(1.11858293216752,1.,1.75699720772089));
#22317=CARTESIAN_POINT('Ctrl Pts',(1.12389096855078,-1.,1.76028671825084));
#22318=CARTESIAN_POINT('Ctrl Pts',(1.12389096855078,1.,1.76028671825084));
#22319=CARTESIAN_POINT('Ctrl Pts',(1.12923123555076,-1.,1.76354571966171));
#22320=CARTESIAN_POINT('Ctrl Pts',(1.12923123555076,1.,1.76354571966171));
#22321=CARTESIAN_POINT('Ctrl Pts',(1.13460291804634,-1.,1.76677384551883));
#22322=CARTESIAN_POINT('Ctrl Pts',(1.13460291804634,1.,1.76677384551883));
#22323=CARTESIAN_POINT('Ctrl Pts',(1.14000548337,-1.,1.76997111386806));
#22324=CARTESIAN_POINT('Ctrl Pts',(1.14000548337,1.,1.76997111386806));
#22325=CARTESIAN_POINT('Ctrl Pts',(1.14543858226948,-1.,1.77313777896234));
#22326=CARTESIAN_POINT('Ctrl Pts',(1.14543858226948,1.,1.77313777896234));
#22327=CARTESIAN_POINT('Ctrl Pts',(1.15090197841531,-1.,1.77627422557034));
#22328=CARTESIAN_POINT('Ctrl Pts',(1.15090197841531,1.,1.77627422557034));
#22329=CARTESIAN_POINT('Ctrl Pts',(1.15639547194689,-1.,1.77938085564261));
#22330=CARTESIAN_POINT('Ctrl Pts',(1.15639547194689,1.,1.77938085564261));
#22331=CARTESIAN_POINT('Ctrl Pts',(1.16191881298458,-1.,1.78245795880949));
#22332=CARTESIAN_POINT('Ctrl Pts',(1.16191881298458,1.,1.78245795880949));
#22333=CARTESIAN_POINT('Ctrl Pts',(1.16747166312239,-1.,1.78550566040349));
#22334=CARTESIAN_POINT('Ctrl Pts',(1.16747166312239,1.,1.78550566040349));
#22335=CARTESIAN_POINT('Ctrl Pts',(1.17305363177265,-1.,1.78852398877523));
#22336=CARTESIAN_POINT('Ctrl Pts',(1.17305363177265,1.,1.78852398877523));
#22337=CARTESIAN_POINT('Ctrl Pts',(1.17866429440781,-1.,1.79151291552646));
#22338=CARTESIAN_POINT('Ctrl Pts',(1.17866429440781,1.,1.79151291552646));
#22339=CARTESIAN_POINT('Ctrl Pts',(1.18430321697471,-1.,1.79447240321572));
#22340=CARTESIAN_POINT('Ctrl Pts',(1.18430321697471,1.,1.79447240321572));
#22341=CARTESIAN_POINT('Ctrl Pts',(1.1899699793456,-1.,1.79740245923649));
#22342=CARTESIAN_POINT('Ctrl Pts',(1.1899699793456,1.,1.79740245923649));
#22343=CARTESIAN_POINT('Ctrl Pts',(1.19566418930405,-1.,1.80030314370121));
#22344=CARTESIAN_POINT('Ctrl Pts',(1.19566418930405,1.,1.80030314370121));
#22345=CARTESIAN_POINT('Ctrl Pts',(1.2013854893912,-1.,1.8031745483882));
#22346=CARTESIAN_POINT('Ctrl Pts',(1.2013854893912,1.,1.8031745483882));
#22347=CARTESIAN_POINT('Ctrl Pts',(1.20713356605519,-1.,1.80601678480772));
#22348=CARTESIAN_POINT('Ctrl Pts',(1.20713356605519,1.,1.80601678480772));
#22349=CARTESIAN_POINT('Ctrl Pts',(1.2129081570818,-1.,1.80882996916931));
#22350=CARTESIAN_POINT('Ctrl Pts',(1.2129081570818,1.,1.80882996916931));
#22351=CARTESIAN_POINT('Ctrl Pts',(1.2187090610323,-1.,1.81161420806172));
#22352=CARTESIAN_POINT('Ctrl Pts',(1.2187090610323,1.,1.81161420806172));
#22353=CARTESIAN_POINT('Ctrl Pts',(1.22453613304507,-1.,1.81436959209778));
#22354=CARTESIAN_POINT('Ctrl Pts',(1.22453613304507,1.,1.81436959209778));
#22355=CARTESIAN_POINT('Ctrl Pts',(1.22921864890975,-1.,1.81655087183054));
#22356=CARTESIAN_POINT('Ctrl Pts',(1.22921864890975,1.,1.81655087183054));
#22357=CARTESIAN_POINT('Ctrl Pts',(1.23274224526804,-1.,1.81817389920914));
#22358=CARTESIAN_POINT('Ctrl Pts',(1.23274224526804,1.,1.81817389920914));
#22359=CARTESIAN_POINT('Ctrl Pts',(1.23509651170384,-1.,1.81925017193531));
#22360=CARTESIAN_POINT('Ctrl Pts',(1.23509651170384,1.,1.81925017193531));
#22361=CARTESIAN_POINT('Ctrl Pts',(1.23627494547115,-1.,1.81978687191668));
#22362=CARTESIAN_POINT('Ctrl Pts',(1.23627494547115,1.,1.81978687191668));
#22363=CARTESIAN_POINT('',(0.892032620296855,1.,1.5055822144029));
#22364=CARTESIAN_POINT('Ctrl Pts',(0.892032620296855,1.,1.5055822144029));
#22365=CARTESIAN_POINT('Ctrl Pts',(0.894452006967538,1.,1.50980486807181));
#22366=CARTESIAN_POINT('Ctrl Pts',(0.89918504749193,1.,1.51805569591479));
#22367=CARTESIAN_POINT('Ctrl Pts',(0.905967409640498,1.,1.52984849890434));
#22368=CARTESIAN_POINT('Ctrl Pts',(0.914375919046579,1.,1.54440491152808));
#22369=CARTESIAN_POINT('Ctrl Pts',(0.923832188966322,1.,1.56065988582509));
#22370=CARTESIAN_POINT('Ctrl Pts',(0.932246680128848,1.,1.57499388385561));
#22371=CARTESIAN_POINT('Ctrl Pts',(0.939646377909319,1.,1.58744937489796));
#22372=CARTESIAN_POINT('Ctrl Pts',(0.946078063325795,1.,1.59810042045408));
#22373=CARTESIAN_POINT('Ctrl Pts',(0.951613284361247,1.,1.60706069897794));
#22374=CARTESIAN_POINT('Ctrl Pts',(0.956354422921572,1.,1.61449324337233));
#22375=CARTESIAN_POINT('Ctrl Pts',(0.960438326099958,1.,1.62061638139929));
#22376=CARTESIAN_POINT('Ctrl Pts',(0.964046107037821,1.,1.6257193066974));
#22377=CARTESIAN_POINT('Ctrl Pts',(0.967387853228041,1.,1.63013849959083));
#22378=CARTESIAN_POINT('Ctrl Pts',(0.970669715996356,1.,1.63420665729609));
#22379=CARTESIAN_POINT('Ctrl Pts',(0.974066058287501,1.,1.63820952658157));
#22380=CARTESIAN_POINT('Ctrl Pts',(0.977689794120296,1.,1.64233990826831));
#22381=CARTESIAN_POINT('Ctrl Pts',(0.981562530940574,1.,1.64665139190834));
#22382=CARTESIAN_POINT('Ctrl Pts',(0.985642622921626,1.,1.6511001661277));
#22383=CARTESIAN_POINT('Ctrl Pts',(0.98985562785445,1.,1.65559044289746));
#22384=CARTESIAN_POINT('Ctrl Pts',(0.994121836661115,1.,1.66001553809916));
#22385=CARTESIAN_POINT('Ctrl Pts',(0.998389654952317,1.,1.66430758030304));
#22386=CARTESIAN_POINT('Ctrl Pts',(1.00265091003682,1.,1.66846059277231));
#22387=CARTESIAN_POINT('Ctrl Pts',(1.00692206696387,1.,1.67250335383248));
#22388=CARTESIAN_POINT('Ctrl Pts',(1.01123236493507,1.,1.67648246776457));
#22389=CARTESIAN_POINT('Ctrl Pts',(1.01561026162786,1.,1.6804428989482));
#22390=CARTESIAN_POINT('Ctrl Pts',(1.02006795074222,1.,1.68440578021739));
#22391=CARTESIAN_POINT('Ctrl Pts',(1.02460180535272,1.,1.68836910178475));
#22392=CARTESIAN_POINT('Ctrl Pts',(1.02919977579155,1.,1.69231840863471));
#22393=CARTESIAN_POINT('Ctrl Pts',(1.03384646003587,1.,1.69623414782769));
#22394=CARTESIAN_POINT('Ctrl Pts',(1.03852922490782,1.,1.70010052930951));
#22395=CARTESIAN_POINT('Ctrl Pts',(1.04324363334546,1.,1.70391338707969));
#22396=CARTESIAN_POINT('Ctrl Pts',(1.0479908540499,1.,1.70767646263641));
#22397=CARTESIAN_POINT('Ctrl Pts',(1.05277517202853,1.,1.71139783543986));
#22398=CARTESIAN_POINT('Ctrl Pts',(1.05760163192481,1.,1.71508654427022));
#22399=CARTESIAN_POINT('Ctrl Pts',(1.06247324680649,1.,1.71874858456908));
#22400=CARTESIAN_POINT('Ctrl Pts',(1.06738966975463,1.,1.72238500928456));
#22401=CARTESIAN_POINT('Ctrl Pts',(1.07234866990252,1.,1.72599406198489));
#22402=CARTESIAN_POINT('Ctrl Pts',(1.0773470373727,1.,1.72957248977424));
#22403=CARTESIAN_POINT('Ctrl Pts',(1.08238162784749,1.,1.73311705663407));
#22404=CARTESIAN_POINT('Ctrl Pts',(1.08745056285429,1.,1.73662628326093));
#22405=CARTESIAN_POINT('Ctrl Pts',(1.09255329056496,1.,1.74010053962252));
#22406=CARTESIAN_POINT('Ctrl Pts',(1.09768999241229,1.,1.74354119236212));
#22407=CARTESIAN_POINT('Ctrl Pts',(1.10286118991144,1.,1.74695004214924));
#22408=CARTESIAN_POINT('Ctrl Pts',(1.10806728183003,1.,1.75032866075914));
#22409=CARTESIAN_POINT('Ctrl Pts',(1.11330807582542,1.,1.75367772094617));
#22410=CARTESIAN_POINT('Ctrl Pts',(1.11858293216752,1.,1.75699720772089));
#22411=CARTESIAN_POINT('Ctrl Pts',(1.12389096855078,1.,1.76028671825084));
#22412=CARTESIAN_POINT('Ctrl Pts',(1.12923123555076,1.,1.76354571966171));
#22413=CARTESIAN_POINT('Ctrl Pts',(1.13460291804634,1.,1.76677384551883));
#22414=CARTESIAN_POINT('Ctrl Pts',(1.14000548337,1.,1.76997111386806));
#22415=CARTESIAN_POINT('Ctrl Pts',(1.14543858226948,1.,1.77313777896234));
#22416=CARTESIAN_POINT('Ctrl Pts',(1.15090197841531,1.,1.77627422557034));
#22417=CARTESIAN_POINT('Ctrl Pts',(1.15639547194689,1.,1.77938085564261));
#22418=CARTESIAN_POINT('Ctrl Pts',(1.16191881298458,1.,1.78245795880949));
#22419=CARTESIAN_POINT('Ctrl Pts',(1.16747166312239,1.,1.78550566040349));
#22420=CARTESIAN_POINT('Ctrl Pts',(1.17305363177265,1.,1.78852398877523));
#22421=CARTESIAN_POINT('Ctrl Pts',(1.17866429440781,1.,1.79151291552646));
#22422=CARTESIAN_POINT('Ctrl Pts',(1.18430321697471,1.,1.79447240321572));
#22423=CARTESIAN_POINT('Ctrl Pts',(1.1899699793456,1.,1.79740245923649));
#22424=CARTESIAN_POINT('Ctrl Pts',(1.19566418930405,1.,1.80030314370121));
#22425=CARTESIAN_POINT('Ctrl Pts',(1.2013854893912,1.,1.8031745483882));
#22426=CARTESIAN_POINT('Ctrl Pts',(1.20713356605519,1.,1.80601678480772));
#22427=CARTESIAN_POINT('Ctrl Pts',(1.2129081570818,1.,1.80882996916931));
#22428=CARTESIAN_POINT('Ctrl Pts',(1.2187090610323,1.,1.81161420806172));
#22429=CARTESIAN_POINT('Ctrl Pts',(1.22453613304507,1.,1.81436959209778));
#22430=CARTESIAN_POINT('Ctrl Pts',(1.22921864890975,1.,1.81655087183054));
#22431=CARTESIAN_POINT('Ctrl Pts',(1.23274224526804,1.,1.81817389920914));
#22432=CARTESIAN_POINT('Ctrl Pts',(1.23509651170384,1.,1.81925017193531));
#22433=CARTESIAN_POINT('Ctrl Pts',(1.23627494547115,1.,1.81978687191668));
#22434=CARTESIAN_POINT('',(0.892032620296854,0.,1.5055822144029));
#22435=CARTESIAN_POINT('Origin',(0.,0.,0.));
#22436=CARTESIAN_POINT('',(0.693717979106305,1.,1.60662857109684));
#22437=CARTESIAN_POINT('Origin',(0.,1.,0.));
#22438=CARTESIAN_POINT('',(0.693717979106305,0.,1.60662857109684));
#22439=CARTESIAN_POINT('Ctrl Pts',(0.7455743247944,-1.,2.0698113262342));
#22440=CARTESIAN_POINT('Ctrl Pts',(0.7455743247944,1.,2.0698113262342));
#22441=CARTESIAN_POINT('Ctrl Pts',(0.745832791378367,-1.,2.06854248895728));
#22442=CARTESIAN_POINT('Ctrl Pts',(0.745832791378367,1.,2.06854248895728));
#22443=CARTESIAN_POINT('Ctrl Pts',(0.7463458715442,-1.,2.06600523016815));
#22444=CARTESIAN_POINT('Ctrl Pts',(0.7463458715442,1.,2.06600523016815));
#22445=CARTESIAN_POINT('Ctrl Pts',(0.747103932787919,-1.,2.06220058927826));
#22446=CARTESIAN_POINT('Ctrl Pts',(0.747103932787919,1.,2.06220058927826));
#22447=CARTESIAN_POINT('Ctrl Pts',(0.748091554183802,-1.,2.05713023031007));
#22448=CARTESIAN_POINT('Ctrl Pts',(0.748091554183802,1.,2.05713023031007));
#22449=CARTESIAN_POINT('Ctrl Pts',(0.749287468665046,-1.,2.05079645592154));
#22450=CARTESIAN_POINT('Ctrl Pts',(0.749287468665046,1.,2.05079645592154));
#22451=CARTESIAN_POINT('Ctrl Pts',(0.750444657875575,-1.,2.04446689147979));
#22452=CARTESIAN_POINT('Ctrl Pts',(0.750444657875575,1.,2.04446689147979));
#22453=CARTESIAN_POINT('Ctrl Pts',(0.751562963361115,-1.,2.03814160092099));
#22454=CARTESIAN_POINT('Ctrl Pts',(0.751562963361115,1.,2.03814160092099));
#22455=CARTESIAN_POINT('Ctrl Pts',(0.75264218048721,-1.,2.03182068456221));
#22456=CARTESIAN_POINT('Ctrl Pts',(0.75264218048721,1.,2.03182068456221));
#22457=CARTESIAN_POINT('Ctrl Pts',(0.753682061112768,-1.,2.02550428623313));
#22458=CARTESIAN_POINT('Ctrl Pts',(0.753682061112768,1.,2.02550428623313));
#22459=CARTESIAN_POINT('Ctrl Pts',(0.754682330722816,-1.,2.01919259405809));
#22460=CARTESIAN_POINT('Ctrl Pts',(0.754682330722816,1.,2.01919259405809));
#22461=CARTESIAN_POINT('Ctrl Pts',(0.755642704957865,-1.,2.01288584328084));
#22462=CARTESIAN_POINT('Ctrl Pts',(0.755642704957865,1.,2.01288584328084));
#22463=CARTESIAN_POINT('Ctrl Pts',(0.75656290464667,-1.,2.0065843158773));
#22464=CARTESIAN_POINT('Ctrl Pts',(0.75656290464667,1.,2.0065843158773));
#22465=CARTESIAN_POINT('Ctrl Pts',(0.757442676862724,-1.,2.00028834739178));
#22466=CARTESIAN_POINT('Ctrl Pts',(0.757442676862724,1.,2.00028834739178));
#22467=CARTESIAN_POINT('Ctrl Pts',(0.758281796766761,-1.,1.99399831098817));
#22468=CARTESIAN_POINT('Ctrl Pts',(0.758281796766761,1.,1.99399831098817));
#22469=CARTESIAN_POINT('Ctrl Pts',(0.759080037802488,-1.,1.98771456680874));
#22470=CARTESIAN_POINT('Ctrl Pts',(0.759080037802488,1.,1.98771456680874));
#22471=CARTESIAN_POINT('Ctrl Pts',(0.75983714745219,-1.,1.98143741418172));
#22472=CARTESIAN_POINT('Ctrl Pts',(0.75983714745219,1.,1.98143741418172));
#22473=CARTESIAN_POINT('Ctrl Pts',(0.760552825409757,-1.,1.97516705321494));
#22474=CARTESIAN_POINT('Ctrl Pts',(0.760552825409757,1.,1.97516705321494));
#22475=CARTESIAN_POINT('Ctrl Pts',(0.76122669048382,-1.,1.96890351582499));
#22476=CARTESIAN_POINT('Ctrl Pts',(0.76122669048382,1.,1.96890351582499));
#22477=CARTESIAN_POINT('Ctrl Pts',(0.761858300014423,-1.,1.96264672744186));
#22478=CARTESIAN_POINT('Ctrl Pts',(0.761858300014423,1.,1.96264672744186));
#22479=CARTESIAN_POINT('Ctrl Pts',(0.762447203806178,-1.,1.95639665309869));
#22480=CARTESIAN_POINT('Ctrl Pts',(0.762447203806178,1.,1.95639665309869));
#22481=CARTESIAN_POINT('Ctrl Pts',(0.762992990878769,-1.,1.95015342590024));
#22482=CARTESIAN_POINT('Ctrl Pts',(0.762992990878769,1.,1.95015342590024));
#22483=CARTESIAN_POINT('Ctrl Pts',(0.763495333538629,-1.,1.9439174661764));
#22484=CARTESIAN_POINT('Ctrl Pts',(0.763495333538629,1.,1.9439174661764));
#22485=CARTESIAN_POINT('Ctrl Pts',(0.763954049121458,-1.,1.93768964875886));
#22486=CARTESIAN_POINT('Ctrl Pts',(0.763954049121458,1.,1.93768964875886));
#22487=CARTESIAN_POINT('Ctrl Pts',(0.76436901067394,-1.,1.93147105496382));
#22488=CARTESIAN_POINT('Ctrl Pts',(0.76436901067394,1.,1.93147105496382));
#22489=CARTESIAN_POINT('Ctrl Pts',(0.764740025488211,-1.,1.92526263537048));
#22490=CARTESIAN_POINT('Ctrl Pts',(0.764740025488211,1.,1.92526263537048));
#22491=CARTESIAN_POINT('Ctrl Pts',(0.765066729667088,-1.,1.91906491634196));
#22492=CARTESIAN_POINT('Ctrl Pts',(0.765066729667088,1.,1.91906491634196));
#22493=CARTESIAN_POINT('Ctrl Pts',(0.765348465884722,-1.,1.91287765805169));
#22494=CARTESIAN_POINT('Ctrl Pts',(0.765348465884722,1.,1.91287765805169));
#22495=CARTESIAN_POINT('Ctrl Pts',(0.765584196937919,-1.,1.90669961402356));
#22496=CARTESIAN_POINT('Ctrl Pts',(0.765584196937919,1.,1.90669961402356));
#22497=CARTESIAN_POINT('Ctrl Pts',(0.765772772593386,-1.,1.90052930393596));
#22498=CARTESIAN_POINT('Ctrl Pts',(0.765772772593386,1.,1.90052930393596));
#22499=CARTESIAN_POINT('Ctrl Pts',(0.765913193856978,-1.,1.89436577771388));
#22500=CARTESIAN_POINT('Ctrl Pts',(0.765913193856978,1.,1.89436577771388));
#22501=CARTESIAN_POINT('Ctrl Pts',(0.766004837062091,-1.,1.88820926433409));
#22502=CARTESIAN_POINT('Ctrl Pts',(0.766004837062091,1.,1.88820926433409));
#22503=CARTESIAN_POINT('Ctrl Pts',(0.766047794851864,-1.,1.88206215302561));
#22504=CARTESIAN_POINT('Ctrl Pts',(0.766047794851864,1.,1.88206215302561));
#22505=CARTESIAN_POINT('Ctrl Pts',(0.766042837036744,-1.,1.87592888967883));
#22506=CARTESIAN_POINT('Ctrl Pts',(0.766042837036744,1.,1.87592888967883));
#22507=CARTESIAN_POINT('Ctrl Pts',(0.765990708546091,-1.,1.86981398314341));
#22508=CARTESIAN_POINT('Ctrl Pts',(0.765990708546091,1.,1.86981398314341));
#22509=CARTESIAN_POINT('Ctrl Pts',(0.765891519092547,-1.,1.86372027063312));
#22510=CARTESIAN_POINT('Ctrl Pts',(0.765891519092547,1.,1.86372027063312));
#22511=CARTESIAN_POINT('Ctrl Pts',(0.765744212909318,-1.,1.85764741390394));
#22512=CARTESIAN_POINT('Ctrl Pts',(0.765744212909318,1.,1.85764741390394));
#22513=CARTESIAN_POINT('Ctrl Pts',(0.765545710619062,-1.,1.85158945130063));
#22514=CARTESIAN_POINT('Ctrl Pts',(0.765545710619062,1.,1.85158945130063));
#22515=CARTESIAN_POINT('Ctrl Pts',(0.765291664862029,-1.,1.84553698875924));
#22516=CARTESIAN_POINT('Ctrl Pts',(0.765291664862029,1.,1.84553698875924));
#22517=CARTESIAN_POINT('Ctrl Pts',(0.764978057881737,-1.,1.83948181064835));
#22518=CARTESIAN_POINT('Ctrl Pts',(0.764978057881737,1.,1.83948181064835));
#22519=CARTESIAN_POINT('Ctrl Pts',(0.764602549687853,-1.,1.83342077227142));
#22520=CARTESIAN_POINT('Ctrl Pts',(0.764602549687853,1.,1.83342077227142));
#22521=CARTESIAN_POINT('Ctrl Pts',(0.764165902605995,-1.,1.82735991200065));
#22522=CARTESIAN_POINT('Ctrl Pts',(0.764165902605995,1.,1.82735991200065));
#22523=CARTESIAN_POINT('Ctrl Pts',(0.763673465462726,-1.,1.82131873145266));
#22524=CARTESIAN_POINT('Ctrl Pts',(0.763673465462726,1.,1.82131873145266));
#22525=CARTESIAN_POINT('Ctrl Pts',(0.763132003836634,-1.,1.8153211840553));
#22526=CARTESIAN_POINT('Ctrl Pts',(0.763132003836634,1.,1.8153211840553));
#22527=CARTESIAN_POINT('Ctrl Pts',(0.762546129463938,-1.,1.80938551463965));
#22528=CARTESIAN_POINT('Ctrl Pts',(0.762546129463938,1.,1.80938551463965));
#22529=CARTESIAN_POINT('Ctrl Pts',(0.761915336443547,-1.,1.80351583877342));
#22530=CARTESIAN_POINT('Ctrl Pts',(0.761915336443547,1.,1.80351583877342));
#22531=CARTESIAN_POINT('Ctrl Pts',(0.761229695230558,-1.,1.79768986997783));
#22532=CARTESIAN_POINT('Ctrl Pts',(0.761229695230558,1.,1.79768986997783));
#22533=CARTESIAN_POINT('Ctrl Pts',(0.760469555880749,-1.,1.7918581561088));
#22534=CARTESIAN_POINT('Ctrl Pts',(0.760469555880749,1.,1.7918581561088));
#22535=CARTESIAN_POINT('Ctrl Pts',(0.759614401110189,-1.,1.78596964884604));
#22536=CARTESIAN_POINT('Ctrl Pts',(0.759614401110189,1.,1.78596964884604));
#22537=CARTESIAN_POINT('Ctrl Pts',(0.758650626677518,-1.,1.77999411220945));
#22538=CARTESIAN_POINT('Ctrl Pts',(0.758650626677518,1.,1.77999411220945));
#22539=CARTESIAN_POINT('Ctrl Pts',(0.757578264077028,-1.,1.77394167108292));
#22540=CARTESIAN_POINT('Ctrl Pts',(0.757578264077028,1.,1.77394167108292));
#22541=CARTESIAN_POINT('Ctrl Pts',(0.75642189602781,-1.,1.76789396002998));
#22542=CARTESIAN_POINT('Ctrl Pts',(0.75642189602781,1.,1.76789396002998));
#22543=CARTESIAN_POINT('Ctrl Pts',(0.755220979974461,-1.,1.76197817240128));
#22544=CARTESIAN_POINT('Ctrl Pts',(0.755220979974461,1.,1.76197817240128));
#22545=CARTESIAN_POINT('Ctrl Pts',(0.754009254027828,-1.,1.75631083600019));
#22546=CARTESIAN_POINT('Ctrl Pts',(0.754009254027828,1.,1.75631083600019));
#22547=CARTESIAN_POINT('Ctrl Pts',(0.752797683531314,-1.,1.75095139468794));
#22548=CARTESIAN_POINT('Ctrl Pts',(0.752797683531314,1.,1.75095139468794));
#22549=CARTESIAN_POINT('Ctrl Pts',(0.751555614164482,-1.,1.74585086852502));
#22550=CARTESIAN_POINT('Ctrl Pts',(0.751555614164482,1.,1.74585086852502));
#22551=CARTESIAN_POINT('Ctrl Pts',(0.750193435981249,-1.,1.74080458267114));
#22552=CARTESIAN_POINT('Ctrl Pts',(0.750193435981249,1.,1.74080458267114));
#22553=CARTESIAN_POINT('Ctrl Pts',(0.74858246295687,-1.,1.7355035168033));
#22554=CARTESIAN_POINT('Ctrl Pts',(0.74858246295687,1.,1.7355035168033));
#22555=CARTESIAN_POINT('Ctrl Pts',(0.746574710097752,-1.,1.72958533647714));
#22556=CARTESIAN_POINT('Ctrl Pts',(0.746574710097752,1.,1.72958533647714));
#22557=CARTESIAN_POINT('Ctrl Pts',(0.744021445433093,-1.,1.72268229916769));
#22558=CARTESIAN_POINT('Ctrl Pts',(0.744021445433093,1.,1.72268229916769));
#22559=CARTESIAN_POINT('Ctrl Pts',(0.74079516202821,-1.,1.71447789751001));
#22560=CARTESIAN_POINT('Ctrl Pts',(0.74079516202821,1.,1.71447789751001));
#22561=CARTESIAN_POINT('Ctrl Pts',(0.736799665716932,-1.,1.70473309004249));
#22562=CARTESIAN_POINT('Ctrl Pts',(0.736799665716932,1.,1.70473309004249));
#22563=CARTESIAN_POINT('Ctrl Pts',(0.731963238685357,-1.,1.69326921972915));
#22564=CARTESIAN_POINT('Ctrl Pts',(0.731963238685357,1.,1.69326921972915));
#22565=CARTESIAN_POINT('Ctrl Pts',(0.726235967982445,-1.,1.67996158451922));
#22566=CARTESIAN_POINT('Ctrl Pts',(0.726235967982445,1.,1.67996158451922));
#22567=CARTESIAN_POINT('Ctrl Pts',(0.719585433787949,-1.,1.66472880551777));
#22568=CARTESIAN_POINT('Ctrl Pts',(0.719585433787949,1.,1.66472880551777));
#22569=CARTESIAN_POINT('Ctrl Pts',(0.711993139340447,-1.,1.64752408828442));
#22570=CARTESIAN_POINT('Ctrl Pts',(0.711993139340447,1.,1.64752408828442));
#22571=CARTESIAN_POINT('Ctrl Pts',(0.705159151977294,-1.,1.6321654166204));
#22572=CARTESIAN_POINT('Ctrl Pts',(0.705159151977294,1.,1.6321654166204));
#22573=CARTESIAN_POINT('Ctrl Pts',(0.699605146398836,-1.,1.61974673471117));
#22574=CARTESIAN_POINT('Ctrl Pts',(0.699605146398836,1.,1.61974673471117));
#22575=CARTESIAN_POINT('Ctrl Pts',(0.69571209787897,-1.,1.61106790957619));
#22576=CARTESIAN_POINT('Ctrl Pts',(0.69571209787897,1.,1.61106790957619));
#22577=CARTESIAN_POINT('Ctrl Pts',(0.693717979106305,-1.,1.60662857109684));
#22578=CARTESIAN_POINT('Ctrl Pts',(0.693717979106305,1.,1.60662857109684));
#22579=CARTESIAN_POINT('',(0.7455743247944,1.,2.0698113262342));
#22580=CARTESIAN_POINT('Ctrl Pts',(0.7455743247944,1.,2.0698113262342));
#22581=CARTESIAN_POINT('Ctrl Pts',(0.745832791378367,1.,2.06854248895728));
#22582=CARTESIAN_POINT('Ctrl Pts',(0.7463458715442,1.,2.06600523016815));
#22583=CARTESIAN_POINT('Ctrl Pts',(0.747103932787919,1.,2.06220058927826));
#22584=CARTESIAN_POINT('Ctrl Pts',(0.748091554183802,1.,2.05713023031007));
#22585=CARTESIAN_POINT('Ctrl Pts',(0.749287468665046,1.,2.05079645592154));
#22586=CARTESIAN_POINT('Ctrl Pts',(0.750444657875575,1.,2.04446689147979));
#22587=CARTESIAN_POINT('Ctrl Pts',(0.751562963361115,1.,2.03814160092099));
#22588=CARTESIAN_POINT('Ctrl Pts',(0.75264218048721,1.,2.03182068456221));
#22589=CARTESIAN_POINT('Ctrl Pts',(0.753682061112768,1.,2.02550428623313));
#22590=CARTESIAN_POINT('Ctrl Pts',(0.754682330722816,1.,2.01919259405809));
#22591=CARTESIAN_POINT('Ctrl Pts',(0.755642704957865,1.,2.01288584328084));
#22592=CARTESIAN_POINT('Ctrl Pts',(0.75656290464667,1.,2.0065843158773));
#22593=CARTESIAN_POINT('Ctrl Pts',(0.757442676862724,1.,2.00028834739178));
#22594=CARTESIAN_POINT('Ctrl Pts',(0.758281796766761,1.,1.99399831098817));
#22595=CARTESIAN_POINT('Ctrl Pts',(0.759080037802488,1.,1.98771456680874));
#22596=CARTESIAN_POINT('Ctrl Pts',(0.75983714745219,1.,1.98143741418172));
#22597=CARTESIAN_POINT('Ctrl Pts',(0.760552825409757,1.,1.97516705321494));
#22598=CARTESIAN_POINT('Ctrl Pts',(0.76122669048382,1.,1.96890351582499));
#22599=CARTESIAN_POINT('Ctrl Pts',(0.761858300014423,1.,1.96264672744186));
#22600=CARTESIAN_POINT('Ctrl Pts',(0.762447203806178,1.,1.95639665309869));
#22601=CARTESIAN_POINT('Ctrl Pts',(0.762992990878769,1.,1.95015342590024));
#22602=CARTESIAN_POINT('Ctrl Pts',(0.763495333538629,1.,1.9439174661764));
#22603=CARTESIAN_POINT('Ctrl Pts',(0.763954049121458,1.,1.93768964875886));
#22604=CARTESIAN_POINT('Ctrl Pts',(0.76436901067394,1.,1.93147105496382));
#22605=CARTESIAN_POINT('Ctrl Pts',(0.764740025488211,1.,1.92526263537048));
#22606=CARTESIAN_POINT('Ctrl Pts',(0.765066729667088,1.,1.91906491634196));
#22607=CARTESIAN_POINT('Ctrl Pts',(0.765348465884722,1.,1.91287765805169));
#22608=CARTESIAN_POINT('Ctrl Pts',(0.765584196937919,1.,1.90669961402356));
#22609=CARTESIAN_POINT('Ctrl Pts',(0.765772772593386,1.,1.90052930393596));
#22610=CARTESIAN_POINT('Ctrl Pts',(0.765913193856978,1.,1.89436577771388));
#22611=CARTESIAN_POINT('Ctrl Pts',(0.766004837062091,1.,1.88820926433409));
#22612=CARTESIAN_POINT('Ctrl Pts',(0.766047794851864,1.,1.88206215302561));
#22613=CARTESIAN_POINT('Ctrl Pts',(0.766042837036744,1.,1.87592888967883));
#22614=CARTESIAN_POINT('Ctrl Pts',(0.765990708546091,1.,1.86981398314341));
#22615=CARTESIAN_POINT('Ctrl Pts',(0.765891519092547,1.,1.86372027063312));
#22616=CARTESIAN_POINT('Ctrl Pts',(0.765744212909318,1.,1.85764741390394));
#22617=CARTESIAN_POINT('Ctrl Pts',(0.765545710619062,1.,1.85158945130063));
#22618=CARTESIAN_POINT('Ctrl Pts',(0.765291664862029,1.,1.84553698875924));
#22619=CARTESIAN_POINT('Ctrl Pts',(0.764978057881737,1.,1.83948181064835));
#22620=CARTESIAN_POINT('Ctrl Pts',(0.764602549687853,1.,1.83342077227142));
#22621=CARTESIAN_POINT('Ctrl Pts',(0.764165902605995,1.,1.82735991200065));
#22622=CARTESIAN_POINT('Ctrl Pts',(0.763673465462726,1.,1.82131873145266));
#22623=CARTESIAN_POINT('Ctrl Pts',(0.763132003836634,1.,1.8153211840553));
#22624=CARTESIAN_POINT('Ctrl Pts',(0.762546129463938,1.,1.80938551463965));
#22625=CARTESIAN_POINT('Ctrl Pts',(0.761915336443547,1.,1.80351583877342));
#22626=CARTESIAN_POINT('Ctrl Pts',(0.761229695230558,1.,1.79768986997783));
#22627=CARTESIAN_POINT('Ctrl Pts',(0.760469555880749,1.,1.7918581561088));
#22628=CARTESIAN_POINT('Ctrl Pts',(0.759614401110189,1.,1.78596964884604));
#22629=CARTESIAN_POINT('Ctrl Pts',(0.758650626677518,1.,1.77999411220945));
#22630=CARTESIAN_POINT('Ctrl Pts',(0.757578264077028,1.,1.77394167108292));
#22631=CARTESIAN_POINT('Ctrl Pts',(0.75642189602781,1.,1.76789396002998));
#22632=CARTESIAN_POINT('Ctrl Pts',(0.755220979974461,1.,1.76197817240128));
#22633=CARTESIAN_POINT('Ctrl Pts',(0.754009254027828,1.,1.75631083600019));
#22634=CARTESIAN_POINT('Ctrl Pts',(0.752797683531314,1.,1.75095139468794));
#22635=CARTESIAN_POINT('Ctrl Pts',(0.751555614164482,1.,1.74585086852502));
#22636=CARTESIAN_POINT('Ctrl Pts',(0.750193435981249,1.,1.74080458267114));
#22637=CARTESIAN_POINT('Ctrl Pts',(0.74858246295687,1.,1.7355035168033));
#22638=CARTESIAN_POINT('Ctrl Pts',(0.746574710097752,1.,1.72958533647714));
#22639=CARTESIAN_POINT('Ctrl Pts',(0.744021445433093,1.,1.72268229916769));
#22640=CARTESIAN_POINT('Ctrl Pts',(0.74079516202821,1.,1.71447789751001));
#22641=CARTESIAN_POINT('Ctrl Pts',(0.736799665716932,1.,1.70473309004249));
#22642=CARTESIAN_POINT('Ctrl Pts',(0.731963238685357,1.,1.69326921972915));
#22643=CARTESIAN_POINT('Ctrl Pts',(0.726235967982445,1.,1.67996158451922));
#22644=CARTESIAN_POINT('Ctrl Pts',(0.719585433787949,1.,1.66472880551777));
#22645=CARTESIAN_POINT('Ctrl Pts',(0.711993139340447,1.,1.64752408828442));
#22646=CARTESIAN_POINT('Ctrl Pts',(0.705159151977294,1.,1.6321654166204));
#22647=CARTESIAN_POINT('Ctrl Pts',(0.699605146398836,1.,1.61974673471117));
#22648=CARTESIAN_POINT('Ctrl Pts',(0.69571209787897,1.,1.61106790957619));
#22649=CARTESIAN_POINT('Ctrl Pts',(0.693717979106305,1.,1.60662857109684));
#22650=CARTESIAN_POINT('',(0.7455743247944,0.,2.0698113262342));
#22651=CARTESIAN_POINT('Origin',(0.61342227326009,0.,2.11275013067528));
#22652=CARTESIAN_POINT('',(0.61342227326009,1.,2.11275013067528));
#22653=CARTESIAN_POINT('',(0.7455743247944,1.,2.0698113262342));
#22654=CARTESIAN_POINT('',(0.61342227326009,0.,2.11275013067528));
#22655=CARTESIAN_POINT('Ctrl Pts',(0.383122945602004,-1.,1.7075470150345));
#22656=CARTESIAN_POINT('Ctrl Pts',(0.383122945602004,1.,1.7075470150345));
#22657=CARTESIAN_POINT('Ctrl Pts',(0.384119047315541,-1.,1.71231062891958));
#22658=CARTESIAN_POINT('Ctrl Pts',(0.384119047315541,1.,1.71231062891958));
#22659=CARTESIAN_POINT('Ctrl Pts',(0.38607079032701,-1.,1.72162022246158));
#22660=CARTESIAN_POINT('Ctrl Pts',(0.38607079032701,1.,1.72162022246158));
#22661=CARTESIAN_POINT('Ctrl Pts',(0.388877023509191,-1.,1.7349317097561));
#22662=CARTESIAN_POINT('Ctrl Pts',(0.388877023509191,1.,1.7349317097561));
#22663=CARTESIAN_POINT('Ctrl Pts',(0.392375812294307,-1.,1.75137405313962));
#22664=CARTESIAN_POINT('Ctrl Pts',(0.392375812294307,1.,1.75137405313962));
#22665=CARTESIAN_POINT('Ctrl Pts',(0.39634619612042,-1.,1.7697556004756));
#22666=CARTESIAN_POINT('Ctrl Pts',(0.39634619612042,1.,1.7697556004756));
#22667=CARTESIAN_POINT('Ctrl Pts',(0.39991940378308,-1.,1.78598826347533));
#22668=CARTESIAN_POINT('Ctrl Pts',(0.39991940378308,1.,1.78598826347533));
#22669=CARTESIAN_POINT('Ctrl Pts',(0.403107976170441,-1.,1.80012077176221));
#22670=CARTESIAN_POINT('Ctrl Pts',(0.403107976170441,1.,1.80012077176221));
#22671=CARTESIAN_POINT('Ctrl Pts',(0.405933518411838,-1.,1.81223801813988));
#22672=CARTESIAN_POINT('Ctrl Pts',(0.405933518411838,1.,1.81223801813988));
#22673=CARTESIAN_POINT('Ctrl Pts',(0.408428948108533,-1.,1.8224702267854));
#22674=CARTESIAN_POINT('Ctrl Pts',(0.408428948108533,1.,1.8224702267854));
#22675=CARTESIAN_POINT('Ctrl Pts',(0.410641256301674,-1.,1.83100408895216));
#22676=CARTESIAN_POINT('Ctrl Pts',(0.410641256301674,1.,1.83100408895216));
#22677=CARTESIAN_POINT('Ctrl Pts',(0.412633125322161,-1.,1.83808953475839));
#22678=CARTESIAN_POINT('Ctrl Pts',(0.412633125322161,1.,1.83808953475839));
#22679=CARTESIAN_POINT('Ctrl Pts',(0.41448743825434,-1.,1.8440575707371));
#22680=CARTESIAN_POINT('Ctrl Pts',(0.41448743825434,1.,1.8440575707371));
#22681=CARTESIAN_POINT('Ctrl Pts',(0.416300022038864,-1.,1.84929312929882));
#22682=CARTESIAN_POINT('Ctrl Pts',(0.416300022038864,1.,1.84929312929882));
#22683=CARTESIAN_POINT('Ctrl Pts',(0.418164129143534,-1.,1.85417632856234));
#22684=CARTESIAN_POINT('Ctrl Pts',(0.418164129143534,1.,1.85417632856234));
#22685=CARTESIAN_POINT('Ctrl Pts',(0.420157287975619,-1.,1.85903281096686));
#22686=CARTESIAN_POINT('Ctrl Pts',(0.420157287975619,1.,1.85903281096686));
#22687=CARTESIAN_POINT('Ctrl Pts',(0.422327307418275,-1.,1.86408083334028));
#22688=CARTESIAN_POINT('Ctrl Pts',(0.422327307418275,1.,1.86408083334028));
#22689=CARTESIAN_POINT('Ctrl Pts',(0.424678177291358,-1.,1.86937803944323));
#22690=CARTESIAN_POINT('Ctrl Pts',(0.424678177291358,1.,1.86937803944323));
#22691=CARTESIAN_POINT('Ctrl Pts',(0.427183828519102,-1.,1.87486989291484));
#22692=CARTESIAN_POINT('Ctrl Pts',(0.427183828519102,1.,1.87486989291484));
#22693=CARTESIAN_POINT('Ctrl Pts',(0.429803062482344,-1.,1.88044229001832));
#22694=CARTESIAN_POINT('Ctrl Pts',(0.429803062482344,1.,1.88044229001832));
#22695=CARTESIAN_POINT('Ctrl Pts',(0.432493038548748,-1.,1.88596913666793));
#22696=CARTESIAN_POINT('Ctrl Pts',(0.432493038548748,1.,1.88596913666793));
#22697=CARTESIAN_POINT('Ctrl Pts',(0.435225660963383,-1.,1.89136993975504));
#22698=CARTESIAN_POINT('Ctrl Pts',(0.435225660963383,1.,1.89136993975504));
#22699=CARTESIAN_POINT('Ctrl Pts',(0.437995003948244,-1.,1.89663648956466));
#22700=CARTESIAN_POINT('Ctrl Pts',(0.437995003948244,1.,1.89663648956466));
#22701=CARTESIAN_POINT('Ctrl Pts',(0.440807833704038,-1.,1.90180124389086));
#22702=CARTESIAN_POINT('Ctrl Pts',(0.440807833704038,1.,1.90180124389086));
#22703=CARTESIAN_POINT('Ctrl Pts',(0.44367755684915,-1.,1.90691756144898));
#22704=CARTESIAN_POINT('Ctrl Pts',(0.44367755684915,1.,1.90691756144898));
#22705=CARTESIAN_POINT('Ctrl Pts',(0.446617343485711,-1.,1.9120369998112));
#22706=CARTESIAN_POINT('Ctrl Pts',(0.446617343485711,1.,1.9120369998112));
#22707=CARTESIAN_POINT('Ctrl Pts',(0.449632260106662,-1.,1.91718342555755));
#22708=CARTESIAN_POINT('Ctrl Pts',(0.449632260106662,1.,1.91718342555755));
#22709=CARTESIAN_POINT('Ctrl Pts',(0.452719478359432,-1.,1.92235380648502));
#22710=CARTESIAN_POINT('Ctrl Pts',(0.452719478359432,1.,1.92235380648502));
#22711=CARTESIAN_POINT('Ctrl Pts',(0.45587200517437,-1.,1.92753067150476));
#22712=CARTESIAN_POINT('Ctrl Pts',(0.45587200517437,1.,1.92753067150476));
#22713=CARTESIAN_POINT('Ctrl Pts',(0.459081234547926,-1.,1.93269066517934));
#22714=CARTESIAN_POINT('Ctrl Pts',(0.459081234547926,1.,1.93269066517934));
#22715=CARTESIAN_POINT('Ctrl Pts',(0.462340031009056,-1.,1.93781486640821));
#22716=CARTESIAN_POINT('Ctrl Pts',(0.462340031009056,1.,1.93781486640821));
#22717=CARTESIAN_POINT('Ctrl Pts',(0.46564546202603,-1.,1.9428979419619));
#22718=CARTESIAN_POINT('Ctrl Pts',(0.46564546202603,1.,1.9428979419619));
#22719=CARTESIAN_POINT('Ctrl Pts',(0.468997482913135,-1.,1.94794381136514));
#22720=CARTESIAN_POINT('Ctrl Pts',(0.468997482913135,1.,1.94794381136514));
#22721=CARTESIAN_POINT('Ctrl Pts',(0.472397672264072,-1.,1.95296148278133));
#22722=CARTESIAN_POINT('Ctrl Pts',(0.472397672264072,1.,1.95296148278133));
#22723=CARTESIAN_POINT('Ctrl Pts',(0.475848034683176,-1.,1.95796111148177));
#22724=CARTESIAN_POINT('Ctrl Pts',(0.475848034683176,1.,1.95796111148177));
#22725=CARTESIAN_POINT('Ctrl Pts',(0.479349583074855,-1.,1.96294933055943));
#22726=CARTESIAN_POINT('Ctrl Pts',(0.479349583074855,1.,1.96294933055943));
#22727=CARTESIAN_POINT('Ctrl Pts',(0.48290166212069,-1.,1.96792703422362));
#22728=CARTESIAN_POINT('Ctrl Pts',(0.48290166212069,1.,1.96792703422362));
#22729=CARTESIAN_POINT('Ctrl Pts',(0.486502692907658,-1.,1.97289186263272));
#22730=CARTESIAN_POINT('Ctrl Pts',(0.486502692907658,1.,1.97289186263272));
#22731=CARTESIAN_POINT('Ctrl Pts',(0.490150627860952,-1.,1.97783973019229));
#22732=CARTESIAN_POINT('Ctrl Pts',(0.490150627860952,1.,1.97783973019229));
#22733=CARTESIAN_POINT('Ctrl Pts',(0.493843476541494,-1.,1.98276658761821));
#22734=CARTESIAN_POINT('Ctrl Pts',(0.493843476541494,1.,1.98276658761821));
#22735=CARTESIAN_POINT('Ctrl Pts',(0.497579909545574,-1.,1.98767044752932));
#22736=CARTESIAN_POINT('Ctrl Pts',(0.497579909545574,1.,1.98767044752932));
#22737=CARTESIAN_POINT('Ctrl Pts',(0.501359287727146,-1.,1.99255149126155));
#22738=CARTESIAN_POINT('Ctrl Pts',(0.501359287727146,1.,1.99255149126155));
#22739=CARTESIAN_POINT('Ctrl Pts',(0.505181361323026,-1.,1.99741107463572));
#22740=CARTESIAN_POINT('Ctrl Pts',(0.505181361323026,1.,1.99741107463572));
#22741=CARTESIAN_POINT('Ctrl Pts',(0.509046069886157,-1.,2.00225107134734));
#22742=CARTESIAN_POINT('Ctrl Pts',(0.509046069886157,1.,2.00225107134734));
#22743=CARTESIAN_POINT('Ctrl Pts',(0.512953306961792,-1.,2.00707309946949));
#22744=CARTESIAN_POINT('Ctrl Pts',(0.512953306961792,1.,2.00707309946949));
#22745=CARTESIAN_POINT('Ctrl Pts',(0.516902681728687,-1.,2.01187773939242));
#22746=CARTESIAN_POINT('Ctrl Pts',(0.516902681728687,1.,2.01187773939242));
#22747=CARTESIAN_POINT('Ctrl Pts',(0.52089359039937,-1.,2.01666477917286));
#22748=CARTESIAN_POINT('Ctrl Pts',(0.52089359039937,1.,2.01666477917286));
#22749=CARTESIAN_POINT('Ctrl Pts',(0.524925318333476,-1.,2.02143356304698));
#22750=CARTESIAN_POINT('Ctrl Pts',(0.524925318333476,1.,2.02143356304698));
#22751=CARTESIAN_POINT('Ctrl Pts',(0.528997127241914,-1.,2.0261832908329));
#22752=CARTESIAN_POINT('Ctrl Pts',(0.528997127241914,1.,2.0261832908329));
#22753=CARTESIAN_POINT('Ctrl Pts',(0.533108355132976,-1.,2.03091336214426));
#22754=CARTESIAN_POINT('Ctrl Pts',(0.533108355132976,1.,2.03091336214426));
#22755=CARTESIAN_POINT('Ctrl Pts',(0.537258489833262,-1.,2.03562362954037));
#22756=CARTESIAN_POINT('Ctrl Pts',(0.537258489833262,1.,2.03562362954037));
#22757=CARTESIAN_POINT('Ctrl Pts',(0.541447120615659,-1.,2.04031422690527));
#22758=CARTESIAN_POINT('Ctrl Pts',(0.541447120615659,1.,2.04031422690527));
#22759=CARTESIAN_POINT('Ctrl Pts',(0.54567390381743,-1.,2.04498544714588));
#22760=CARTESIAN_POINT('Ctrl Pts',(0.54567390381743,1.,2.04498544714588));
#22761=CARTESIAN_POINT('Ctrl Pts',(0.549938525150295,-1.,2.04963761077958));
#22762=CARTESIAN_POINT('Ctrl Pts',(0.549938525150295,1.,2.04963761077958));
#22763=CARTESIAN_POINT('Ctrl Pts',(0.554240657463906,-1.,2.05427091604413));
#22764=CARTESIAN_POINT('Ctrl Pts',(0.554240657463906,1.,2.05427091604413));
#22765=CARTESIAN_POINT('Ctrl Pts',(0.558579940185151,-1.,2.05888537756462));
#22766=CARTESIAN_POINT('Ctrl Pts',(0.558579940185151,1.,2.05888537756462));
#22767=CARTESIAN_POINT('Ctrl Pts',(0.562955993082261,-1.,2.06348090160589));
#22768=CARTESIAN_POINT('Ctrl Pts',(0.562955993082261,1.,2.06348090160589));
#22769=CARTESIAN_POINT('Ctrl Pts',(0.567368421181087,-1.,2.06805732997334));
#22770=CARTESIAN_POINT('Ctrl Pts',(0.567368421181087,1.,2.06805732997334));
#22771=CARTESIAN_POINT('Ctrl Pts',(0.571816823242602,-1.,2.07261449292824));
#22772=CARTESIAN_POINT('Ctrl Pts',(0.571816823242602,1.,2.07261449292824));
#22773=CARTESIAN_POINT('Ctrl Pts',(0.576300797416844,-1.,2.07715226767559));
#22774=CARTESIAN_POINT('Ctrl Pts',(0.576300797416844,1.,2.07715226767559));
#22775=CARTESIAN_POINT('Ctrl Pts',(0.580819952108063,-1.,2.08167059018418));
#22776=CARTESIAN_POINT('Ctrl Pts',(0.580819952108063,1.,2.08167059018418));
#22777=CARTESIAN_POINT('Ctrl Pts',(0.585373918991617,-1.,2.08616943727951));
#22778=CARTESIAN_POINT('Ctrl Pts',(0.585373918991617,1.,2.08616943727951));
#22779=CARTESIAN_POINT('Ctrl Pts',(0.589962365403406,-1.,2.09064881812129));
#22780=CARTESIAN_POINT('Ctrl Pts',(0.589962365403406,1.,2.09064881812129));
#22781=CARTESIAN_POINT('Ctrl Pts',(0.594585006052162,-1.,2.0951087622027));
#22782=CARTESIAN_POINT('Ctrl Pts',(0.594585006052162,1.,2.0951087622027));
#22783=CARTESIAN_POINT('Ctrl Pts',(0.599241616420533,-1.,2.0995493086477));
#22784=CARTESIAN_POINT('Ctrl Pts',(0.599241616420533,1.,2.0995493086477));
#22785=CARTESIAN_POINT('Ctrl Pts',(0.60393203073603,-1.,2.10397049886949));
#22786=CARTESIAN_POINT('Ctrl Pts',(0.60393203073603,1.,2.10397049886949));
#22787=CARTESIAN_POINT('Ctrl Pts',(0.607711315454876,-1.,2.1074919961518));
#22788=CARTESIAN_POINT('Ctrl Pts',(0.607711315454876,1.,2.1074919961518));
#22789=CARTESIAN_POINT('Ctrl Pts',(0.610560911689898,-1.,2.11012443807238));
#22790=CARTESIAN_POINT('Ctrl Pts',(0.610560911689898,1.,2.11012443807238));
#22791=CARTESIAN_POINT('Ctrl Pts',(0.6124673655618,-1.,2.11187554259986));
#22792=CARTESIAN_POINT('Ctrl Pts',(0.6124673655618,1.,2.11187554259986));
#22793=CARTESIAN_POINT('Ctrl Pts',(0.61342227326009,-1.,2.11275013067528));
#22794=CARTESIAN_POINT('Ctrl Pts',(0.61342227326009,1.,2.11275013067528));
#22795=CARTESIAN_POINT('',(0.383122945602004,1.,1.7075470150345));
#22796=CARTESIAN_POINT('Ctrl Pts',(0.383122945602004,1.,1.7075470150345));
#22797=CARTESIAN_POINT('Ctrl Pts',(0.384119047315541,1.,1.71231062891958));
#22798=CARTESIAN_POINT('Ctrl Pts',(0.38607079032701,1.,1.72162022246158));
#22799=CARTESIAN_POINT('Ctrl Pts',(0.388877023509191,1.,1.7349317097561));
#22800=CARTESIAN_POINT('Ctrl Pts',(0.392375812294307,1.,1.75137405313962));
#22801=CARTESIAN_POINT('Ctrl Pts',(0.39634619612042,1.,1.7697556004756));
#22802=CARTESIAN_POINT('Ctrl Pts',(0.39991940378308,1.,1.78598826347533));
#22803=CARTESIAN_POINT('Ctrl Pts',(0.403107976170441,1.,1.80012077176221));
#22804=CARTESIAN_POINT('Ctrl Pts',(0.405933518411838,1.,1.81223801813988));
#22805=CARTESIAN_POINT('Ctrl Pts',(0.408428948108533,1.,1.8224702267854));
#22806=CARTESIAN_POINT('Ctrl Pts',(0.410641256301674,1.,1.83100408895216));
#22807=CARTESIAN_POINT('Ctrl Pts',(0.412633125322161,1.,1.83808953475839));
#22808=CARTESIAN_POINT('Ctrl Pts',(0.41448743825434,1.,1.8440575707371));
#22809=CARTESIAN_POINT('Ctrl Pts',(0.416300022038864,1.,1.84929312929882));
#22810=CARTESIAN_POINT('Ctrl Pts',(0.418164129143534,1.,1.85417632856234));
#22811=CARTESIAN_POINT('Ctrl Pts',(0.420157287975619,1.,1.85903281096686));
#22812=CARTESIAN_POINT('Ctrl Pts',(0.422327307418275,1.,1.86408083334028));
#22813=CARTESIAN_POINT('Ctrl Pts',(0.424678177291358,1.,1.86937803944323));
#22814=CARTESIAN_POINT('Ctrl Pts',(0.427183828519102,1.,1.87486989291484));
#22815=CARTESIAN_POINT('Ctrl Pts',(0.429803062482344,1.,1.88044229001832));
#22816=CARTESIAN_POINT('Ctrl Pts',(0.432493038548748,1.,1.88596913666793));
#22817=CARTESIAN_POINT('Ctrl Pts',(0.435225660963383,1.,1.89136993975504));
#22818=CARTESIAN_POINT('Ctrl Pts',(0.437995003948244,1.,1.89663648956466));
#22819=CARTESIAN_POINT('Ctrl Pts',(0.440807833704038,1.,1.90180124389086));
#22820=CARTESIAN_POINT('Ctrl Pts',(0.44367755684915,1.,1.90691756144898));
#22821=CARTESIAN_POINT('Ctrl Pts',(0.446617343485711,1.,1.9120369998112));
#22822=CARTESIAN_POINT('Ctrl Pts',(0.449632260106662,1.,1.91718342555755));
#22823=CARTESIAN_POINT('Ctrl Pts',(0.452719478359432,1.,1.92235380648502));
#22824=CARTESIAN_POINT('Ctrl Pts',(0.45587200517437,1.,1.92753067150476));
#22825=CARTESIAN_POINT('Ctrl Pts',(0.459081234547926,1.,1.93269066517934));
#22826=CARTESIAN_POINT('Ctrl Pts',(0.462340031009056,1.,1.93781486640821));
#22827=CARTESIAN_POINT('Ctrl Pts',(0.46564546202603,1.,1.9428979419619));
#22828=CARTESIAN_POINT('Ctrl Pts',(0.468997482913135,1.,1.94794381136514));
#22829=CARTESIAN_POINT('Ctrl Pts',(0.472397672264072,1.,1.95296148278133));
#22830=CARTESIAN_POINT('Ctrl Pts',(0.475848034683176,1.,1.95796111148177));
#22831=CARTESIAN_POINT('Ctrl Pts',(0.479349583074855,1.,1.96294933055943));
#22832=CARTESIAN_POINT('Ctrl Pts',(0.48290166212069,1.,1.96792703422362));
#22833=CARTESIAN_POINT('Ctrl Pts',(0.486502692907658,1.,1.97289186263272));
#22834=CARTESIAN_POINT('Ctrl Pts',(0.490150627860952,1.,1.97783973019229));
#22835=CARTESIAN_POINT('Ctrl Pts',(0.493843476541494,1.,1.98276658761821));
#22836=CARTESIAN_POINT('Ctrl Pts',(0.497579909545574,1.,1.98767044752932));
#22837=CARTESIAN_POINT('Ctrl Pts',(0.501359287727146,1.,1.99255149126155));
#22838=CARTESIAN_POINT('Ctrl Pts',(0.505181361323026,1.,1.99741107463572));
#22839=CARTESIAN_POINT('Ctrl Pts',(0.509046069886157,1.,2.00225107134734));
#22840=CARTESIAN_POINT('Ctrl Pts',(0.512953306961792,1.,2.00707309946949));
#22841=CARTESIAN_POINT('Ctrl Pts',(0.516902681728687,1.,2.01187773939242));
#22842=CARTESIAN_POINT('Ctrl Pts',(0.52089359039937,1.,2.01666477917286));
#22843=CARTESIAN_POINT('Ctrl Pts',(0.524925318333476,1.,2.02143356304698));
#22844=CARTESIAN_POINT('Ctrl Pts',(0.528997127241914,1.,2.0261832908329));
#22845=CARTESIAN_POINT('Ctrl Pts',(0.533108355132976,1.,2.03091336214426));
#22846=CARTESIAN_POINT('Ctrl Pts',(0.537258489833262,1.,2.03562362954037));
#22847=CARTESIAN_POINT('Ctrl Pts',(0.541447120615659,1.,2.04031422690527));
#22848=CARTESIAN_POINT('Ctrl Pts',(0.54567390381743,1.,2.04498544714588));
#22849=CARTESIAN_POINT('Ctrl Pts',(0.549938525150295,1.,2.04963761077958));
#22850=CARTESIAN_POINT('Ctrl Pts',(0.554240657463906,1.,2.05427091604413));
#22851=CARTESIAN_POINT('Ctrl Pts',(0.558579940185151,1.,2.05888537756462));
#22852=CARTESIAN_POINT('Ctrl Pts',(0.562955993082261,1.,2.06348090160589));
#22853=CARTESIAN_POINT('Ctrl Pts',(0.567368421181087,1.,2.06805732997334));
#22854=CARTESIAN_POINT('Ctrl Pts',(0.571816823242602,1.,2.07261449292824));
#22855=CARTESIAN_POINT('Ctrl Pts',(0.576300797416844,1.,2.07715226767559));
#22856=CARTESIAN_POINT('Ctrl Pts',(0.580819952108063,1.,2.08167059018418));
#22857=CARTESIAN_POINT('Ctrl Pts',(0.585373918991617,1.,2.08616943727951));
#22858=CARTESIAN_POINT('Ctrl Pts',(0.589962365403406,1.,2.09064881812129));
#22859=CARTESIAN_POINT('Ctrl Pts',(0.594585006052162,1.,2.0951087622027));
#22860=CARTESIAN_POINT('Ctrl Pts',(0.599241616420533,1.,2.0995493086477));
#22861=CARTESIAN_POINT('Ctrl Pts',(0.60393203073603,1.,2.10397049886949));
#22862=CARTESIAN_POINT('Ctrl Pts',(0.607711315454876,1.,2.1074919961518));
#22863=CARTESIAN_POINT('Ctrl Pts',(0.610560911689898,1.,2.11012443807238));
#22864=CARTESIAN_POINT('Ctrl Pts',(0.6124673655618,1.,2.11187554259986));
#22865=CARTESIAN_POINT('Ctrl Pts',(0.61342227326009,1.,2.11275013067528));
#22866=CARTESIAN_POINT('',(0.383122945602003,0.,1.7075470150345));
#22867=CARTESIAN_POINT('Origin',(0.,0.,0.));
#22868=CARTESIAN_POINT('',(0.163289472382896,1.,1.74236521665491));
#22869=CARTESIAN_POINT('Origin',(0.,1.,0.));
#22870=CARTESIAN_POINT('',(0.163289472382896,0.,1.74236521665491));
#22871=CARTESIAN_POINT('Ctrl Pts',(0.0694764450219578,-1.,2.19890268624765));
#22872=CARTESIAN_POINT('Ctrl Pts',(0.0694764450219578,1.,2.19890268624765));
#22873=CARTESIAN_POINT('Ctrl Pts',(0.0701143536325487,-1.,2.19777582085423));
#22874=CARTESIAN_POINT('Ctrl Pts',(0.0701143536325487,1.,2.19777582085423));
#22875=CARTESIAN_POINT('Ctrl Pts',(0.0713863779526151,-1.,2.19552129484002));
#22876=CARTESIAN_POINT('Ctrl Pts',(0.0713863779526151,1.,2.19552129484002));
#22877=CARTESIAN_POINT('Ctrl Pts',(0.0732830357306722,-1.,2.19213712013662));
#22878=CARTESIAN_POINT('Ctrl Pts',(0.0732830357306722,1.,2.19213712013662));
#22879=CARTESIAN_POINT('Ctrl Pts',(0.0757891465836145,-1.,2.1876201139953));
#22880=CARTESIAN_POINT('Ctrl Pts',(0.0757891465836145,1.,2.1876201139953));
#22881=CARTESIAN_POINT('Ctrl Pts',(0.078883772768524,-1.,2.18196589448887));
#22882=CARTESIAN_POINT('Ctrl Pts',(0.078883772768524,1.,2.18196589448887));
#22883=CARTESIAN_POINT('Ctrl Pts',(0.0819402680872763,-1.,2.176303712113));
#22884=CARTESIAN_POINT('Ctrl Pts',(0.0819402680872763,1.,2.176303712113));
#22885=CARTESIAN_POINT('Ctrl Pts',(0.084958462083537,-1.,2.17063357870952));
#22886=CARTESIAN_POINT('Ctrl Pts',(0.084958462083537,1.,2.17063357870952));
#22887=CARTESIAN_POINT('Ctrl Pts',(0.087938129138692,-1.,2.16495552645014));
#22888=CARTESIAN_POINT('Ctrl Pts',(0.087938129138692,1.,2.16495552645014));
#22889=CARTESIAN_POINT('Ctrl Pts',(0.0908789888107263,-1.,2.15926961544516));
#22890=CARTESIAN_POINT('Ctrl Pts',(0.0908789888107263,1.,2.15926961544516));
#22891=CARTESIAN_POINT('Ctrl Pts',(0.0937807218867641,-1.,2.1535759397817));
#22892=CARTESIAN_POINT('Ctrl Pts',(0.0937807218867641,1.,2.1535759397817));
#22893=CARTESIAN_POINT('Ctrl Pts',(0.0966429852305456,-1.,2.14787463531795));
#22894=CARTESIAN_POINT('Ctrl Pts',(0.0966429852305456,1.,2.14787463531795));
#22895=CARTESIAN_POINT('Ctrl Pts',(0.0994654261990913,-1.,2.14216588396025));
#22896=CARTESIAN_POINT('Ctrl Pts',(0.0994654261990913,1.,2.14216588396025));
#22897=CARTESIAN_POINT('Ctrl Pts',(0.1022477005561,-1.,2.13644992667165));
#22898=CARTESIAN_POINT('Ctrl Pts',(0.1022477005561,1.,2.13644992667165));
#22899=CARTESIAN_POINT('Ctrl Pts',(0.104989479152739,-1.,2.13072704887293));
#22900=CARTESIAN_POINT('Ctrl Pts',(0.104989479152739,1.,2.13072704887293));
#22901=CARTESIAN_POINT('Ctrl Pts',(0.10769043523109,-1.,2.12499752307));
#22902=CARTESIAN_POINT('Ctrl Pts',(0.10769043523109,1.,2.12499752307));
#22903=CARTESIAN_POINT('Ctrl Pts',(0.110350236135025,-1.,2.11926155590865));
#22904=CARTESIAN_POINT('Ctrl Pts',(0.110350236135025,1.,2.11926155590865));
#22905=CARTESIAN_POINT('Ctrl Pts',(0.112968534419737,-1.,2.11351924490306));
#22906=CARTESIAN_POINT('Ctrl Pts',(0.112968534419737,1.,2.11351924490306));
#22907=CARTESIAN_POINT('Ctrl Pts',(0.115544957687926,-1.,2.10777050261309));
#22908=CARTESIAN_POINT('Ctrl Pts',(0.115544957687926,1.,2.10777050261309));
#22909=CARTESIAN_POINT('Ctrl Pts',(0.118079107988355,-1.,2.102015121329));
#22910=CARTESIAN_POINT('Ctrl Pts',(0.118079107988355,1.,2.102015121329));
#22911=CARTESIAN_POINT('Ctrl Pts',(0.120570567965122,-1.,2.0962529286773));
#22912=CARTESIAN_POINT('Ctrl Pts',(0.120570567965122,1.,2.0962529286773));
#22913=CARTESIAN_POINT('Ctrl Pts',(0.123018905621083,-1.,2.09048392424825));
#22914=CARTESIAN_POINT('Ctrl Pts',(0.123018905621083,1.,2.09048392424825));
#22915=CARTESIAN_POINT('Ctrl Pts',(0.125423679412061,-1.,2.08470840653643));
#22916=CARTESIAN_POINT('Ctrl Pts',(0.125423679412061,1.,2.08470840653643));
#22917=CARTESIAN_POINT('Ctrl Pts',(0.12778444527612,-1.,2.07892715110987));
#22918=CARTESIAN_POINT('Ctrl Pts',(0.12778444527612,1.,2.07892715110987));
#22919=CARTESIAN_POINT('Ctrl Pts',(0.130100748328403,-1.,2.07314114713063));
#22920=CARTESIAN_POINT('Ctrl Pts',(0.130100748328403,1.,2.07314114713063));
#22921=CARTESIAN_POINT('Ctrl Pts',(0.13237211154771,-1.,2.06735123910326));
#22922=CARTESIAN_POINT('Ctrl Pts',(0.13237211154771,1.,2.06735123910326));
#22923=CARTESIAN_POINT('Ctrl Pts',(0.134598026192106,-1.,2.06155781517842));
#22924=CARTESIAN_POINT('Ctrl Pts',(0.134598026192106,1.,2.06155781517842));
#22925=CARTESIAN_POINT('Ctrl Pts',(0.136777941218043,-1.,2.05576044414264));
#22926=CARTESIAN_POINT('Ctrl Pts',(0.136777941218043,1.,2.05576044414264));
#22927=CARTESIAN_POINT('Ctrl Pts',(0.138911255368966,-1.,2.04995762001328));
#22928=CARTESIAN_POINT('Ctrl Pts',(0.138911255368966,1.,2.04995762001328));
#22929=CARTESIAN_POINT('Ctrl Pts',(0.140997332152546,-1.,2.04414757947916));
#22930=CARTESIAN_POINT('Ctrl Pts',(0.140997332152546,1.,2.04414757947916));
#22931=CARTESIAN_POINT('Ctrl Pts',(0.143035515058208,-1.,2.03832911025912));
#22932=CARTESIAN_POINT('Ctrl Pts',(0.143035515058208,1.,2.03832911025912));
#22933=CARTESIAN_POINT('Ctrl Pts',(0.145025140186057,-1.,2.03250223739942));
#22934=CARTESIAN_POINT('Ctrl Pts',(0.145025140186057,1.,2.03250223739942));
#22935=CARTESIAN_POINT('Ctrl Pts',(0.146965557332583,-1.,2.02666926182017));
#22936=CARTESIAN_POINT('Ctrl Pts',(0.146965557332583,1.,2.02666926182017));
#22937=CARTESIAN_POINT('Ctrl Pts',(0.148856124775337,-1.,2.02083464969894));
#22938=CARTESIAN_POINT('Ctrl Pts',(0.148856124775337,1.,2.02083464969894));
#22939=CARTESIAN_POINT('Ctrl Pts',(0.150696157673078,-1.,2.01500291940238));
#22940=CARTESIAN_POINT('Ctrl Pts',(0.150696157673078,1.,2.01500291940238));
#22941=CARTESIAN_POINT('Ctrl Pts',(0.152484883621449,-1.,2.00917680318424));
#22942=CARTESIAN_POINT('Ctrl Pts',(0.152484883621449,1.,2.00917680318424));
#22943=CARTESIAN_POINT('Ctrl Pts',(0.154221403049722,-1.,2.00335565310543));
#22944=CARTESIAN_POINT('Ctrl Pts',(0.154221403049722,1.,2.00335565310543));
#22945=CARTESIAN_POINT('Ctrl Pts',(0.155904629548783,-1.,1.99753284771497));
#22946=CARTESIAN_POINT('Ctrl Pts',(0.155904629548783,1.,1.99753284771497));
#22947=CARTESIAN_POINT('Ctrl Pts',(0.157533331459227,-1.,1.99169810931908));
#22948=CARTESIAN_POINT('Ctrl Pts',(0.157533331459227,1.,1.99169810931908));
#22949=CARTESIAN_POINT('Ctrl Pts',(0.159106226437299,-1.,1.98584238283292));
#22950=CARTESIAN_POINT('Ctrl Pts',(0.159106226437299,1.,1.98584238283292));
#22951=CARTESIAN_POINT('Ctrl Pts',(0.160622060784611,-1.,1.97996195437559));
#22952=CARTESIAN_POINT('Ctrl Pts',(0.160622060784611,1.,1.97996195437559));
#22953=CARTESIAN_POINT('Ctrl Pts',(0.162079693556288,-1.,1.97406280235188));
#22954=CARTESIAN_POINT('Ctrl Pts',(0.162079693556288,1.,1.97406280235188));
#22955=CARTESIAN_POINT('Ctrl Pts',(0.163478185457734,-1.,1.96816512677967));
#22956=CARTESIAN_POINT('Ctrl Pts',(0.163478185457734,1.,1.96816512677967));
#22957=CARTESIAN_POINT('Ctrl Pts',(0.164816568920269,-1.,1.96229379940136));
#22958=CARTESIAN_POINT('Ctrl Pts',(0.164816568920269,1.,1.96229379940136));
#22959=CARTESIAN_POINT('Ctrl Pts',(0.166093592002812,-1.,1.9564675971873));
#22960=CARTESIAN_POINT('Ctrl Pts',(0.166093592002812,1.,1.9564675971873));
#22961=CARTESIAN_POINT('Ctrl Pts',(0.167307501784475,-1.,1.95069027794294));
#22962=CARTESIAN_POINT('Ctrl Pts',(0.167307501784475,1.,1.95069027794294));
#22963=CARTESIAN_POINT('Ctrl Pts',(0.168455741607556,-1.,1.94493757756931));
#22964=CARTESIAN_POINT('Ctrl Pts',(0.168455741607556,1.,1.94493757756931));
#22965=CARTESIAN_POINT('Ctrl Pts',(0.16953490481749,-1.,1.93915639211581));
#22966=CARTESIAN_POINT('Ctrl Pts',(0.16953490481749,1.,1.93915639211581));
#22967=CARTESIAN_POINT('Ctrl Pts',(0.170541253116201,-1.,1.93329183155539));
#22968=CARTESIAN_POINT('Ctrl Pts',(0.170541253116201,1.,1.93329183155539));
#22969=CARTESIAN_POINT('Ctrl Pts',(0.171471191532988,-1.,1.92731093582036));
#22970=CARTESIAN_POINT('Ctrl Pts',(0.171471191532988,1.,1.92731093582036));
#22971=CARTESIAN_POINT('Ctrl Pts',(0.172321621259513,-1.,1.9212233439798));
#22972=CARTESIAN_POINT('Ctrl Pts',(0.172321621259513,1.,1.9212233439798));
#22973=CARTESIAN_POINT('Ctrl Pts',(0.173090695383496,-1.,1.91511429159527));
#22974=CARTESIAN_POINT('Ctrl Pts',(0.173090695383496,1.,1.91511429159527));
#22975=CARTESIAN_POINT('Ctrl Pts',(0.173776635257816,-1.,1.90911693975267));
#22976=CARTESIAN_POINT('Ctrl Pts',(0.173776635257816,1.,1.90911693975267));
#22977=CARTESIAN_POINT('Ctrl Pts',(0.174375518661085,-1.,1.90335253862834));
#22978=CARTESIAN_POINT('Ctrl Pts',(0.174375518661085,1.,1.90335253862834));
#22979=CARTESIAN_POINT('Ctrl Pts',(0.174879405091263,-1.,1.89788101117132));
#22980=CARTESIAN_POINT('Ctrl Pts',(0.174879405091263,1.,1.89788101117132));
#22981=CARTESIAN_POINT('Ctrl Pts',(0.175274276190844,-1.,1.892646301985));
#22982=CARTESIAN_POINT('Ctrl Pts',(0.175274276190844,1.,1.892646301985));
#22983=CARTESIAN_POINT('Ctrl Pts',(0.175538155840648,-1.,1.88742606273259));
#22984=CARTESIAN_POINT('Ctrl Pts',(0.175538155840648,1.,1.88742606273259));
#22985=CARTESIAN_POINT('Ctrl Pts',(0.175644148889698,-1.,1.88188663145367));
#22986=CARTESIAN_POINT('Ctrl Pts',(0.175644148889698,1.,1.88188663145367));
#22987=CARTESIAN_POINT('Ctrl Pts',(0.175563480746485,-1.,1.87563767773588));
#22988=CARTESIAN_POINT('Ctrl Pts',(0.175563480746485,1.,1.87563767773588));
#22989=CARTESIAN_POINT('Ctrl Pts',(0.175268337590757,-1.,1.86828349694799));
#22990=CARTESIAN_POINT('Ctrl Pts',(0.175268337590757,1.,1.86828349694799));
#22991=CARTESIAN_POINT('Ctrl Pts',(0.17473525927603,-1.,1.85948367088837));
#22992=CARTESIAN_POINT('Ctrl Pts',(0.17473525927603,1.,1.85948367088837));
#22993=CARTESIAN_POINT('Ctrl Pts',(0.173946627587731,-1.,1.8489811319852));
#22994=CARTESIAN_POINT('Ctrl Pts',(0.173946627587731,1.,1.8489811319852));
#22995=CARTESIAN_POINT('Ctrl Pts',(0.1728894428919,-1.,1.83658380527692));
#22996=CARTESIAN_POINT('Ctrl Pts',(0.1728894428919,1.,1.83658380527692));
#22997=CARTESIAN_POINT('Ctrl Pts',(0.171554770204119,-1.,1.82215766811545));
#22998=CARTESIAN_POINT('Ctrl Pts',(0.171554770204119,1.,1.82215766811545));
#22999=CARTESIAN_POINT('Ctrl Pts',(0.169936923904608,-1.,1.80561530629706));
#23000=CARTESIAN_POINT('Ctrl Pts',(0.169936923904608,1.,1.80561530629706));
#23001=CARTESIAN_POINT('Ctrl Pts',(0.168032772805197,-1.,1.7869064998507));
#23002=CARTESIAN_POINT('Ctrl Pts',(0.168032772805197,1.,1.7869064998507));
#23003=CARTESIAN_POINT('Ctrl Pts',(0.1662793551464,-1.,1.77018771684844));
#23004=CARTESIAN_POINT('Ctrl Pts',(0.1662793551464,1.,1.77018771684844));
#23005=CARTESIAN_POINT('Ctrl Pts',(0.164834765707158,-1.,1.75666056638427));
#23006=CARTESIAN_POINT('Ctrl Pts',(0.164834765707158,1.,1.75666056638427));
#23007=CARTESIAN_POINT('Ctrl Pts',(0.163814161002002,-1.,1.7472034950333));
#23008=CARTESIAN_POINT('Ctrl Pts',(0.163814161002002,1.,1.7472034950333));
#23009=CARTESIAN_POINT('Ctrl Pts',(0.163289472382896,-1.,1.74236521665491));
#23010=CARTESIAN_POINT('Ctrl Pts',(0.163289472382896,1.,1.74236521665491));
#23011=CARTESIAN_POINT('',(0.0694764450219578,1.,2.19890268624765));
#23012=CARTESIAN_POINT('Ctrl Pts',(0.0694764450219578,1.,2.19890268624765));
#23013=CARTESIAN_POINT('Ctrl Pts',(0.0701143536325487,1.,2.19777582085423));
#23014=CARTESIAN_POINT('Ctrl Pts',(0.0713863779526151,1.,2.19552129484002));
#23015=CARTESIAN_POINT('Ctrl Pts',(0.0732830357306722,1.,2.19213712013662));
#23016=CARTESIAN_POINT('Ctrl Pts',(0.0757891465836145,1.,2.1876201139953));
#23017=CARTESIAN_POINT('Ctrl Pts',(0.078883772768524,1.,2.18196589448887));
#23018=CARTESIAN_POINT('Ctrl Pts',(0.0819402680872763,1.,2.176303712113));
#23019=CARTESIAN_POINT('Ctrl Pts',(0.084958462083537,1.,2.17063357870952));
#23020=CARTESIAN_POINT('Ctrl Pts',(0.087938129138692,1.,2.16495552645014));
#23021=CARTESIAN_POINT('Ctrl Pts',(0.0908789888107263,1.,2.15926961544516));
#23022=CARTESIAN_POINT('Ctrl Pts',(0.0937807218867641,1.,2.1535759397817));
#23023=CARTESIAN_POINT('Ctrl Pts',(0.0966429852305456,1.,2.14787463531795));
#23024=CARTESIAN_POINT('Ctrl Pts',(0.0994654261990913,1.,2.14216588396025));
#23025=CARTESIAN_POINT('Ctrl Pts',(0.1022477005561,1.,2.13644992667165));
#23026=CARTESIAN_POINT('Ctrl Pts',(0.104989479152739,1.,2.13072704887293));
#23027=CARTESIAN_POINT('Ctrl Pts',(0.10769043523109,1.,2.12499752307));
#23028=CARTESIAN_POINT('Ctrl Pts',(0.110350236135025,1.,2.11926155590865));
#23029=CARTESIAN_POINT('Ctrl Pts',(0.112968534419737,1.,2.11351924490306));
#23030=CARTESIAN_POINT('Ctrl Pts',(0.115544957687926,1.,2.10777050261309));
#23031=CARTESIAN_POINT('Ctrl Pts',(0.118079107988355,1.,2.102015121329));
#23032=CARTESIAN_POINT('Ctrl Pts',(0.120570567965122,1.,2.0962529286773));
#23033=CARTESIAN_POINT('Ctrl Pts',(0.123018905621083,1.,2.09048392424825));
#23034=CARTESIAN_POINT('Ctrl Pts',(0.125423679412061,1.,2.08470840653643));
#23035=CARTESIAN_POINT('Ctrl Pts',(0.12778444527612,1.,2.07892715110987));
#23036=CARTESIAN_POINT('Ctrl Pts',(0.130100748328403,1.,2.07314114713063));
#23037=CARTESIAN_POINT('Ctrl Pts',(0.13237211154771,1.,2.06735123910326));
#23038=CARTESIAN_POINT('Ctrl Pts',(0.134598026192106,1.,2.06155781517842));
#23039=CARTESIAN_POINT('Ctrl Pts',(0.136777941218043,1.,2.05576044414264));
#23040=CARTESIAN_POINT('Ctrl Pts',(0.138911255368966,1.,2.04995762001328));
#23041=CARTESIAN_POINT('Ctrl Pts',(0.140997332152546,1.,2.04414757947916));
#23042=CARTESIAN_POINT('Ctrl Pts',(0.143035515058208,1.,2.03832911025912));
#23043=CARTESIAN_POINT('Ctrl Pts',(0.145025140186057,1.,2.03250223739942));
#23044=CARTESIAN_POINT('Ctrl Pts',(0.146965557332583,1.,2.02666926182017));
#23045=CARTESIAN_POINT('Ctrl Pts',(0.148856124775337,1.,2.02083464969894));
#23046=CARTESIAN_POINT('Ctrl Pts',(0.150696157673078,1.,2.01500291940238));
#23047=CARTESIAN_POINT('Ctrl Pts',(0.152484883621449,1.,2.00917680318424));
#23048=CARTESIAN_POINT('Ctrl Pts',(0.154221403049722,1.,2.00335565310543));
#23049=CARTESIAN_POINT('Ctrl Pts',(0.155904629548783,1.,1.99753284771497));
#23050=CARTESIAN_POINT('Ctrl Pts',(0.157533331459227,1.,1.99169810931908));
#23051=CARTESIAN_POINT('Ctrl Pts',(0.159106226437299,1.,1.98584238283292));
#23052=CARTESIAN_POINT('Ctrl Pts',(0.160622060784611,1.,1.97996195437559));
#23053=CARTESIAN_POINT('Ctrl Pts',(0.162079693556288,1.,1.97406280235188));
#23054=CARTESIAN_POINT('Ctrl Pts',(0.163478185457734,1.,1.96816512677967));
#23055=CARTESIAN_POINT('Ctrl Pts',(0.164816568920269,1.,1.96229379940136));
#23056=CARTESIAN_POINT('Ctrl Pts',(0.166093592002812,1.,1.9564675971873));
#23057=CARTESIAN_POINT('Ctrl Pts',(0.167307501784475,1.,1.95069027794294));
#23058=CARTESIAN_POINT('Ctrl Pts',(0.168455741607556,1.,1.94493757756931));
#23059=CARTESIAN_POINT('Ctrl Pts',(0.16953490481749,1.,1.93915639211581));
#23060=CARTESIAN_POINT('Ctrl Pts',(0.170541253116201,1.,1.93329183155539));
#23061=CARTESIAN_POINT('Ctrl Pts',(0.171471191532988,1.,1.92731093582036));
#23062=CARTESIAN_POINT('Ctrl Pts',(0.172321621259513,1.,1.9212233439798));
#23063=CARTESIAN_POINT('Ctrl Pts',(0.173090695383496,1.,1.91511429159527));
#23064=CARTESIAN_POINT('Ctrl Pts',(0.173776635257816,1.,1.90911693975267));
#23065=CARTESIAN_POINT('Ctrl Pts',(0.174375518661085,1.,1.90335253862834));
#23066=CARTESIAN_POINT('Ctrl Pts',(0.174879405091263,1.,1.89788101117132));
#23067=CARTESIAN_POINT('Ctrl Pts',(0.175274276190844,1.,1.892646301985));
#23068=CARTESIAN_POINT('Ctrl Pts',(0.175538155840648,1.,1.88742606273259));
#23069=CARTESIAN_POINT('Ctrl Pts',(0.175644148889698,1.,1.88188663145367));
#23070=CARTESIAN_POINT('Ctrl Pts',(0.175563480746485,1.,1.87563767773588));
#23071=CARTESIAN_POINT('Ctrl Pts',(0.175268337590757,1.,1.86828349694799));
#23072=CARTESIAN_POINT('Ctrl Pts',(0.17473525927603,1.,1.85948367088837));
#23073=CARTESIAN_POINT('Ctrl Pts',(0.173946627587731,1.,1.8489811319852));
#23074=CARTESIAN_POINT('Ctrl Pts',(0.1728894428919,1.,1.83658380527692));
#23075=CARTESIAN_POINT('Ctrl Pts',(0.171554770204119,1.,1.82215766811545));
#23076=CARTESIAN_POINT('Ctrl Pts',(0.169936923904608,1.,1.80561530629706));
#23077=CARTESIAN_POINT('Ctrl Pts',(0.168032772805197,1.,1.7869064998507));
#23078=CARTESIAN_POINT('Ctrl Pts',(0.1662793551464,1.,1.77018771684844));
#23079=CARTESIAN_POINT('Ctrl Pts',(0.164834765707158,1.,1.75666056638427));
#23080=CARTESIAN_POINT('Ctrl Pts',(0.163814161002002,1.,1.7472034950333));
#23081=CARTESIAN_POINT('Ctrl Pts',(0.163289472382896,1.,1.74236521665491));
#23082=CARTESIAN_POINT('',(0.0694764450219578,0.,2.19890268624765));
#23083=CARTESIAN_POINT('Origin',(-0.0694764450219586,0.,2.19890268624765));
#23084=CARTESIAN_POINT('',(-0.0694764450219586,1.,2.19890268624765));
#23085=CARTESIAN_POINT('',(0.0694764450219578,1.,2.19890268624765));
#23086=CARTESIAN_POINT('',(-0.0694764450219586,0.,2.19890268624765));
#23087=CARTESIAN_POINT('Ctrl Pts',(-0.163289472382896,-1.,1.74236521665491));
#23088=CARTESIAN_POINT('Ctrl Pts',(-0.163289472382896,1.,1.74236521665491));
#23089=CARTESIAN_POINT('Ctrl Pts',(-0.163814161002474,-1.,1.74720349503904));
#23090=CARTESIAN_POINT('Ctrl Pts',(-0.163814161002474,1.,1.74720349503904));
#23091=CARTESIAN_POINT('Ctrl Pts',(-0.164834765708484,-1.,1.75666056640041));
#23092=CARTESIAN_POINT('Ctrl Pts',(-0.164834765708484,1.,1.75666056640041));
#23093=CARTESIAN_POINT('Ctrl Pts',(-0.166279355148738,-1.,1.77018771687692));
#23094=CARTESIAN_POINT('Ctrl Pts',(-0.166279355148738,1.,1.77018771687692));
#23095=CARTESIAN_POINT('Ctrl Pts',(-0.16803277280837,-1.,1.78690649988931));
#23096=CARTESIAN_POINT('Ctrl Pts',(-0.16803277280837,1.,1.78690649988931));
#23097=CARTESIAN_POINT('Ctrl Pts',(-0.169936923908078,-1.,1.80561530633924));
#23098=CARTESIAN_POINT('Ctrl Pts',(-0.169936923908078,1.,1.80561530633924));
#23099=CARTESIAN_POINT('Ctrl Pts',(-0.171554770207306,-1.,1.82215766815414));
#23100=CARTESIAN_POINT('Ctrl Pts',(-0.171554770207306,1.,1.82215766815414));
#23101=CARTESIAN_POINT('Ctrl Pts',(-0.17288944289442,-1.,1.83658380530747));
#23102=CARTESIAN_POINT('Ctrl Pts',(-0.17288944289442,1.,1.83658380530747));
#23103=CARTESIAN_POINT('Ctrl Pts',(-0.173946627589401,-1.,1.84898113200543));
#23104=CARTESIAN_POINT('Ctrl Pts',(-0.173946627589401,1.,1.84898113200543));
#23105=CARTESIAN_POINT('Ctrl Pts',(-0.174735259276856,-1.,1.85948367089838));
#23106=CARTESIAN_POINT('Ctrl Pts',(-0.174735259276856,1.,1.85948367089838));
#23107=CARTESIAN_POINT('Ctrl Pts',(-0.175268337590901,-1.,1.86828349694972));
#23108=CARTESIAN_POINT('Ctrl Pts',(-0.175268337590901,1.,1.86828349694972));
#23109=CARTESIAN_POINT('Ctrl Pts',(-0.175563480746206,-1.,1.87563767773249));
#23110=CARTESIAN_POINT('Ctrl Pts',(-0.175563480746206,1.,1.87563767773249));
#23111=CARTESIAN_POINT('Ctrl Pts',(-0.175644148889271,-1.,1.88188663144846));
#23112=CARTESIAN_POINT('Ctrl Pts',(-0.175644148889271,1.,1.88188663144846));
#23113=CARTESIAN_POINT('Ctrl Pts',(-0.175538155840286,-1.,1.88742606272818));
#23114=CARTESIAN_POINT('Ctrl Pts',(-0.175538155840286,1.,1.88742606272818));
#23115=CARTESIAN_POINT('Ctrl Pts',(-0.175274276190664,-1.,1.89264630198279));
#23116=CARTESIAN_POINT('Ctrl Pts',(-0.175274276190664,1.,1.89264630198279));
#23117=CARTESIAN_POINT('Ctrl Pts',(-0.174879405091277,-1.,1.89788101117148));
#23118=CARTESIAN_POINT('Ctrl Pts',(-0.174879405091277,1.,1.89788101117148));
#23119=CARTESIAN_POINT('Ctrl Pts',(-0.174375518661222,-1.,1.90335253863003));
#23120=CARTESIAN_POINT('Ctrl Pts',(-0.174375518661222,1.,1.90335253863003));
#23121=CARTESIAN_POINT('Ctrl Pts',(-0.173776635257984,-1.,1.90911693975475));
#23122=CARTESIAN_POINT('Ctrl Pts',(-0.173776635257984,1.,1.90911693975475));
#23123=CARTESIAN_POINT('Ctrl Pts',(-0.173090695383619,-1.,1.91511429159681));
#23124=CARTESIAN_POINT('Ctrl Pts',(-0.173090695383619,1.,1.91511429159681));
#23125=CARTESIAN_POINT('Ctrl Pts',(-0.172321621259557,-1.,1.92122334398034));
#23126=CARTESIAN_POINT('Ctrl Pts',(-0.172321621259557,1.,1.92122334398034));
#23127=CARTESIAN_POINT('Ctrl Pts',(-0.17147119153296,-1.,1.92731093582));
#23128=CARTESIAN_POINT('Ctrl Pts',(-0.17147119153296,1.,1.92731093582));
#23129=CARTESIAN_POINT('Ctrl Pts',(-0.170541253116136,-1.,1.93329183155455));
#23130=CARTESIAN_POINT('Ctrl Pts',(-0.170541253116136,1.,1.93329183155455));
#23131=CARTESIAN_POINT('Ctrl Pts',(-0.169534904817425,-1.,1.93915639211497));
#23132=CARTESIAN_POINT('Ctrl Pts',(-0.169534904817425,1.,1.93915639211497));
#23133=CARTESIAN_POINT('Ctrl Pts',(-0.168455741607516,-1.,1.94493757756879));
#23134=CARTESIAN_POINT('Ctrl Pts',(-0.168455741607516,1.,1.94493757756879));
#23135=CARTESIAN_POINT('Ctrl Pts',(-0.167307501784469,-1.,1.95069027794286));
#23136=CARTESIAN_POINT('Ctrl Pts',(-0.167307501784469,1.,1.95069027794286));
#23137=CARTESIAN_POINT('Ctrl Pts',(-0.166093592002833,-1.,1.95646759718755));
#23138=CARTESIAN_POINT('Ctrl Pts',(-0.166093592002833,1.,1.95646759718755));
#23139=CARTESIAN_POINT('Ctrl Pts',(-0.1648165689203,-1.,1.96229379940174));
#23140=CARTESIAN_POINT('Ctrl Pts',(-0.1648165689203,1.,1.96229379940174));
#23141=CARTESIAN_POINT('Ctrl Pts',(-0.16347818545776,-1.,1.96816512678));
#23142=CARTESIAN_POINT('Ctrl Pts',(-0.16347818545776,1.,1.96816512678));
#23143=CARTESIAN_POINT('Ctrl Pts',(-0.162079693556302,-1.,1.97406280235204));
#23144=CARTESIAN_POINT('Ctrl Pts',(-0.162079693556302,1.,1.97406280235204));
#23145=CARTESIAN_POINT('Ctrl Pts',(-0.16062206078461,-1.,1.97996195437557));
#23146=CARTESIAN_POINT('Ctrl Pts',(-0.16062206078461,1.,1.97996195437557));
#23147=CARTESIAN_POINT('Ctrl Pts',(-0.159106226437289,-1.,1.98584238283279));
#23148=CARTESIAN_POINT('Ctrl Pts',(-0.159106226437289,1.,1.98584238283279));
#23149=CARTESIAN_POINT('Ctrl Pts',(-0.157533331459215,-1.,1.99169810931893));
#23150=CARTESIAN_POINT('Ctrl Pts',(-0.157533331459215,1.,1.99169810931893));
#23151=CARTESIAN_POINT('Ctrl Pts',(-0.155904629548775,-1.,1.99753284771487));
#23152=CARTESIAN_POINT('Ctrl Pts',(-0.155904629548775,1.,1.99753284771487));
#23153=CARTESIAN_POINT('Ctrl Pts',(-0.154221403049719,-1.,2.00335565310539));
#23154=CARTESIAN_POINT('Ctrl Pts',(-0.154221403049719,1.,2.00335565310539));
#23155=CARTESIAN_POINT('Ctrl Pts',(-0.152484883621452,-1.,2.00917680318426));
#23156=CARTESIAN_POINT('Ctrl Pts',(-0.152484883621452,1.,2.00917680318426));
#23157=CARTESIAN_POINT('Ctrl Pts',(-0.150696157673084,-1.,2.01500291940243));
#23158=CARTESIAN_POINT('Ctrl Pts',(-0.150696157673084,1.,2.01500291940243));
#23159=CARTESIAN_POINT('Ctrl Pts',(-0.148856124775343,-1.,2.02083464969897));
#23160=CARTESIAN_POINT('Ctrl Pts',(-0.148856124775343,1.,2.02083464969897));
#23161=CARTESIAN_POINT('Ctrl Pts',(-0.146965557332586,-1.,2.02666926182017));
#23162=CARTESIAN_POINT('Ctrl Pts',(-0.146965557332586,1.,2.02666926182017));
#23163=CARTESIAN_POINT('Ctrl Pts',(-0.145025140186058,-1.,2.03250223739941));
#23164=CARTESIAN_POINT('Ctrl Pts',(-0.145025140186058,1.,2.03250223739941));
#23165=CARTESIAN_POINT('Ctrl Pts',(-0.143035515058208,-1.,2.03832911025913));
#23166=CARTESIAN_POINT('Ctrl Pts',(-0.143035515058208,1.,2.03832911025913));
#23167=CARTESIAN_POINT('Ctrl Pts',(-0.140997332152546,-1.,2.04414757947919));
#23168=CARTESIAN_POINT('Ctrl Pts',(-0.140997332152546,1.,2.04414757947919));
#23169=CARTESIAN_POINT('Ctrl Pts',(-0.138911255368966,-1.,2.04995762001333));
#23170=CARTESIAN_POINT('Ctrl Pts',(-0.138911255368966,1.,2.04995762001333));
#23171=CARTESIAN_POINT('Ctrl Pts',(-0.136777941218044,-1.,2.0557604441427));
#23172=CARTESIAN_POINT('Ctrl Pts',(-0.136777941218044,1.,2.0557604441427));
#23173=CARTESIAN_POINT('Ctrl Pts',(-0.134598026192107,-1.,2.06155781517844));
#23174=CARTESIAN_POINT('Ctrl Pts',(-0.134598026192107,1.,2.06155781517844));
#23175=CARTESIAN_POINT('Ctrl Pts',(-0.13237211154771,-1.,2.06735123910319));
#23176=CARTESIAN_POINT('Ctrl Pts',(-0.13237211154771,1.,2.06735123910319));
#23177=CARTESIAN_POINT('Ctrl Pts',(-0.130100748328401,-1.,2.07314114713047));
#23178=CARTESIAN_POINT('Ctrl Pts',(-0.130100748328401,1.,2.07314114713047));
#23179=CARTESIAN_POINT('Ctrl Pts',(-0.127784445276116,-1.,2.07892715110967));
#23180=CARTESIAN_POINT('Ctrl Pts',(-0.127784445276116,1.,2.07892715110967));
#23181=CARTESIAN_POINT('Ctrl Pts',(-0.125423679412058,-1.,2.08470840653628));
#23182=CARTESIAN_POINT('Ctrl Pts',(-0.125423679412058,1.,2.08470840653628));
#23183=CARTESIAN_POINT('Ctrl Pts',(-0.123018905621083,-1.,2.09048392424826));
#23184=CARTESIAN_POINT('Ctrl Pts',(-0.123018905621083,1.,2.09048392424826));
#23185=CARTESIAN_POINT('Ctrl Pts',(-0.120570567965129,-1.,2.09625292867756));
#23186=CARTESIAN_POINT('Ctrl Pts',(-0.120570567965129,1.,2.09625292867756));
#23187=CARTESIAN_POINT('Ctrl Pts',(-0.118079107988368,-1.,2.10201512132945));
#23188=CARTESIAN_POINT('Ctrl Pts',(-0.118079107988368,1.,2.10201512132945));
#23189=CARTESIAN_POINT('Ctrl Pts',(-0.115544957687941,-1.,2.10777050261359));
#23190=CARTESIAN_POINT('Ctrl Pts',(-0.115544957687941,1.,2.10777050261359));
#23191=CARTESIAN_POINT('Ctrl Pts',(-0.112968534419746,-1.,2.11351924490335));
#23192=CARTESIAN_POINT('Ctrl Pts',(-0.112968534419746,1.,2.11351924490335));
#23193=CARTESIAN_POINT('Ctrl Pts',(-0.11035023613502,-1.,2.11926155590849));
#23194=CARTESIAN_POINT('Ctrl Pts',(-0.11035023613502,1.,2.11926155590849));
#23195=CARTESIAN_POINT('Ctrl Pts',(-0.107690435231068,-1.,2.12499752306927));
#23196=CARTESIAN_POINT('Ctrl Pts',(-0.107690435231068,1.,2.12499752306927));
#23197=CARTESIAN_POINT('Ctrl Pts',(-0.104989479152703,-1.,2.1307270488718));
#23198=CARTESIAN_POINT('Ctrl Pts',(-0.104989479152703,1.,2.1307270488718));
#23199=CARTESIAN_POINT('Ctrl Pts',(-0.102247700556064,-1.,2.13644992667052));
#23200=CARTESIAN_POINT('Ctrl Pts',(-0.102247700556064,1.,2.13644992667052));
#23201=CARTESIAN_POINT('Ctrl Pts',(-0.0994654261990745,-1.,2.14216588395974));
#23202=CARTESIAN_POINT('Ctrl Pts',(-0.0994654261990745,1.,2.14216588395974));
#23203=CARTESIAN_POINT('Ctrl Pts',(-0.0966429852305691,-1.,2.14787463531864));
#23204=CARTESIAN_POINT('Ctrl Pts',(-0.0966429852305691,1.,2.14787463531864));
#23205=CARTESIAN_POINT('Ctrl Pts',(-0.0937807218868348,-1.,2.15357593978377));
#23206=CARTESIAN_POINT('Ctrl Pts',(-0.0937807218868348,1.,2.15357593978377));
#23207=CARTESIAN_POINT('Ctrl Pts',(-0.0908789888108269,-1.,2.15926961544808));
#23208=CARTESIAN_POINT('Ctrl Pts',(-0.0908789888108269,1.,2.15926961544808));
#23209=CARTESIAN_POINT('Ctrl Pts',(-0.0879381291387825,-1.,2.16495552645275));
#23210=CARTESIAN_POINT('Ctrl Pts',(-0.0879381291387825,1.,2.16495552645275));
#23211=CARTESIAN_POINT('Ctrl Pts',(-0.0849584620835646,-1.,2.17063357871031));
#23212=CARTESIAN_POINT('Ctrl Pts',(-0.0849584620835646,1.,2.17063357871031));
#23213=CARTESIAN_POINT('Ctrl Pts',(-0.0819402680871942,-1.,2.1763037121106));
#23214=CARTESIAN_POINT('Ctrl Pts',(-0.0819402680871942,1.,2.1763037121106));
#23215=CARTESIAN_POINT('Ctrl Pts',(-0.078883772768323,-1.,2.18196589448304));
#23216=CARTESIAN_POINT('Ctrl Pts',(-0.078883772768323,1.,2.18196589448304));
#23217=CARTESIAN_POINT('Ctrl Pts',(-0.0757891465833414,-1.,2.1876201139874));
#23218=CARTESIAN_POINT('Ctrl Pts',(-0.0757891465833414,1.,2.1876201139874));
#23219=CARTESIAN_POINT('Ctrl Pts',(-0.0732830357304279,-1.,2.19213712012956));
#23220=CARTESIAN_POINT('Ctrl Pts',(-0.0732830357304279,1.,2.19213712012956));
#23221=CARTESIAN_POINT('Ctrl Pts',(-0.071386377952463,-1.,2.19552129483562));
#23222=CARTESIAN_POINT('Ctrl Pts',(-0.071386377952463,1.,2.19552129483562));
#23223=CARTESIAN_POINT('Ctrl Pts',(-0.0701143536324929,-1.,2.19777582085261));
#23224=CARTESIAN_POINT('Ctrl Pts',(-0.0701143536324929,1.,2.19777582085261));
#23225=CARTESIAN_POINT('Ctrl Pts',(-0.0694764450219586,-1.,2.19890268624765));
#23226=CARTESIAN_POINT('Ctrl Pts',(-0.0694764450219586,1.,2.19890268624765));
#23227=CARTESIAN_POINT('',(-0.163289472382896,1.,1.74236521665491));
#23228=CARTESIAN_POINT('Ctrl Pts',(-0.163289472382896,1.,1.74236521665491));
#23229=CARTESIAN_POINT('Ctrl Pts',(-0.163814161002474,1.,1.74720349503904));
#23230=CARTESIAN_POINT('Ctrl Pts',(-0.164834765708484,1.,1.75666056640041));
#23231=CARTESIAN_POINT('Ctrl Pts',(-0.166279355148738,1.,1.77018771687692));
#23232=CARTESIAN_POINT('Ctrl Pts',(-0.16803277280837,1.,1.78690649988931));
#23233=CARTESIAN_POINT('Ctrl Pts',(-0.169936923908078,1.,1.80561530633924));
#23234=CARTESIAN_POINT('Ctrl Pts',(-0.171554770207306,1.,1.82215766815414));
#23235=CARTESIAN_POINT('Ctrl Pts',(-0.17288944289442,1.,1.83658380530747));
#23236=CARTESIAN_POINT('Ctrl Pts',(-0.173946627589401,1.,1.84898113200543));
#23237=CARTESIAN_POINT('Ctrl Pts',(-0.174735259276856,1.,1.85948367089838));
#23238=CARTESIAN_POINT('Ctrl Pts',(-0.175268337590901,1.,1.86828349694972));
#23239=CARTESIAN_POINT('Ctrl Pts',(-0.175563480746206,1.,1.87563767773249));
#23240=CARTESIAN_POINT('Ctrl Pts',(-0.175644148889271,1.,1.88188663144846));
#23241=CARTESIAN_POINT('Ctrl Pts',(-0.175538155840286,1.,1.88742606272818));
#23242=CARTESIAN_POINT('Ctrl Pts',(-0.175274276190664,1.,1.89264630198279));
#23243=CARTESIAN_POINT('Ctrl Pts',(-0.174879405091277,1.,1.89788101117148));
#23244=CARTESIAN_POINT('Ctrl Pts',(-0.174375518661222,1.,1.90335253863003));
#23245=CARTESIAN_POINT('Ctrl Pts',(-0.173776635257984,1.,1.90911693975475));
#23246=CARTESIAN_POINT('Ctrl Pts',(-0.173090695383619,1.,1.91511429159681));
#23247=CARTESIAN_POINT('Ctrl Pts',(-0.172321621259557,1.,1.92122334398034));
#23248=CARTESIAN_POINT('Ctrl Pts',(-0.17147119153296,1.,1.92731093582));
#23249=CARTESIAN_POINT('Ctrl Pts',(-0.170541253116136,1.,1.93329183155455));
#23250=CARTESIAN_POINT('Ctrl Pts',(-0.169534904817425,1.,1.93915639211497));
#23251=CARTESIAN_POINT('Ctrl Pts',(-0.168455741607516,1.,1.94493757756879));
#23252=CARTESIAN_POINT('Ctrl Pts',(-0.167307501784469,1.,1.95069027794286));
#23253=CARTESIAN_POINT('Ctrl Pts',(-0.166093592002833,1.,1.95646759718755));
#23254=CARTESIAN_POINT('Ctrl Pts',(-0.1648165689203,1.,1.96229379940174));
#23255=CARTESIAN_POINT('Ctrl Pts',(-0.16347818545776,1.,1.96816512678));
#23256=CARTESIAN_POINT('Ctrl Pts',(-0.162079693556302,1.,1.97406280235204));
#23257=CARTESIAN_POINT('Ctrl Pts',(-0.16062206078461,1.,1.97996195437557));
#23258=CARTESIAN_POINT('Ctrl Pts',(-0.159106226437289,1.,1.98584238283279));
#23259=CARTESIAN_POINT('Ctrl Pts',(-0.157533331459215,1.,1.99169810931893));
#23260=CARTESIAN_POINT('Ctrl Pts',(-0.155904629548775,1.,1.99753284771487));
#23261=CARTESIAN_POINT('Ctrl Pts',(-0.154221403049719,1.,2.00335565310539));
#23262=CARTESIAN_POINT('Ctrl Pts',(-0.152484883621452,1.,2.00917680318426));
#23263=CARTESIAN_POINT('Ctrl Pts',(-0.150696157673084,1.,2.01500291940243));
#23264=CARTESIAN_POINT('Ctrl Pts',(-0.148856124775343,1.,2.02083464969897));
#23265=CARTESIAN_POINT('Ctrl Pts',(-0.146965557332586,1.,2.02666926182017));
#23266=CARTESIAN_POINT('Ctrl Pts',(-0.145025140186058,1.,2.03250223739941));
#23267=CARTESIAN_POINT('Ctrl Pts',(-0.143035515058208,1.,2.03832911025913));
#23268=CARTESIAN_POINT('Ctrl Pts',(-0.140997332152546,1.,2.04414757947919));
#23269=CARTESIAN_POINT('Ctrl Pts',(-0.138911255368966,1.,2.04995762001333));
#23270=CARTESIAN_POINT('Ctrl Pts',(-0.136777941218044,1.,2.0557604441427));
#23271=CARTESIAN_POINT('Ctrl Pts',(-0.134598026192107,1.,2.06155781517844));
#23272=CARTESIAN_POINT('Ctrl Pts',(-0.13237211154771,1.,2.06735123910319));
#23273=CARTESIAN_POINT('Ctrl Pts',(-0.130100748328401,1.,2.07314114713047));
#23274=CARTESIAN_POINT('Ctrl Pts',(-0.127784445276116,1.,2.07892715110967));
#23275=CARTESIAN_POINT('Ctrl Pts',(-0.125423679412058,1.,2.08470840653628));
#23276=CARTESIAN_POINT('Ctrl Pts',(-0.123018905621083,1.,2.09048392424826));
#23277=CARTESIAN_POINT('Ctrl Pts',(-0.120570567965129,1.,2.09625292867756));
#23278=CARTESIAN_POINT('Ctrl Pts',(-0.118079107988368,1.,2.10201512132945));
#23279=CARTESIAN_POINT('Ctrl Pts',(-0.115544957687941,1.,2.10777050261359));
#23280=CARTESIAN_POINT('Ctrl Pts',(-0.112968534419746,1.,2.11351924490335));
#23281=CARTESIAN_POINT('Ctrl Pts',(-0.11035023613502,1.,2.11926155590849));
#23282=CARTESIAN_POINT('Ctrl Pts',(-0.107690435231068,1.,2.12499752306927));
#23283=CARTESIAN_POINT('Ctrl Pts',(-0.104989479152703,1.,2.1307270488718));
#23284=CARTESIAN_POINT('Ctrl Pts',(-0.102247700556064,1.,2.13644992667052));
#23285=CARTESIAN_POINT('Ctrl Pts',(-0.0994654261990745,1.,2.14216588395974));
#23286=CARTESIAN_POINT('Ctrl Pts',(-0.0966429852305691,1.,2.14787463531864));
#23287=CARTESIAN_POINT('Ctrl Pts',(-0.0937807218868348,1.,2.15357593978377));
#23288=CARTESIAN_POINT('Ctrl Pts',(-0.0908789888108269,1.,2.15926961544808));
#23289=CARTESIAN_POINT('Ctrl Pts',(-0.0879381291387825,1.,2.16495552645275));
#23290=CARTESIAN_POINT('Ctrl Pts',(-0.0849584620835646,1.,2.17063357871031));
#23291=CARTESIAN_POINT('Ctrl Pts',(-0.0819402680871942,1.,2.1763037121106));
#23292=CARTESIAN_POINT('Ctrl Pts',(-0.078883772768323,1.,2.18196589448304));
#23293=CARTESIAN_POINT('Ctrl Pts',(-0.0757891465833414,1.,2.1876201139874));
#23294=CARTESIAN_POINT('Ctrl Pts',(-0.0732830357304279,1.,2.19213712012956));
#23295=CARTESIAN_POINT('Ctrl Pts',(-0.071386377952463,1.,2.19552129483562));
#23296=CARTESIAN_POINT('Ctrl Pts',(-0.0701143536324929,1.,2.19777582085261));
#23297=CARTESIAN_POINT('Ctrl Pts',(-0.0694764450219586,1.,2.19890268624765));
#23298=CARTESIAN_POINT('',(-0.163289472382897,0.,1.74236521665491));
#23299=CARTESIAN_POINT('Origin',(0.,0.,0.));
#23300=CARTESIAN_POINT('',(-0.383122945602004,1.,1.7075470150345));
#23301=CARTESIAN_POINT('Origin',(0.,1.,0.));
#23302=CARTESIAN_POINT('',(-0.383122945602004,0.,1.7075470150345));
#23303=CARTESIAN_POINT('Ctrl Pts',(-0.61342227326009,-1.,2.11275013067528));
#23304=CARTESIAN_POINT('Ctrl Pts',(-0.61342227326009,1.,2.11275013067528));
#23305=CARTESIAN_POINT('Ctrl Pts',(-0.61246736556225,-1.,2.11187554260142));
#23306=CARTESIAN_POINT('Ctrl Pts',(-0.61246736556225,1.,2.11187554260142));
#23307=CARTESIAN_POINT('Ctrl Pts',(-0.610560911691113,-1.,2.11012443807661));
#23308=CARTESIAN_POINT('Ctrl Pts',(-0.610560911691113,1.,2.11012443807661));
#23309=CARTESIAN_POINT('Ctrl Pts',(-0.607711315456826,-1.,2.10749199615859));
#23310=CARTESIAN_POINT('Ctrl Pts',(-0.607711315456826,1.,2.10749199615859));
#23311=CARTESIAN_POINT('Ctrl Pts',(-0.603932030738212,-1.,2.10397049887709));
#23312=CARTESIAN_POINT('Ctrl Pts',(-0.603932030738212,1.,2.10397049887709));
#23313=CARTESIAN_POINT('Ctrl Pts',(-0.599241616422144,-1.,2.09954930865331));
#23314=CARTESIAN_POINT('Ctrl Pts',(-0.599241616422144,1.,2.09954930865331));
#23315=CARTESIAN_POINT('Ctrl Pts',(-0.594585006052824,-1.,2.09510876220501));
#23316=CARTESIAN_POINT('Ctrl Pts',(-0.594585006052824,1.,2.09510876220501));
#23317=CARTESIAN_POINT('Ctrl Pts',(-0.589962365403189,-1.,2.09064881812053));
#23318=CARTESIAN_POINT('Ctrl Pts',(-0.589962365403189,1.,2.09064881812053));
#23319=CARTESIAN_POINT('Ctrl Pts',(-0.585373918990895,-1.,2.086169437277));
#23320=CARTESIAN_POINT('Ctrl Pts',(-0.585373918990895,1.,2.086169437277));
#23321=CARTESIAN_POINT('Ctrl Pts',(-0.580819952107257,-1.,2.08167059018138));
#23322=CARTESIAN_POINT('Ctrl Pts',(-0.580819952107257,1.,2.08167059018138));
#23323=CARTESIAN_POINT('Ctrl Pts',(-0.576300797416275,-1.,2.07715226767361));
#23324=CARTESIAN_POINT('Ctrl Pts',(-0.576300797416275,1.,2.07715226767361));
#23325=CARTESIAN_POINT('Ctrl Pts',(-0.571816823242411,-1.,2.07261449292757));
#23326=CARTESIAN_POINT('Ctrl Pts',(-0.571816823242411,1.,2.07261449292757));
#23327=CARTESIAN_POINT('Ctrl Pts',(-0.567368421181229,-1.,2.06805732997383));
#23328=CARTESIAN_POINT('Ctrl Pts',(-0.567368421181229,1.,2.06805732997383));
#23329=CARTESIAN_POINT('Ctrl Pts',(-0.562955993082574,-1.,2.06348090160697));
#23330=CARTESIAN_POINT('Ctrl Pts',(-0.562955993082574,1.,2.06348090160697));
#23331=CARTESIAN_POINT('Ctrl Pts',(-0.558579940185467,-1.,2.05888537756571));
#23332=CARTESIAN_POINT('Ctrl Pts',(-0.558579940185467,1.,2.05888537756571));
#23333=CARTESIAN_POINT('Ctrl Pts',(-0.55424065746411,-1.,2.05427091604482));
#23334=CARTESIAN_POINT('Ctrl Pts',(-0.55424065746411,1.,2.05427091604482));
#23335=CARTESIAN_POINT('Ctrl Pts',(-0.549938525150342,-1.,2.04963761077974));
#23336=CARTESIAN_POINT('Ctrl Pts',(-0.549938525150342,1.,2.04963761077974));
#23337=CARTESIAN_POINT('Ctrl Pts',(-0.545673903817348,-1.,2.0449854471456));
#23338=CARTESIAN_POINT('Ctrl Pts',(-0.545673903817348,1.,2.0449854471456));
#23339=CARTESIAN_POINT('Ctrl Pts',(-0.54144712061552,-1.,2.0403142269048));
#23340=CARTESIAN_POINT('Ctrl Pts',(-0.54144712061552,1.,2.0403142269048));
#23341=CARTESIAN_POINT('Ctrl Pts',(-0.537258489833134,-1.,2.03562362953993));
#23342=CARTESIAN_POINT('Ctrl Pts',(-0.537258489833134,1.,2.03562362953993));
#23343=CARTESIAN_POINT('Ctrl Pts',(-0.533108355132905,-1.,2.03091336214401));
#23344=CARTESIAN_POINT('Ctrl Pts',(-0.533108355132905,1.,2.03091336214401));
#23345=CARTESIAN_POINT('Ctrl Pts',(-0.528997127241911,-1.,2.02618329083289));
#23346=CARTESIAN_POINT('Ctrl Pts',(-0.528997127241911,1.,2.02618329083289));
#23347=CARTESIAN_POINT('Ctrl Pts',(-0.524925318333518,-1.,2.02143356304712));
#23348=CARTESIAN_POINT('Ctrl Pts',(-0.524925318333518,1.,2.02143356304712));
#23349=CARTESIAN_POINT('Ctrl Pts',(-0.520893590399428,-1.,2.01666477917305));
#23350=CARTESIAN_POINT('Ctrl Pts',(-0.520893590399428,1.,2.01666477917305));
#23351=CARTESIAN_POINT('Ctrl Pts',(-0.516902681728733,-1.,2.01187773939257));
#23352=CARTESIAN_POINT('Ctrl Pts',(-0.516902681728733,1.,2.01187773939257));
#23353=CARTESIAN_POINT('Ctrl Pts',(-0.512953306961814,-1.,2.00707309946955));
#23354=CARTESIAN_POINT('Ctrl Pts',(-0.512953306961814,1.,2.00707309946955));
#23355=CARTESIAN_POINT('Ctrl Pts',(-0.509046069886152,-1.,2.00225107134733));
#23356=CARTESIAN_POINT('Ctrl Pts',(-0.509046069886152,1.,2.00225107134733));
#23357=CARTESIAN_POINT('Ctrl Pts',(-0.505181361323011,-1.,1.99741107463567));
#23358=CARTESIAN_POINT('Ctrl Pts',(-0.505181361323011,1.,1.99741107463567));
#23359=CARTESIAN_POINT('Ctrl Pts',(-0.501359287727129,-1.,1.9925514912615));
#23360=CARTESIAN_POINT('Ctrl Pts',(-0.501359287727129,1.,1.9925514912615));
#23361=CARTESIAN_POINT('Ctrl Pts',(-0.497579909545564,-1.,1.98767044752929));
#23362=CARTESIAN_POINT('Ctrl Pts',(-0.497579909545564,1.,1.98767044752929));
#23363=CARTESIAN_POINT('Ctrl Pts',(-0.493843476541492,-1.,1.9827665876182));
#23364=CARTESIAN_POINT('Ctrl Pts',(-0.493843476541492,1.,1.9827665876182));
#23365=CARTESIAN_POINT('Ctrl Pts',(-0.490150627860955,-1.,1.97783973019229));
#23366=CARTESIAN_POINT('Ctrl Pts',(-0.490150627860955,1.,1.97783973019229));
#23367=CARTESIAN_POINT('Ctrl Pts',(-0.486502692907661,-1.,1.97289186263272));
#23368=CARTESIAN_POINT('Ctrl Pts',(-0.486502692907661,1.,1.97289186263272));
#23369=CARTESIAN_POINT('Ctrl Pts',(-0.482901662120687,-1.,1.96792703422358));
#23370=CARTESIAN_POINT('Ctrl Pts',(-0.482901662120687,1.,1.96792703422358));
#23371=CARTESIAN_POINT('Ctrl Pts',(-0.479349583074846,-1.,1.96294933055938));
#23372=CARTESIAN_POINT('Ctrl Pts',(-0.479349583074846,1.,1.96294933055938));
#23373=CARTESIAN_POINT('Ctrl Pts',(-0.475848034683172,-1.,1.95796111148175));
#23374=CARTESIAN_POINT('Ctrl Pts',(-0.475848034683172,1.,1.95796111148175));
#23375=CARTESIAN_POINT('Ctrl Pts',(-0.47239767226408,-1.,1.95296148278136));
#23376=CARTESIAN_POINT('Ctrl Pts',(-0.47239767226408,1.,1.95296148278136));
#23377=CARTESIAN_POINT('Ctrl Pts',(-0.468997482913158,-1.,1.94794381136524));
#23378=CARTESIAN_POINT('Ctrl Pts',(-0.468997482913158,1.,1.94794381136524));
#23379=CARTESIAN_POINT('Ctrl Pts',(-0.465645462026065,-1.,1.94289794196205));
#23380=CARTESIAN_POINT('Ctrl Pts',(-0.465645462026065,1.,1.94289794196205));
#23381=CARTESIAN_POINT('Ctrl Pts',(-0.462340031009087,-1.,1.93781486640834));
#23382=CARTESIAN_POINT('Ctrl Pts',(-0.462340031009087,1.,1.93781486640834));
#23383=CARTESIAN_POINT('Ctrl Pts',(-0.459081234547931,-1.,1.93269066517936));
#23384=CARTESIAN_POINT('Ctrl Pts',(-0.459081234547931,1.,1.93269066517936));
#23385=CARTESIAN_POINT('Ctrl Pts',(-0.455872005174335,-1.,1.92753067150461));
#23386=CARTESIAN_POINT('Ctrl Pts',(-0.455872005174335,1.,1.92753067150461));
#23387=CARTESIAN_POINT('Ctrl Pts',(-0.452719478359356,-1.,1.9223538064847));
#23388=CARTESIAN_POINT('Ctrl Pts',(-0.452719478359356,1.,1.9223538064847));
#23389=CARTESIAN_POINT('Ctrl Pts',(-0.449632260106572,-1.,1.91718342555717));
#23390=CARTESIAN_POINT('Ctrl Pts',(-0.449632260106572,1.,1.91718342555717));
#23391=CARTESIAN_POINT('Ctrl Pts',(-0.446617343485651,-1.,1.91203699981095));
#23392=CARTESIAN_POINT('Ctrl Pts',(-0.446617343485651,1.,1.91203699981095));
#23393=CARTESIAN_POINT('Ctrl Pts',(-0.44367755684917,-1.,1.90691756144906));
#23394=CARTESIAN_POINT('Ctrl Pts',(-0.44367755684917,1.,1.90691756144906));
#23395=CARTESIAN_POINT('Ctrl Pts',(-0.440807833704161,-1.,1.90180124389137));
#23396=CARTESIAN_POINT('Ctrl Pts',(-0.440807833704161,1.,1.90180124389137));
#23397=CARTESIAN_POINT('Ctrl Pts',(-0.437995003948443,-1.,1.89663648956549));
#23398=CARTESIAN_POINT('Ctrl Pts',(-0.437995003948443,1.,1.89663648956549));
#23399=CARTESIAN_POINT('Ctrl Pts',(-0.43522566096358,-1.,1.89136993975585));
#23400=CARTESIAN_POINT('Ctrl Pts',(-0.43522566096358,1.,1.89136993975585));
#23401=CARTESIAN_POINT('Ctrl Pts',(-0.432493038548833,-1.,1.88596913666828));
#23402=CARTESIAN_POINT('Ctrl Pts',(-0.432493038548833,1.,1.88596913666828));
#23403=CARTESIAN_POINT('Ctrl Pts',(-0.429803062482217,-1.,1.88044229001778));
#23404=CARTESIAN_POINT('Ctrl Pts',(-0.429803062482217,1.,1.88044229001778));
#23405=CARTESIAN_POINT('Ctrl Pts',(-0.427183828518743,-1.,1.87486989291333));
#23406=CARTESIAN_POINT('Ctrl Pts',(-0.427183828518743,1.,1.87486989291333));
#23407=CARTESIAN_POINT('Ctrl Pts',(-0.424678177290876,-1.,1.8693780394412));
#23408=CARTESIAN_POINT('Ctrl Pts',(-0.424678177290876,1.,1.8693780394412));
#23409=CARTESIAN_POINT('Ctrl Pts',(-0.422327307417885,-1.,1.86408083333863));
#23410=CARTESIAN_POINT('Ctrl Pts',(-0.422327307417885,1.,1.86408083333863));
#23411=CARTESIAN_POINT('Ctrl Pts',(-0.420157287975583,-1.,1.8590328109667));
#23412=CARTESIAN_POINT('Ctrl Pts',(-0.420157287975583,1.,1.8590328109667));
#23413=CARTESIAN_POINT('Ctrl Pts',(-0.418164129144045,-1.,1.8541763285645));
#23414=CARTESIAN_POINT('Ctrl Pts',(-0.418164129144045,1.,1.8541763285645));
#23415=CARTESIAN_POINT('Ctrl Pts',(-0.416300022039885,-1.,1.84929312930314));
#23416=CARTESIAN_POINT('Ctrl Pts',(-0.416300022039885,1.,1.84929312930314));
#23417=CARTESIAN_POINT('Ctrl Pts',(-0.414487438255542,-1.,1.84405757074218));
#23418=CARTESIAN_POINT('Ctrl Pts',(-0.414487438255542,1.,1.84405757074218));
#23419=CARTESIAN_POINT('Ctrl Pts',(-0.412633125322945,-1.,1.8380895347617));
#23420=CARTESIAN_POINT('Ctrl Pts',(-0.412633125322945,1.,1.8380895347617));
#23421=CARTESIAN_POINT('Ctrl Pts',(-0.410641256301276,-1.,1.83100408895047));
#23422=CARTESIAN_POINT('Ctrl Pts',(-0.410641256301276,1.,1.83100408895047));
#23423=CARTESIAN_POINT('Ctrl Pts',(-0.408428948106227,-1.,1.82247022677562));
#23424=CARTESIAN_POINT('Ctrl Pts',(-0.408428948106227,1.,1.82247022677562));
#23425=CARTESIAN_POINT('Ctrl Pts',(-0.405933518407175,-1.,1.81223801812013));
#23426=CARTESIAN_POINT('Ctrl Pts',(-0.405933518407175,1.,1.81223801812013));
#23427=CARTESIAN_POINT('Ctrl Pts',(-0.403107976163396,-1.,1.80012077173238));
#23428=CARTESIAN_POINT('Ctrl Pts',(-0.403107976163396,1.,1.80012077173238));
#23429=CARTESIAN_POINT('Ctrl Pts',(-0.399919403774155,-1.,1.78598826343754));
#23430=CARTESIAN_POINT('Ctrl Pts',(-0.399919403774155,1.,1.78598826343754));
#23431=CARTESIAN_POINT('Ctrl Pts',(-0.396346196110688,-1.,1.76975560043442));
#23432=CARTESIAN_POINT('Ctrl Pts',(-0.396346196110688,1.,1.76975560043442));
#23433=CARTESIAN_POINT('Ctrl Pts',(-0.392375812285395,-1.,1.75137405310193));
#23434=CARTESIAN_POINT('Ctrl Pts',(-0.392375812285395,1.,1.75137405310193));
#23435=CARTESIAN_POINT('Ctrl Pts',(-0.388877023502615,-1.,1.73493170972829));
#23436=CARTESIAN_POINT('Ctrl Pts',(-0.388877023502615,1.,1.73493170972829));
#23437=CARTESIAN_POINT('Ctrl Pts',(-0.386070790323281,-1.,1.72162022244582));
#23438=CARTESIAN_POINT('Ctrl Pts',(-0.386070790323281,1.,1.72162022244582));
#23439=CARTESIAN_POINT('Ctrl Pts',(-0.384119047314215,-1.,1.71231062891398));
#23440=CARTESIAN_POINT('Ctrl Pts',(-0.384119047314215,1.,1.71231062891398));
#23441=CARTESIAN_POINT('Ctrl Pts',(-0.383122945602004,-1.,1.7075470150345));
#23442=CARTESIAN_POINT('Ctrl Pts',(-0.383122945602004,1.,1.7075470150345));
#23443=CARTESIAN_POINT('',(-0.61342227326009,1.,2.11275013067528));
#23444=CARTESIAN_POINT('Ctrl Pts',(-0.61342227326009,1.,2.11275013067528));
#23445=CARTESIAN_POINT('Ctrl Pts',(-0.61246736556225,1.,2.11187554260142));
#23446=CARTESIAN_POINT('Ctrl Pts',(-0.610560911691113,1.,2.11012443807661));
#23447=CARTESIAN_POINT('Ctrl Pts',(-0.607711315456826,1.,2.10749199615859));
#23448=CARTESIAN_POINT('Ctrl Pts',(-0.603932030738212,1.,2.10397049887709));
#23449=CARTESIAN_POINT('Ctrl Pts',(-0.599241616422144,1.,2.09954930865331));
#23450=CARTESIAN_POINT('Ctrl Pts',(-0.594585006052824,1.,2.09510876220501));
#23451=CARTESIAN_POINT('Ctrl Pts',(-0.589962365403189,1.,2.09064881812053));
#23452=CARTESIAN_POINT('Ctrl Pts',(-0.585373918990895,1.,2.086169437277));
#23453=CARTESIAN_POINT('Ctrl Pts',(-0.580819952107257,1.,2.08167059018138));
#23454=CARTESIAN_POINT('Ctrl Pts',(-0.576300797416275,1.,2.07715226767361));
#23455=CARTESIAN_POINT('Ctrl Pts',(-0.571816823242411,1.,2.07261449292757));
#23456=CARTESIAN_POINT('Ctrl Pts',(-0.567368421181229,1.,2.06805732997383));
#23457=CARTESIAN_POINT('Ctrl Pts',(-0.562955993082574,1.,2.06348090160697));
#23458=CARTESIAN_POINT('Ctrl Pts',(-0.558579940185467,1.,2.05888537756571));
#23459=CARTESIAN_POINT('Ctrl Pts',(-0.55424065746411,1.,2.05427091604482));
#23460=CARTESIAN_POINT('Ctrl Pts',(-0.549938525150342,1.,2.04963761077974));
#23461=CARTESIAN_POINT('Ctrl Pts',(-0.545673903817348,1.,2.0449854471456));
#23462=CARTESIAN_POINT('Ctrl Pts',(-0.54144712061552,1.,2.0403142269048));
#23463=CARTESIAN_POINT('Ctrl Pts',(-0.537258489833134,1.,2.03562362953993));
#23464=CARTESIAN_POINT('Ctrl Pts',(-0.533108355132905,1.,2.03091336214401));
#23465=CARTESIAN_POINT('Ctrl Pts',(-0.528997127241911,1.,2.02618329083289));
#23466=CARTESIAN_POINT('Ctrl Pts',(-0.524925318333518,1.,2.02143356304712));
#23467=CARTESIAN_POINT('Ctrl Pts',(-0.520893590399428,1.,2.01666477917305));
#23468=CARTESIAN_POINT('Ctrl Pts',(-0.516902681728733,1.,2.01187773939257));
#23469=CARTESIAN_POINT('Ctrl Pts',(-0.512953306961814,1.,2.00707309946955));
#23470=CARTESIAN_POINT('Ctrl Pts',(-0.509046069886152,1.,2.00225107134733));
#23471=CARTESIAN_POINT('Ctrl Pts',(-0.505181361323011,1.,1.99741107463567));
#23472=CARTESIAN_POINT('Ctrl Pts',(-0.501359287727129,1.,1.9925514912615));
#23473=CARTESIAN_POINT('Ctrl Pts',(-0.497579909545564,1.,1.98767044752929));
#23474=CARTESIAN_POINT('Ctrl Pts',(-0.493843476541492,1.,1.9827665876182));
#23475=CARTESIAN_POINT('Ctrl Pts',(-0.490150627860955,1.,1.97783973019229));
#23476=CARTESIAN_POINT('Ctrl Pts',(-0.486502692907661,1.,1.97289186263272));
#23477=CARTESIAN_POINT('Ctrl Pts',(-0.482901662120687,1.,1.96792703422358));
#23478=CARTESIAN_POINT('Ctrl Pts',(-0.479349583074846,1.,1.96294933055938));
#23479=CARTESIAN_POINT('Ctrl Pts',(-0.475848034683172,1.,1.95796111148175));
#23480=CARTESIAN_POINT('Ctrl Pts',(-0.47239767226408,1.,1.95296148278136));
#23481=CARTESIAN_POINT('Ctrl Pts',(-0.468997482913158,1.,1.94794381136524));
#23482=CARTESIAN_POINT('Ctrl Pts',(-0.465645462026065,1.,1.94289794196205));
#23483=CARTESIAN_POINT('Ctrl Pts',(-0.462340031009087,1.,1.93781486640834));
#23484=CARTESIAN_POINT('Ctrl Pts',(-0.459081234547931,1.,1.93269066517936));
#23485=CARTESIAN_POINT('Ctrl Pts',(-0.455872005174335,1.,1.92753067150461));
#23486=CARTESIAN_POINT('Ctrl Pts',(-0.452719478359356,1.,1.9223538064847));
#23487=CARTESIAN_POINT('Ctrl Pts',(-0.449632260106572,1.,1.91718342555717));
#23488=CARTESIAN_POINT('Ctrl Pts',(-0.446617343485651,1.,1.91203699981095));
#23489=CARTESIAN_POINT('Ctrl Pts',(-0.44367755684917,1.,1.90691756144906));
#23490=CARTESIAN_POINT('Ctrl Pts',(-0.440807833704161,1.,1.90180124389137));
#23491=CARTESIAN_POINT('Ctrl Pts',(-0.437995003948443,1.,1.89663648956549));
#23492=CARTESIAN_POINT('Ctrl Pts',(-0.43522566096358,1.,1.89136993975585));
#23493=CARTESIAN_POINT('Ctrl Pts',(-0.432493038548833,1.,1.88596913666828));
#23494=CARTESIAN_POINT('Ctrl Pts',(-0.429803062482217,1.,1.88044229001778));
#23495=CARTESIAN_POINT('Ctrl Pts',(-0.427183828518743,1.,1.87486989291333));
#23496=CARTESIAN_POINT('Ctrl Pts',(-0.424678177290876,1.,1.8693780394412));
#23497=CARTESIAN_POINT('Ctrl Pts',(-0.422327307417885,1.,1.86408083333863));
#23498=CARTESIAN_POINT('Ctrl Pts',(-0.420157287975583,1.,1.8590328109667));
#23499=CARTESIAN_POINT('Ctrl Pts',(-0.418164129144045,1.,1.8541763285645));
#23500=CARTESIAN_POINT('Ctrl Pts',(-0.416300022039885,1.,1.84929312930314));
#23501=CARTESIAN_POINT('Ctrl Pts',(-0.414487438255542,1.,1.84405757074218));
#23502=CARTESIAN_POINT('Ctrl Pts',(-0.412633125322945,1.,1.8380895347617));
#23503=CARTESIAN_POINT('Ctrl Pts',(-0.410641256301276,1.,1.83100408895047));
#23504=CARTESIAN_POINT('Ctrl Pts',(-0.408428948106227,1.,1.82247022677562));
#23505=CARTESIAN_POINT('Ctrl Pts',(-0.405933518407175,1.,1.81223801812013));
#23506=CARTESIAN_POINT('Ctrl Pts',(-0.403107976163396,1.,1.80012077173238));
#23507=CARTESIAN_POINT('Ctrl Pts',(-0.399919403774155,1.,1.78598826343754));
#23508=CARTESIAN_POINT('Ctrl Pts',(-0.396346196110688,1.,1.76975560043442));
#23509=CARTESIAN_POINT('Ctrl Pts',(-0.392375812285395,1.,1.75137405310193));
#23510=CARTESIAN_POINT('Ctrl Pts',(-0.388877023502615,1.,1.73493170972829));
#23511=CARTESIAN_POINT('Ctrl Pts',(-0.386070790323281,1.,1.72162022244582));
#23512=CARTESIAN_POINT('Ctrl Pts',(-0.384119047314215,1.,1.71231062891398));
#23513=CARTESIAN_POINT('Ctrl Pts',(-0.383122945602004,1.,1.7075470150345));
#23514=CARTESIAN_POINT('',(-0.61342227326009,0.,2.11275013067528));
#23515=CARTESIAN_POINT('Origin',(-0.745574324794401,0.,2.0698113262342));
#23516=CARTESIAN_POINT('',(-0.745574324794401,1.,2.0698113262342));
#23517=CARTESIAN_POINT('',(-0.61342227326009,1.,2.11275013067528));
#23518=CARTESIAN_POINT('',(-0.745574324794401,0.,2.0698113262342));
#23519=CARTESIAN_POINT('Ctrl Pts',(-0.693717979106306,-1.,1.60662857109684));
#23520=CARTESIAN_POINT('Ctrl Pts',(-0.693717979106306,1.,1.60662857109684));
#23521=CARTESIAN_POINT('Ctrl Pts',(-0.695712097881194,-1.,1.61106790958151));
#23522=CARTESIAN_POINT('Ctrl Pts',(-0.695712097881194,1.,1.61106790958151));
#23523=CARTESIAN_POINT('Ctrl Pts',(-0.699605146405088,-1.,1.61974673472612));
#23524=CARTESIAN_POINT('Ctrl Pts',(-0.699605146405088,1.,1.61974673472612));
#23525=CARTESIAN_POINT('Ctrl Pts',(-0.705159151988319,-1.,1.63216541664676));
#23526=CARTESIAN_POINT('Ctrl Pts',(-0.705159151988319,1.,1.63216541664676));
#23527=CARTESIAN_POINT('Ctrl Pts',(-0.711993139355394,-1.,1.64752408832016));
#23528=CARTESIAN_POINT('Ctrl Pts',(-0.711993139355394,1.,1.64752408832016));
#23529=CARTESIAN_POINT('Ctrl Pts',(-0.719585433804282,-1.,1.6647288055568));
#23530=CARTESIAN_POINT('Ctrl Pts',(-0.719585433804282,1.,1.6647288055568));
#23531=CARTESIAN_POINT('Ctrl Pts',(-0.726235967997433,-1.,1.67996158455503));
#23532=CARTESIAN_POINT('Ctrl Pts',(-0.726235967997433,1.,1.67996158455503));
#23533=CARTESIAN_POINT('Ctrl Pts',(-0.731963238697195,-1.,1.69326921975743));
#23534=CARTESIAN_POINT('Ctrl Pts',(-0.731963238697195,1.,1.69326921975743));
#23535=CARTESIAN_POINT('Ctrl Pts',(-0.736799665724771,-1.,1.70473309006121));
#23536=CARTESIAN_POINT('Ctrl Pts',(-0.736799665724771,1.,1.70473309006121));
#23537=CARTESIAN_POINT('Ctrl Pts',(-0.740795162032088,-1.,1.71447789751927));
#23538=CARTESIAN_POINT('Ctrl Pts',(-0.740795162032088,1.,1.71447789751927));
#23539=CARTESIAN_POINT('Ctrl Pts',(-0.744021445433764,-1.,1.7226822991693));
#23540=CARTESIAN_POINT('Ctrl Pts',(-0.744021445433764,1.,1.7226822991693));
#23541=CARTESIAN_POINT('Ctrl Pts',(-0.746574710096436,-1.,1.72958533647399));
#23542=CARTESIAN_POINT('Ctrl Pts',(-0.746574710096436,1.,1.72958533647399));
#23543=CARTESIAN_POINT('Ctrl Pts',(-0.748582462954855,-1.,1.73550351679848));
#23544=CARTESIAN_POINT('Ctrl Pts',(-0.748582462954855,1.,1.73550351679848));
#23545=CARTESIAN_POINT('Ctrl Pts',(-0.75019343597954,-1.,1.74080458266705));
#23546=CARTESIAN_POINT('Ctrl Pts',(-0.75019343597954,1.,1.74080458266705));
#23547=CARTESIAN_POINT('Ctrl Pts',(-0.751555614163629,-1.,1.74585086852298));
#23548=CARTESIAN_POINT('Ctrl Pts',(-0.751555614163629,1.,1.74585086852298));
#23549=CARTESIAN_POINT('Ctrl Pts',(-0.752797683531377,-1.,1.75095139468809));
#23550=CARTESIAN_POINT('Ctrl Pts',(-0.752797683531377,1.,1.75095139468809));
#23551=CARTESIAN_POINT('Ctrl Pts',(-0.75400925402848,-1.,1.75631083600175));
#23552=CARTESIAN_POINT('Ctrl Pts',(-0.75400925402848,1.,1.75631083600175));
#23553=CARTESIAN_POINT('Ctrl Pts',(-0.755220979975262,-1.,1.7619781724032));
#23554=CARTESIAN_POINT('Ctrl Pts',(-0.755220979975262,1.,1.7619781724032));
#23555=CARTESIAN_POINT('Ctrl Pts',(-0.756421896028403,-1.,1.76789396003141));
#23556=CARTESIAN_POINT('Ctrl Pts',(-0.756421896028403,1.,1.76789396003141));
#23557=CARTESIAN_POINT('Ctrl Pts',(-0.757578264077238,-1.,1.77394167108342));
#23558=CARTESIAN_POINT('Ctrl Pts',(-0.757578264077238,1.,1.77394167108342));
#23559=CARTESIAN_POINT('Ctrl Pts',(-0.75865062667738,-1.,1.77999411220912));
#23560=CARTESIAN_POINT('Ctrl Pts',(-0.75865062667738,1.,1.77999411220912));
#23561=CARTESIAN_POINT('Ctrl Pts',(-0.759614401109868,-1.,1.78596964884526));
#23562=CARTESIAN_POINT('Ctrl Pts',(-0.759614401109868,1.,1.78596964884526));
#23563=CARTESIAN_POINT('Ctrl Pts',(-0.760469555880425,-1.,1.79185815610802));
#23564=CARTESIAN_POINT('Ctrl Pts',(-0.760469555880425,1.,1.79185815610802));
#23565=CARTESIAN_POINT('Ctrl Pts',(-0.761229695230359,-1.,1.79768986997735));
#23566=CARTESIAN_POINT('Ctrl Pts',(-0.761229695230359,1.,1.79768986997735));
#23567=CARTESIAN_POINT('Ctrl Pts',(-0.761915336443516,-1.,1.80351583877334));
#23568=CARTESIAN_POINT('Ctrl Pts',(-0.761915336443516,1.,1.80351583877334));
#23569=CARTESIAN_POINT('Ctrl Pts',(-0.762546129464036,-1.,1.80938551463989));
#23570=CARTESIAN_POINT('Ctrl Pts',(-0.762546129464036,1.,1.80938551463989));
#23571=CARTESIAN_POINT('Ctrl Pts',(-0.763132003836783,-1.,1.81532118405566));
#23572=CARTESIAN_POINT('Ctrl Pts',(-0.763132003836783,1.,1.81532118405566));
#23573=CARTESIAN_POINT('Ctrl Pts',(-0.763673465462854,-1.,1.82131873145297));
#23574=CARTESIAN_POINT('Ctrl Pts',(-0.763673465462854,1.,1.82131873145297));
#23575=CARTESIAN_POINT('Ctrl Pts',(-0.764165902606055,-1.,1.8273599120008));
#23576=CARTESIAN_POINT('Ctrl Pts',(-0.764165902606055,1.,1.8273599120008));
#23577=CARTESIAN_POINT('Ctrl Pts',(-0.764602549687845,-1.,1.8334207722714));
#23578=CARTESIAN_POINT('Ctrl Pts',(-0.764602549687845,1.,1.8334207722714));
#23579=CARTESIAN_POINT('Ctrl Pts',(-0.764978057881687,-1.,1.83948181064823));
#23580=CARTESIAN_POINT('Ctrl Pts',(-0.764978057881687,1.,1.83948181064823));
#23581=CARTESIAN_POINT('Ctrl Pts',(-0.765291664861971,-1.,1.8455369887591));
#23582=CARTESIAN_POINT('Ctrl Pts',(-0.765291664861971,1.,1.8455369887591));
#23583=CARTESIAN_POINT('Ctrl Pts',(-0.765545710619023,-1.,1.85158945130054));
#23584=CARTESIAN_POINT('Ctrl Pts',(-0.765545710619023,1.,1.85158945130054));
#23585=CARTESIAN_POINT('Ctrl Pts',(-0.765744212909305,-1.,1.85764741390391));
#23586=CARTESIAN_POINT('Ctrl Pts',(-0.765744212909305,1.,1.85764741390391));
#23587=CARTESIAN_POINT('Ctrl Pts',(-0.765891519092557,-1.,1.86372027063314));
#23588=CARTESIAN_POINT('Ctrl Pts',(-0.765891519092557,1.,1.86372027063314));
#23589=CARTESIAN_POINT('Ctrl Pts',(-0.765990708546111,-1.,1.86981398314345));
#23590=CARTESIAN_POINT('Ctrl Pts',(-0.765990708546111,1.,1.86981398314345));
#23591=CARTESIAN_POINT('Ctrl Pts',(-0.766042837036759,-1.,1.87592888967886));
#23592=CARTESIAN_POINT('Ctrl Pts',(-0.766042837036759,1.,1.87592888967886));
#23593=CARTESIAN_POINT('Ctrl Pts',(-0.766047794851869,-1.,1.88206215302561));
#23594=CARTESIAN_POINT('Ctrl Pts',(-0.766047794851869,1.,1.88206215302561));
#23595=CARTESIAN_POINT('Ctrl Pts',(-0.76600483706209,-1.,1.88820926433409));
#23596=CARTESIAN_POINT('Ctrl Pts',(-0.76600483706209,1.,1.88820926433409));
#23597=CARTESIAN_POINT('Ctrl Pts',(-0.765913193856979,-1.,1.89436577771389));
#23598=CARTESIAN_POINT('Ctrl Pts',(-0.765913193856979,1.,1.89436577771389));
#23599=CARTESIAN_POINT('Ctrl Pts',(-0.765772772593395,-1.,1.90052930393599));
#23600=CARTESIAN_POINT('Ctrl Pts',(-0.765772772593395,1.,1.90052930393599));
#23601=CARTESIAN_POINT('Ctrl Pts',(-0.765584196937936,-1.,1.90669961402362));
#23602=CARTESIAN_POINT('Ctrl Pts',(-0.765584196937936,1.,1.90669961402362));
#23603=CARTESIAN_POINT('Ctrl Pts',(-0.765348465884739,-1.,1.91287765805174));
#23604=CARTESIAN_POINT('Ctrl Pts',(-0.765348465884739,1.,1.91287765805174));
#23605=CARTESIAN_POINT('Ctrl Pts',(-0.765066729667095,-1.,1.91906491634197));
#23606=CARTESIAN_POINT('Ctrl Pts',(-0.765066729667095,1.,1.91906491634197));
#23607=CARTESIAN_POINT('Ctrl Pts',(-0.764740025488189,-1.,1.92526263537041));
#23608=CARTESIAN_POINT('Ctrl Pts',(-0.764740025488189,1.,1.92526263537041));
#23609=CARTESIAN_POINT('Ctrl Pts',(-0.764369010673889,-1.,1.93147105496367));
#23610=CARTESIAN_POINT('Ctrl Pts',(-0.764369010673889,1.,1.93147105496367));
#23611=CARTESIAN_POINT('Ctrl Pts',(-0.763954049121393,-1.,1.93768964875867));
#23612=CARTESIAN_POINT('Ctrl Pts',(-0.763954049121393,1.,1.93768964875867));
#23613=CARTESIAN_POINT('Ctrl Pts',(-0.76349533353858,-1.,1.94391746617626));
#23614=CARTESIAN_POINT('Ctrl Pts',(-0.76349533353858,1.,1.94391746617626));
#23615=CARTESIAN_POINT('Ctrl Pts',(-0.762992990878774,-1.,1.95015342590025));
#23616=CARTESIAN_POINT('Ctrl Pts',(-0.762992990878774,1.,1.95015342590025));
#23617=CARTESIAN_POINT('Ctrl Pts',(-0.762447203806263,-1.,1.95639665309893));
#23618=CARTESIAN_POINT('Ctrl Pts',(-0.762447203806263,1.,1.95639665309893));
#23619=CARTESIAN_POINT('Ctrl Pts',(-0.761858300014575,-1.,1.96264672744229));
#23620=CARTESIAN_POINT('Ctrl Pts',(-0.761858300014575,1.,1.96264672744229));
#23621=CARTESIAN_POINT('Ctrl Pts',(-0.761226690483986,-1.,1.96890351582545));
#23622=CARTESIAN_POINT('Ctrl Pts',(-0.761226690483986,1.,1.96890351582545));
#23623=CARTESIAN_POINT('Ctrl Pts',(-0.760552825409855,-1.,1.97516705321521));
#23624=CARTESIAN_POINT('Ctrl Pts',(-0.760552825409855,1.,1.97516705321521));
#23625=CARTESIAN_POINT('Ctrl Pts',(-0.759837147452135,-1.,1.98143741418156));
#23626=CARTESIAN_POINT('Ctrl Pts',(-0.759837147452135,1.,1.98143741418156));
#23627=CARTESIAN_POINT('Ctrl Pts',(-0.759080037802243,-1.,1.98771456680806));
#23628=CARTESIAN_POINT('Ctrl Pts',(-0.759080037802243,1.,1.98771456680806));
#23629=CARTESIAN_POINT('Ctrl Pts',(-0.758281796766377,-1.,1.9939983109871));
#23630=CARTESIAN_POINT('Ctrl Pts',(-0.758281796766377,1.,1.9939983109871));
#23631=CARTESIAN_POINT('Ctrl Pts',(-0.757442676862341,-1.,2.00028834739072));
#23632=CARTESIAN_POINT('Ctrl Pts',(-0.757442676862341,1.,2.00028834739072));
#23633=CARTESIAN_POINT('Ctrl Pts',(-0.756562904646496,-1.,2.00658431587682));
#23634=CARTESIAN_POINT('Ctrl Pts',(-0.756562904646496,1.,2.00658431587682));
#23635=CARTESIAN_POINT('Ctrl Pts',(-0.7556427049581,-1.,2.01288584328149));
#23636=CARTESIAN_POINT('Ctrl Pts',(-0.7556427049581,1.,2.01288584328149));
#23637=CARTESIAN_POINT('Ctrl Pts',(-0.75468233072352,-1.,2.01919259406003));
#23638=CARTESIAN_POINT('Ctrl Pts',(-0.75468233072352,1.,2.01919259406003));
#23639=CARTESIAN_POINT('Ctrl Pts',(-0.753682061113766,-1.,2.02550428623587));
#23640=CARTESIAN_POINT('Ctrl Pts',(-0.753682061113766,1.,2.02550428623587));
#23641=CARTESIAN_POINT('Ctrl Pts',(-0.752642180488104,-1.,2.03182068456467));
#23642=CARTESIAN_POINT('Ctrl Pts',(-0.752642180488104,1.,2.03182068456467));
#23643=CARTESIAN_POINT('Ctrl Pts',(-0.751562963361384,-1.,2.03814160092173));
#23644=CARTESIAN_POINT('Ctrl Pts',(-0.751562963361384,1.,2.03814160092173));
#23645=CARTESIAN_POINT('Ctrl Pts',(-0.750444657874758,-1.,2.04446689147754));
#23646=CARTESIAN_POINT('Ctrl Pts',(-0.750444657874758,1.,2.04446689147754));
#23647=CARTESIAN_POINT('Ctrl Pts',(-0.749287468663053,-1.,2.05079645591606));
#23648=CARTESIAN_POINT('Ctrl Pts',(-0.749287468663053,1.,2.05079645591606));
#23649=CARTESIAN_POINT('Ctrl Pts',(-0.748091554181101,-1.,2.05713023030263));
#23650=CARTESIAN_POINT('Ctrl Pts',(-0.748091554181101,1.,2.05713023030263));
#23651=CARTESIAN_POINT('Ctrl Pts',(-0.747103932785504,-1.,2.06220058927162));
#23652=CARTESIAN_POINT('Ctrl Pts',(-0.747103932785504,1.,2.06220058927162));
#23653=CARTESIAN_POINT('Ctrl Pts',(-0.746345871542696,-1.,2.06600523016401));
#23654=CARTESIAN_POINT('Ctrl Pts',(-0.746345871542696,1.,2.06600523016401));
#23655=CARTESIAN_POINT('Ctrl Pts',(-0.74583279137781,-1.,2.06854248895575));
#23656=CARTESIAN_POINT('Ctrl Pts',(-0.74583279137781,1.,2.06854248895575));
#23657=CARTESIAN_POINT('Ctrl Pts',(-0.745574324794401,-1.,2.0698113262342));
#23658=CARTESIAN_POINT('Ctrl Pts',(-0.745574324794401,1.,2.0698113262342));
#23659=CARTESIAN_POINT('',(-0.693717979106306,1.,1.60662857109684));
#23660=CARTESIAN_POINT('Ctrl Pts',(-0.693717979106306,1.,1.60662857109684));
#23661=CARTESIAN_POINT('Ctrl Pts',(-0.695712097881194,1.,1.61106790958151));
#23662=CARTESIAN_POINT('Ctrl Pts',(-0.699605146405088,1.,1.61974673472612));
#23663=CARTESIAN_POINT('Ctrl Pts',(-0.705159151988319,1.,1.63216541664676));
#23664=CARTESIAN_POINT('Ctrl Pts',(-0.711993139355394,1.,1.64752408832016));
#23665=CARTESIAN_POINT('Ctrl Pts',(-0.719585433804282,1.,1.6647288055568));
#23666=CARTESIAN_POINT('Ctrl Pts',(-0.726235967997433,1.,1.67996158455503));
#23667=CARTESIAN_POINT('Ctrl Pts',(-0.731963238697195,1.,1.69326921975743));
#23668=CARTESIAN_POINT('Ctrl Pts',(-0.736799665724771,1.,1.70473309006121));
#23669=CARTESIAN_POINT('Ctrl Pts',(-0.740795162032088,1.,1.71447789751927));
#23670=CARTESIAN_POINT('Ctrl Pts',(-0.744021445433764,1.,1.7226822991693));
#23671=CARTESIAN_POINT('Ctrl Pts',(-0.746574710096436,1.,1.72958533647399));
#23672=CARTESIAN_POINT('Ctrl Pts',(-0.748582462954855,1.,1.73550351679848));
#23673=CARTESIAN_POINT('Ctrl Pts',(-0.75019343597954,1.,1.74080458266705));
#23674=CARTESIAN_POINT('Ctrl Pts',(-0.751555614163629,1.,1.74585086852298));
#23675=CARTESIAN_POINT('Ctrl Pts',(-0.752797683531377,1.,1.75095139468809));
#23676=CARTESIAN_POINT('Ctrl Pts',(-0.75400925402848,1.,1.75631083600175));
#23677=CARTESIAN_POINT('Ctrl Pts',(-0.755220979975262,1.,1.7619781724032));
#23678=CARTESIAN_POINT('Ctrl Pts',(-0.756421896028403,1.,1.76789396003141));
#23679=CARTESIAN_POINT('Ctrl Pts',(-0.757578264077238,1.,1.77394167108342));
#23680=CARTESIAN_POINT('Ctrl Pts',(-0.75865062667738,1.,1.77999411220912));
#23681=CARTESIAN_POINT('Ctrl Pts',(-0.759614401109868,1.,1.78596964884526));
#23682=CARTESIAN_POINT('Ctrl Pts',(-0.760469555880425,1.,1.79185815610802));
#23683=CARTESIAN_POINT('Ctrl Pts',(-0.761229695230359,1.,1.79768986997735));
#23684=CARTESIAN_POINT('Ctrl Pts',(-0.761915336443516,1.,1.80351583877334));
#23685=CARTESIAN_POINT('Ctrl Pts',(-0.762546129464036,1.,1.80938551463989));
#23686=CARTESIAN_POINT('Ctrl Pts',(-0.763132003836783,1.,1.81532118405566));
#23687=CARTESIAN_POINT('Ctrl Pts',(-0.763673465462854,1.,1.82131873145297));
#23688=CARTESIAN_POINT('Ctrl Pts',(-0.764165902606055,1.,1.8273599120008));
#23689=CARTESIAN_POINT('Ctrl Pts',(-0.764602549687845,1.,1.8334207722714));
#23690=CARTESIAN_POINT('Ctrl Pts',(-0.764978057881687,1.,1.83948181064823));
#23691=CARTESIAN_POINT('Ctrl Pts',(-0.765291664861971,1.,1.8455369887591));
#23692=CARTESIAN_POINT('Ctrl Pts',(-0.765545710619023,1.,1.85158945130054));
#23693=CARTESIAN_POINT('Ctrl Pts',(-0.765744212909305,1.,1.85764741390391));
#23694=CARTESIAN_POINT('Ctrl Pts',(-0.765891519092557,1.,1.86372027063314));
#23695=CARTESIAN_POINT('Ctrl Pts',(-0.765990708546111,1.,1.86981398314345));
#23696=CARTESIAN_POINT('Ctrl Pts',(-0.766042837036759,1.,1.87592888967886));
#23697=CARTESIAN_POINT('Ctrl Pts',(-0.766047794851869,1.,1.88206215302561));
#23698=CARTESIAN_POINT('Ctrl Pts',(-0.76600483706209,1.,1.88820926433409));
#23699=CARTESIAN_POINT('Ctrl Pts',(-0.765913193856979,1.,1.89436577771389));
#23700=CARTESIAN_POINT('Ctrl Pts',(-0.765772772593395,1.,1.90052930393599));
#23701=CARTESIAN_POINT('Ctrl Pts',(-0.765584196937936,1.,1.90669961402362));
#23702=CARTESIAN_POINT('Ctrl Pts',(-0.765348465884739,1.,1.91287765805174));
#23703=CARTESIAN_POINT('Ctrl Pts',(-0.765066729667095,1.,1.91906491634197));
#23704=CARTESIAN_POINT('Ctrl Pts',(-0.764740025488189,1.,1.92526263537041));
#23705=CARTESIAN_POINT('Ctrl Pts',(-0.764369010673889,1.,1.93147105496367));
#23706=CARTESIAN_POINT('Ctrl Pts',(-0.763954049121393,1.,1.93768964875867));
#23707=CARTESIAN_POINT('Ctrl Pts',(-0.76349533353858,1.,1.94391746617626));
#23708=CARTESIAN_POINT('Ctrl Pts',(-0.762992990878774,1.,1.95015342590025));
#23709=CARTESIAN_POINT('Ctrl Pts',(-0.762447203806263,1.,1.95639665309893));
#23710=CARTESIAN_POINT('Ctrl Pts',(-0.761858300014575,1.,1.96264672744229));
#23711=CARTESIAN_POINT('Ctrl Pts',(-0.761226690483986,1.,1.96890351582545));
#23712=CARTESIAN_POINT('Ctrl Pts',(-0.760552825409855,1.,1.97516705321521));
#23713=CARTESIAN_POINT('Ctrl Pts',(-0.759837147452135,1.,1.98143741418156));
#23714=CARTESIAN_POINT('Ctrl Pts',(-0.759080037802243,1.,1.98771456680806));
#23715=CARTESIAN_POINT('Ctrl Pts',(-0.758281796766377,1.,1.9939983109871));
#23716=CARTESIAN_POINT('Ctrl Pts',(-0.757442676862341,1.,2.00028834739072));
#23717=CARTESIAN_POINT('Ctrl Pts',(-0.756562904646496,1.,2.00658431587682));
#23718=CARTESIAN_POINT('Ctrl Pts',(-0.7556427049581,1.,2.01288584328149));
#23719=CARTESIAN_POINT('Ctrl Pts',(-0.75468233072352,1.,2.01919259406003));
#23720=CARTESIAN_POINT('Ctrl Pts',(-0.753682061113766,1.,2.02550428623587));
#23721=CARTESIAN_POINT('Ctrl Pts',(-0.752642180488104,1.,2.03182068456467));
#23722=CARTESIAN_POINT('Ctrl Pts',(-0.751562963361384,1.,2.03814160092173));
#23723=CARTESIAN_POINT('Ctrl Pts',(-0.750444657874758,1.,2.04446689147754));
#23724=CARTESIAN_POINT('Ctrl Pts',(-0.749287468663053,1.,2.05079645591606));
#23725=CARTESIAN_POINT('Ctrl Pts',(-0.748091554181101,1.,2.05713023030263));
#23726=CARTESIAN_POINT('Ctrl Pts',(-0.747103932785504,1.,2.06220058927162));
#23727=CARTESIAN_POINT('Ctrl Pts',(-0.746345871542696,1.,2.06600523016401));
#23728=CARTESIAN_POINT('Ctrl Pts',(-0.74583279137781,1.,2.06854248895575));
#23729=CARTESIAN_POINT('Ctrl Pts',(-0.745574324794401,1.,2.0698113262342));
#23730=CARTESIAN_POINT('',(-0.693717979106306,0.,1.60662857109684));
#23731=CARTESIAN_POINT('Origin',(0.,0.,0.));
#23732=CARTESIAN_POINT('',(-0.892032620296855,1.,1.5055822144029));
#23733=CARTESIAN_POINT('Origin',(0.,1.,0.));
#23734=CARTESIAN_POINT('',(-0.892032620296855,0.,1.5055822144029));
#23735=CARTESIAN_POINT('Ctrl Pts',(-1.23627494547115,-1.,1.81978687191668));
#23736=CARTESIAN_POINT('Ctrl Pts',(-1.23627494547115,1.,1.81978687191668));
#23737=CARTESIAN_POINT('Ctrl Pts',(-1.23509651170476,-1.,1.81925017193666));
#23738=CARTESIAN_POINT('Ctrl Pts',(-1.23509651170476,1.,1.81925017193666));
#23739=CARTESIAN_POINT('Ctrl Pts',(-1.2327422452705,-1.,1.81817389921279));
#23740=CARTESIAN_POINT('Ctrl Pts',(-1.2327422452705,1.,1.81817389921279));
#23741=CARTESIAN_POINT('Ctrl Pts',(-1.2292186489137,-1.,1.8165508718364));
#23742=CARTESIAN_POINT('Ctrl Pts',(-1.2292186489137,1.,1.8165508718364));
#23743=CARTESIAN_POINT('Ctrl Pts',(-1.2245361330495,-1.,1.81436959210434));
#23744=CARTESIAN_POINT('Ctrl Pts',(-1.2245361330495,1.,1.81436959210434));
#23745=CARTESIAN_POINT('Ctrl Pts',(-1.21870906103557,-1.,1.81161420806656));
#23746=CARTESIAN_POINT('Ctrl Pts',(-1.21870906103557,1.,1.81161420806656));
#23747=CARTESIAN_POINT('Ctrl Pts',(-1.21290815708314,-1.,1.80882996917129));
#23748=CARTESIAN_POINT('Ctrl Pts',(-1.21290815708314,1.,1.80882996917129));
#23749=CARTESIAN_POINT('Ctrl Pts',(-1.20713356605475,-1.,1.80601678480707));
#23750=CARTESIAN_POINT('Ctrl Pts',(-1.20713356605475,1.,1.80601678480707));
#23751=CARTESIAN_POINT('Ctrl Pts',(-1.20138548938974,-1.,1.80317454838603));
#23752=CARTESIAN_POINT('Ctrl Pts',(-1.20138548938974,1.,1.80317454838603));
#23753=CARTESIAN_POINT('Ctrl Pts',(-1.19566418930242,-1.,1.80030314369879));
#23754=CARTESIAN_POINT('Ctrl Pts',(-1.19566418930242,1.,1.80030314369879));
#23755=CARTESIAN_POINT('Ctrl Pts',(-1.18996997934445,-1.,1.79740245923478));
#23756=CARTESIAN_POINT('Ctrl Pts',(-1.18996997934445,1.,1.79740245923478));
#23757=CARTESIAN_POINT('Ctrl Pts',(-1.18430321697432,-1.,1.79447240321515));
#23758=CARTESIAN_POINT('Ctrl Pts',(-1.18430321697432,1.,1.79447240321515));
#23759=CARTESIAN_POINT('Ctrl Pts',(-1.17866429440809,-1.,1.79151291552689));
#23760=CARTESIAN_POINT('Ctrl Pts',(-1.17866429440809,1.,1.79151291552689));
#23761=CARTESIAN_POINT('Ctrl Pts',(-1.17305363177328,-1.,1.78852398877616));
#23762=CARTESIAN_POINT('Ctrl Pts',(-1.17305363177328,1.,1.78852398877616));
#23763=CARTESIAN_POINT('Ctrl Pts',(-1.16747166312303,-1.,1.78550566040443));
#23764=CARTESIAN_POINT('Ctrl Pts',(-1.16747166312303,1.,1.78550566040443));
#23765=CARTESIAN_POINT('Ctrl Pts',(-1.16191881298499,-1.,1.78245795881009));
#23766=CARTESIAN_POINT('Ctrl Pts',(-1.16191881298499,1.,1.78245795881009));
#23767=CARTESIAN_POINT('Ctrl Pts',(-1.15639547194698,-1.,1.77938085564275));
#23768=CARTESIAN_POINT('Ctrl Pts',(-1.15639547194698,1.,1.77938085564275));
#23769=CARTESIAN_POINT('Ctrl Pts',(-1.15090197841515,-1.,1.7762742255701));
#23770=CARTESIAN_POINT('Ctrl Pts',(-1.15090197841515,1.,1.7762742255701));
#23771=CARTESIAN_POINT('Ctrl Pts',(-1.1454385822692,-1.,1.77313777896194));
#23772=CARTESIAN_POINT('Ctrl Pts',(-1.1454385822692,1.,1.77313777896194));
#23773=CARTESIAN_POINT('Ctrl Pts',(-1.14000548336975,-1.,1.76997111386769));
#23774=CARTESIAN_POINT('Ctrl Pts',(-1.14000548336975,1.,1.76997111386769));
#23775=CARTESIAN_POINT('Ctrl Pts',(-1.1346029180462,-1.,1.76677384551862));
#23776=CARTESIAN_POINT('Ctrl Pts',(-1.1346029180462,1.,1.76677384551862));
#23777=CARTESIAN_POINT('Ctrl Pts',(-1.12923123555075,-1.,1.7635457196617));
#23778=CARTESIAN_POINT('Ctrl Pts',(-1.12923123555075,1.,1.7635457196617));
#23779=CARTESIAN_POINT('Ctrl Pts',(-1.12389096855086,-1.,1.76028671825096));
#23780=CARTESIAN_POINT('Ctrl Pts',(-1.12389096855086,1.,1.76028671825096));
#23781=CARTESIAN_POINT('Ctrl Pts',(-1.11858293216763,-1.,1.75699720772105));
#23782=CARTESIAN_POINT('Ctrl Pts',(-1.11858293216763,1.,1.75699720772105));
#23783=CARTESIAN_POINT('Ctrl Pts',(-1.11330807582551,-1.,1.7536777209463));
#23784=CARTESIAN_POINT('Ctrl Pts',(-1.11330807582551,1.,1.7536777209463));
#23785=CARTESIAN_POINT('Ctrl Pts',(-1.10806728183007,-1.,1.7503286607592));
#23786=CARTESIAN_POINT('Ctrl Pts',(-1.10806728183007,1.,1.7503286607592));
#23787=CARTESIAN_POINT('Ctrl Pts',(-1.10286118991143,-1.,1.74695004214923));
#23788=CARTESIAN_POINT('Ctrl Pts',(-1.10286118991143,1.,1.74695004214923));
#23789=CARTESIAN_POINT('Ctrl Pts',(-1.09768999241225,-1.,1.74354119236208));
#23790=CARTESIAN_POINT('Ctrl Pts',(-1.09768999241225,1.,1.74354119236208));
#23791=CARTESIAN_POINT('Ctrl Pts',(-1.09255329056493,-1.,1.74010053962247));
#23792=CARTESIAN_POINT('Ctrl Pts',(-1.09255329056493,1.,1.74010053962247));
#23793=CARTESIAN_POINT('Ctrl Pts',(-1.08745056285427,-1.,1.73662628326091));
#23794=CARTESIAN_POINT('Ctrl Pts',(-1.08745056285427,1.,1.73662628326091));
#23795=CARTESIAN_POINT('Ctrl Pts',(-1.08238162784749,-1.,1.73311705663407));
#23796=CARTESIAN_POINT('Ctrl Pts',(-1.08238162784749,1.,1.73311705663407));
#23797=CARTESIAN_POINT('Ctrl Pts',(-1.0773470373727,-1.,1.72957248977424));
#23798=CARTESIAN_POINT('Ctrl Pts',(-1.0773470373727,1.,1.72957248977424));
#23799=CARTESIAN_POINT('Ctrl Pts',(-1.07234866990252,-1.,1.72599406198488));
#23800=CARTESIAN_POINT('Ctrl Pts',(-1.07234866990252,1.,1.72599406198488));
#23801=CARTESIAN_POINT('Ctrl Pts',(-1.06738966975462,-1.,1.72238500928453));
#23802=CARTESIAN_POINT('Ctrl Pts',(-1.06738966975462,1.,1.72238500928453));
#23803=CARTESIAN_POINT('Ctrl Pts',(-1.06247324680647,-1.,1.71874858456904));
#23804=CARTESIAN_POINT('Ctrl Pts',(-1.06247324680647,1.,1.71874858456904));
#23805=CARTESIAN_POINT('Ctrl Pts',(-1.05760163192479,-1.,1.7150865442702));
#23806=CARTESIAN_POINT('Ctrl Pts',(-1.05760163192479,1.,1.7150865442702));
#23807=CARTESIAN_POINT('Ctrl Pts',(-1.05277517202855,-1.,1.71139783543989));
#23808=CARTESIAN_POINT('Ctrl Pts',(-1.05277517202855,1.,1.71139783543989));
#23809=CARTESIAN_POINT('Ctrl Pts',(-1.04799085404995,-1.,1.70767646263649));
#23810=CARTESIAN_POINT('Ctrl Pts',(-1.04799085404995,1.,1.70767646263649));
#23811=CARTESIAN_POINT('Ctrl Pts',(-1.04324363334554,-1.,1.70391338707982));
#23812=CARTESIAN_POINT('Ctrl Pts',(-1.04324363334554,1.,1.70391338707982));
#23813=CARTESIAN_POINT('Ctrl Pts',(-1.03852922490789,-1.,1.70010052930962));
#23814=CARTESIAN_POINT('Ctrl Pts',(-1.03852922490789,1.,1.70010052930962));
#23815=CARTESIAN_POINT('Ctrl Pts',(-1.03384646003588,-1.,1.69623414782771));
#23816=CARTESIAN_POINT('Ctrl Pts',(-1.03384646003588,1.,1.69623414782771));
#23817=CARTESIAN_POINT('Ctrl Pts',(-1.02919977579147,-1.,1.69231840863458));
#23818=CARTESIAN_POINT('Ctrl Pts',(-1.02919977579147,1.,1.69231840863458));
#23819=CARTESIAN_POINT('Ctrl Pts',(-1.02460180535255,-1.,1.68836910178447));
#23820=CARTESIAN_POINT('Ctrl Pts',(-1.02460180535255,1.,1.68836910178447));
#23821=CARTESIAN_POINT('Ctrl Pts',(-1.02006795074201,-1.,1.68440578021706));
#23822=CARTESIAN_POINT('Ctrl Pts',(-1.02006795074201,1.,1.68440578021706));
#23823=CARTESIAN_POINT('Ctrl Pts',(-1.01561026162773,-1.,1.68044289894798));
#23824=CARTESIAN_POINT('Ctrl Pts',(-1.01561026162773,1.,1.68044289894798));
#23825=CARTESIAN_POINT('Ctrl Pts',(-1.01123236493511,-1.,1.67648246776464));
#23826=CARTESIAN_POINT('Ctrl Pts',(-1.01123236493511,1.,1.67648246776464));
#23827=CARTESIAN_POINT('Ctrl Pts',(-1.00692206696414,-1.,1.67250335383293));
#23828=CARTESIAN_POINT('Ctrl Pts',(-1.00692206696414,1.,1.67250335383293));
#23829=CARTESIAN_POINT('Ctrl Pts',(-1.00265091003727,-1.,1.66846059277303));
#23830=CARTESIAN_POINT('Ctrl Pts',(-1.00265091003727,1.,1.66846059277303));
#23831=CARTESIAN_POINT('Ctrl Pts',(-0.998389654952758,-1.,1.66430758030376));
#23832=CARTESIAN_POINT('Ctrl Pts',(-0.998389654952758,1.,1.66430758030376));
#23833=CARTESIAN_POINT('Ctrl Pts',(-0.994121836661306,-1.,1.66001553809947));
#23834=CARTESIAN_POINT('Ctrl Pts',(-0.994121836661306,1.,1.66001553809947));
#23835=CARTESIAN_POINT('Ctrl Pts',(-0.989855627854165,-1.,1.65559044289699));
#23836=CARTESIAN_POINT('Ctrl Pts',(-0.989855627854165,1.,1.65559044289699));
#23837=CARTESIAN_POINT('Ctrl Pts',(-0.985642622920821,-1.,1.65110016612638));
#23838=CARTESIAN_POINT('Ctrl Pts',(-0.985642622920821,1.,1.65110016612638));
#23839=CARTESIAN_POINT('Ctrl Pts',(-0.981562530939489,-1.,1.64665139190656));
#23840=CARTESIAN_POINT('Ctrl Pts',(-0.981562530939489,1.,1.64665139190656));
#23841=CARTESIAN_POINT('Ctrl Pts',(-0.977689794119416,-1.,1.64233990826687));
#23842=CARTESIAN_POINT('Ctrl Pts',(-0.977689794119416,1.,1.64233990826687));
#23843=CARTESIAN_POINT('Ctrl Pts',(-0.974066058287418,-1.,1.63820952658144));
#23844=CARTESIAN_POINT('Ctrl Pts',(-0.974066058287418,1.,1.63820952658144));
#23845=CARTESIAN_POINT('Ctrl Pts',(-0.970669715997509,-1.,1.63420665729798));
#23846=CARTESIAN_POINT('Ctrl Pts',(-0.970669715997509,1.,1.63420665729798));
#23847=CARTESIAN_POINT('Ctrl Pts',(-0.967387853230345,-1.,1.63013849959461));
#23848=CARTESIAN_POINT('Ctrl Pts',(-0.967387853230345,1.,1.63013849959461));
#23849=CARTESIAN_POINT('Ctrl Pts',(-0.964046107040536,-1.,1.62571930670187));
#23850=CARTESIAN_POINT('Ctrl Pts',(-0.964046107040536,1.,1.62571930670187));
#23851=CARTESIAN_POINT('Ctrl Pts',(-0.960438326101729,-1.,1.62061638140221));
#23852=CARTESIAN_POINT('Ctrl Pts',(-0.960438326101729,1.,1.62061638140221));
#23853=CARTESIAN_POINT('Ctrl Pts',(-0.956354422920671,-1.,1.61449324337085));
#23854=CARTESIAN_POINT('Ctrl Pts',(-0.956354422920671,1.,1.61449324337085));
#23855=CARTESIAN_POINT('Ctrl Pts',(-0.951613284356035,-1.,1.60706069896936));
#23856=CARTESIAN_POINT('Ctrl Pts',(-0.951613284356035,1.,1.60706069896936));
#23857=CARTESIAN_POINT('Ctrl Pts',(-0.946078063315257,-1.,1.59810042043673));
#23858=CARTESIAN_POINT('Ctrl Pts',(-0.946078063315257,1.,1.59810042043673));
#23859=CARTESIAN_POINT('Ctrl Pts',(-0.939646377893399,-1.,1.58744937487176));
#23860=CARTESIAN_POINT('Ctrl Pts',(-0.939646377893399,1.,1.58744937487176));
#23861=CARTESIAN_POINT('Ctrl Pts',(-0.932246680108685,-1.,1.57499388382243));
#23862=CARTESIAN_POINT('Ctrl Pts',(-0.932246680108685,1.,1.57499388382243));
#23863=CARTESIAN_POINT('Ctrl Pts',(-0.923832188944341,-1.,1.56065988578893));
#23864=CARTESIAN_POINT('Ctrl Pts',(-0.923832188944341,1.,1.56065988578893));
#23865=CARTESIAN_POINT('Ctrl Pts',(-0.914375919026456,-1.,1.54440491149498));
#23866=CARTESIAN_POINT('Ctrl Pts',(-0.914375919026456,1.,1.54440491149498));
#23867=CARTESIAN_POINT('Ctrl Pts',(-0.905967409625651,-1.,1.52984849887993));
#23868=CARTESIAN_POINT('Ctrl Pts',(-0.905967409625651,1.,1.52984849887993));
#23869=CARTESIAN_POINT('Ctrl Pts',(-0.899185047483511,-1.,1.51805569590094));
#23870=CARTESIAN_POINT('Ctrl Pts',(-0.899185047483511,1.,1.51805569590094));
#23871=CARTESIAN_POINT('Ctrl Pts',(-0.894452006964543,-1.,1.50980486806688));
#23872=CARTESIAN_POINT('Ctrl Pts',(-0.894452006964543,1.,1.50980486806688));
#23873=CARTESIAN_POINT('Ctrl Pts',(-0.892032620296855,-1.,1.5055822144029));
#23874=CARTESIAN_POINT('Ctrl Pts',(-0.892032620296855,1.,1.5055822144029));
#23875=CARTESIAN_POINT('',(-1.23627494547115,1.,1.81978687191668));
#23876=CARTESIAN_POINT('Ctrl Pts',(-1.23627494547115,1.,1.81978687191668));
#23877=CARTESIAN_POINT('Ctrl Pts',(-1.23509651170476,1.,1.81925017193666));
#23878=CARTESIAN_POINT('Ctrl Pts',(-1.2327422452705,1.,1.81817389921279));
#23879=CARTESIAN_POINT('Ctrl Pts',(-1.2292186489137,1.,1.8165508718364));
#23880=CARTESIAN_POINT('Ctrl Pts',(-1.2245361330495,1.,1.81436959210434));
#23881=CARTESIAN_POINT('Ctrl Pts',(-1.21870906103557,1.,1.81161420806656));
#23882=CARTESIAN_POINT('Ctrl Pts',(-1.21290815708314,1.,1.80882996917129));
#23883=CARTESIAN_POINT('Ctrl Pts',(-1.20713356605475,1.,1.80601678480707));
#23884=CARTESIAN_POINT('Ctrl Pts',(-1.20138548938974,1.,1.80317454838603));
#23885=CARTESIAN_POINT('Ctrl Pts',(-1.19566418930242,1.,1.80030314369879));
#23886=CARTESIAN_POINT('Ctrl Pts',(-1.18996997934445,1.,1.79740245923478));
#23887=CARTESIAN_POINT('Ctrl Pts',(-1.18430321697432,1.,1.79447240321515));
#23888=CARTESIAN_POINT('Ctrl Pts',(-1.17866429440809,1.,1.79151291552689));
#23889=CARTESIAN_POINT('Ctrl Pts',(-1.17305363177328,1.,1.78852398877616));
#23890=CARTESIAN_POINT('Ctrl Pts',(-1.16747166312303,1.,1.78550566040443));
#23891=CARTESIAN_POINT('Ctrl Pts',(-1.16191881298499,1.,1.78245795881009));
#23892=CARTESIAN_POINT('Ctrl Pts',(-1.15639547194698,1.,1.77938085564275));
#23893=CARTESIAN_POINT('Ctrl Pts',(-1.15090197841515,1.,1.7762742255701));
#23894=CARTESIAN_POINT('Ctrl Pts',(-1.1454385822692,1.,1.77313777896194));
#23895=CARTESIAN_POINT('Ctrl Pts',(-1.14000548336975,1.,1.76997111386769));
#23896=CARTESIAN_POINT('Ctrl Pts',(-1.1346029180462,1.,1.76677384551862));
#23897=CARTESIAN_POINT('Ctrl Pts',(-1.12923123555075,1.,1.7635457196617));
#23898=CARTESIAN_POINT('Ctrl Pts',(-1.12389096855086,1.,1.76028671825096));
#23899=CARTESIAN_POINT('Ctrl Pts',(-1.11858293216763,1.,1.75699720772105));
#23900=CARTESIAN_POINT('Ctrl Pts',(-1.11330807582551,1.,1.7536777209463));
#23901=CARTESIAN_POINT('Ctrl Pts',(-1.10806728183007,1.,1.7503286607592));
#23902=CARTESIAN_POINT('Ctrl Pts',(-1.10286118991143,1.,1.74695004214923));
#23903=CARTESIAN_POINT('Ctrl Pts',(-1.09768999241225,1.,1.74354119236208));
#23904=CARTESIAN_POINT('Ctrl Pts',(-1.09255329056493,1.,1.74010053962247));
#23905=CARTESIAN_POINT('Ctrl Pts',(-1.08745056285427,1.,1.73662628326091));
#23906=CARTESIAN_POINT('Ctrl Pts',(-1.08238162784749,1.,1.73311705663407));
#23907=CARTESIAN_POINT('Ctrl Pts',(-1.0773470373727,1.,1.72957248977424));
#23908=CARTESIAN_POINT('Ctrl Pts',(-1.07234866990252,1.,1.72599406198488));
#23909=CARTESIAN_POINT('Ctrl Pts',(-1.06738966975462,1.,1.72238500928453));
#23910=CARTESIAN_POINT('Ctrl Pts',(-1.06247324680647,1.,1.71874858456904));
#23911=CARTESIAN_POINT('Ctrl Pts',(-1.05760163192479,1.,1.7150865442702));
#23912=CARTESIAN_POINT('Ctrl Pts',(-1.05277517202855,1.,1.71139783543989));
#23913=CARTESIAN_POINT('Ctrl Pts',(-1.04799085404995,1.,1.70767646263649));
#23914=CARTESIAN_POINT('Ctrl Pts',(-1.04324363334554,1.,1.70391338707982));
#23915=CARTESIAN_POINT('Ctrl Pts',(-1.03852922490789,1.,1.70010052930962));
#23916=CARTESIAN_POINT('Ctrl Pts',(-1.03384646003588,1.,1.69623414782771));
#23917=CARTESIAN_POINT('Ctrl Pts',(-1.02919977579147,1.,1.69231840863458));
#23918=CARTESIAN_POINT('Ctrl Pts',(-1.02460180535255,1.,1.68836910178447));
#23919=CARTESIAN_POINT('Ctrl Pts',(-1.02006795074201,1.,1.68440578021706));
#23920=CARTESIAN_POINT('Ctrl Pts',(-1.01561026162773,1.,1.68044289894798));
#23921=CARTESIAN_POINT('Ctrl Pts',(-1.01123236493511,1.,1.67648246776464));
#23922=CARTESIAN_POINT('Ctrl Pts',(-1.00692206696414,1.,1.67250335383293));
#23923=CARTESIAN_POINT('Ctrl Pts',(-1.00265091003727,1.,1.66846059277303));
#23924=CARTESIAN_POINT('Ctrl Pts',(-0.998389654952758,1.,1.66430758030376));
#23925=CARTESIAN_POINT('Ctrl Pts',(-0.994121836661306,1.,1.66001553809947));
#23926=CARTESIAN_POINT('Ctrl Pts',(-0.989855627854165,1.,1.65559044289699));
#23927=CARTESIAN_POINT('Ctrl Pts',(-0.985642622920821,1.,1.65110016612638));
#23928=CARTESIAN_POINT('Ctrl Pts',(-0.981562530939489,1.,1.64665139190656));
#23929=CARTESIAN_POINT('Ctrl Pts',(-0.977689794119416,1.,1.64233990826687));
#23930=CARTESIAN_POINT('Ctrl Pts',(-0.974066058287418,1.,1.63820952658144));
#23931=CARTESIAN_POINT('Ctrl Pts',(-0.970669715997509,1.,1.63420665729798));
#23932=CARTESIAN_POINT('Ctrl Pts',(-0.967387853230345,1.,1.63013849959461));
#23933=CARTESIAN_POINT('Ctrl Pts',(-0.964046107040536,1.,1.62571930670187));
#23934=CARTESIAN_POINT('Ctrl Pts',(-0.960438326101729,1.,1.62061638140221));
#23935=CARTESIAN_POINT('Ctrl Pts',(-0.956354422920671,1.,1.61449324337085));
#23936=CARTESIAN_POINT('Ctrl Pts',(-0.951613284356035,1.,1.60706069896936));
#23937=CARTESIAN_POINT('Ctrl Pts',(-0.946078063315257,1.,1.59810042043673));
#23938=CARTESIAN_POINT('Ctrl Pts',(-0.939646377893399,1.,1.58744937487176));
#23939=CARTESIAN_POINT('Ctrl Pts',(-0.932246680108685,1.,1.57499388382243));
#23940=CARTESIAN_POINT('Ctrl Pts',(-0.923832188944341,1.,1.56065988578893));
#23941=CARTESIAN_POINT('Ctrl Pts',(-0.914375919026456,1.,1.54440491149498));
#23942=CARTESIAN_POINT('Ctrl Pts',(-0.905967409625651,1.,1.52984849887993));
#23943=CARTESIAN_POINT('Ctrl Pts',(-0.899185047483511,1.,1.51805569590094));
#23944=CARTESIAN_POINT('Ctrl Pts',(-0.894452006964543,1.,1.50980486806688));
#23945=CARTESIAN_POINT('Ctrl Pts',(-0.892032620296855,1.,1.5055822144029));
#23946=CARTESIAN_POINT('',(-1.23627494547115,0.,1.81978687191668));
#23947=CARTESIAN_POINT('Origin',(-1.34869019493419,0.,1.73811241238545));
#23948=CARTESIAN_POINT('',(-1.34869019493419,1.,1.73811241238545));
#23949=CARTESIAN_POINT('',(-1.23627494547115,1.,1.81978687191668));
#23950=CARTESIAN_POINT('',(-1.34869019493419,0.,1.73811241238545));
#23951=CARTESIAN_POINT('Ctrl Pts',(-1.15624053661742,-1.,1.31362392696032));
#23952=CARTESIAN_POINT('Ctrl Pts',(-1.15624053661742,1.,1.31362392696032));
#23953=CARTESIAN_POINT('Ctrl Pts',(-1.15950888730809,-1.,1.31722977216397));
#23954=CARTESIAN_POINT('Ctrl Pts',(-1.15950888730809,1.,1.31722977216397));
#23955=CARTESIAN_POINT('Ctrl Pts',(-1.16589330093588,-1.,1.32428080721772));
#23956=CARTESIAN_POINT('Ctrl Pts',(-1.16589330093588,1.,1.32428080721772));
#23957=CARTESIAN_POINT('Ctrl Pts',(-1.17501305789857,-1.,1.33437539347008));
#23958=CARTESIAN_POINT('Ctrl Pts',(-1.17501305789857,1.,1.33437539347008));
#23959=CARTESIAN_POINT('Ctrl Pts',(-1.18625865667441,-1.,1.34687054001093));
#23960=CARTESIAN_POINT('Ctrl Pts',(-1.18625865667441,1.,1.34687054001093));
#23961=CARTESIAN_POINT('Ctrl Pts',(-1.1987959077932,-1.,1.36088705043885));
#23962=CARTESIAN_POINT('Ctrl Pts',(-1.1987959077932,1.,1.36088705043885));
#23963=CARTESIAN_POINT('Ctrl Pts',(-1.20982812925645,-1.,1.37331915607905));
#23964=CARTESIAN_POINT('Ctrl Pts',(-1.20982812925645,1.,1.37331915607905));
#23965=CARTESIAN_POINT('Ctrl Pts',(-1.21938737280852,-1.,1.38420564527715));
#23966=CARTESIAN_POINT('Ctrl Pts',(-1.21938737280852,1.,1.38420564527715));
#23967=CARTESIAN_POINT('Ctrl Pts',(-1.22752961899387,-1.,1.39361389568796));
#23968=CARTESIAN_POINT('Ctrl Pts',(-1.22752961899387,1.,1.39361389568796));
#23969=CARTESIAN_POINT('Ctrl Pts',(-1.23434087290423,-1.,1.40164708206106));
#23970=CARTESIAN_POINT('Ctrl Pts',(-1.23434087290423,1.,1.40164708206106));
#23971=CARTESIAN_POINT('Ctrl Pts',(-1.23994455029534,-1.,1.40845295531283));
#23972=CARTESIAN_POINT('Ctrl Pts',(-1.23994455029534,1.,1.40845295531283));
#23973=CARTESIAN_POINT('Ctrl Pts',(-1.24450600513056,-1.,1.41422913175179));
#23974=CARTESIAN_POINT('Ctrl Pts',(-1.24450600513056,1.,1.41422913175179));
#23975=CARTESIAN_POINT('Ctrl Pts',(-1.24824430986571,-1.,1.41923722596025));
#23976=CARTESIAN_POINT('Ctrl Pts',(-1.24824430986571,1.,1.41923722596025));
#23977=CARTESIAN_POINT('Ctrl Pts',(-1.2514145557001,-1.,1.42378102115575));
#23978=CARTESIAN_POINT('Ctrl Pts',(-1.2514145557001,1.,1.42378102115575));
#23979=CARTESIAN_POINT('Ctrl Pts',(-1.25426945222639,-1.,1.42815938799387));
#23980=CARTESIAN_POINT('Ctrl Pts',(-1.25426945222639,1.,1.42815938799387));
#23981=CARTESIAN_POINT('Ctrl Pts',(-1.25702687965755,-1.,1.43262645609691));
#23982=CARTESIAN_POINT('Ctrl Pts',(-1.25702687965755,1.,1.43262645609691));
#23983=CARTESIAN_POINT('Ctrl Pts',(-1.25983531012005,-1.,1.43734919180848));
#23984=CARTESIAN_POINT('Ctrl Pts',(-1.25983531012005,1.,1.43734919180848));
#23985=CARTESIAN_POINT('Ctrl Pts',(-1.26273903323859,-1.,1.44236470511303));
#23986=CARTESIAN_POINT('Ctrl Pts',(-1.26273903323859,1.,1.44236470511303));
#23987=CARTESIAN_POINT('Ctrl Pts',(-1.26570925118868,-1.,1.44761985001662));
#23988=CARTESIAN_POINT('Ctrl Pts',(-1.26570925118868,1.,1.44761985001662));
#23989=CARTESIAN_POINT('Ctrl Pts',(-1.2686778680489,-1.,1.45301422764247));
#23990=CARTESIAN_POINT('Ctrl Pts',(-1.2686778680489,1.,1.45301422764247));
#23991=CARTESIAN_POINT('Ctrl Pts',(-1.27156805265289,-1.,1.45843906294697));
#23992=CARTESIAN_POINT('Ctrl Pts',(-1.27156805265289,1.,1.45843906294697));
#23993=CARTESIAN_POINT('Ctrl Pts',(-1.27433119897822,-1.,1.46382431332476));
#23994=CARTESIAN_POINT('Ctrl Pts',(-1.27433119897822,1.,1.46382431332476));
#23995=CARTESIAN_POINT('Ctrl Pts',(-1.27696414831089,-1.,1.46916035917133));
#23996=CARTESIAN_POINT('Ctrl Pts',(-1.27696414831089,1.,1.46916035917133));
#23997=CARTESIAN_POINT('Ctrl Pts',(-1.2794891824849,-1.,1.4744717526707));
#23998=CARTESIAN_POINT('Ctrl Pts',(-1.2794891824849,1.,1.4744717526707));
#23999=CARTESIAN_POINT('Ctrl Pts',(-1.28194158939517,-1.,1.47980070347095));
#24000=CARTESIAN_POINT('Ctrl Pts',(-1.28194158939517,1.,1.47980070347095));
#24001=CARTESIAN_POINT('Ctrl Pts',(-1.28435533880201,-1.,1.4851881711891));
#24002=CARTESIAN_POINT('Ctrl Pts',(-1.28435533880201,1.,1.4851881711891));
#24003=CARTESIAN_POINT('Ctrl Pts',(-1.2867467611644,-1.,1.4906522831278));
#24004=CARTESIAN_POINT('Ctrl Pts',(-1.2867467611644,1.,1.4906522831278));
#24005=CARTESIAN_POINT('Ctrl Pts',(-1.28911506584254,-1.,1.49618896881754));
#24006=CARTESIAN_POINT('Ctrl Pts',(-1.28911506584254,1.,1.49618896881754));
#24007=CARTESIAN_POINT('Ctrl Pts',(-1.29145022885181,-1.,1.50178230149776));
#24008=CARTESIAN_POINT('Ctrl Pts',(-1.29145022885181,1.,1.50178230149776));
#24009=CARTESIAN_POINT('Ctrl Pts',(-1.29373841372842,-1.,1.50741159078365));
#24010=CARTESIAN_POINT('Ctrl Pts',(-1.29373841372842,1.,1.50741159078365));
#24011=CARTESIAN_POINT('Ctrl Pts',(-1.29596850710509,-1.,1.51305994241402));
#24012=CARTESIAN_POINT('Ctrl Pts',(-1.29596850710509,1.,1.51305994241402));
#24013=CARTESIAN_POINT('Ctrl Pts',(-1.29813791800747,-1.,1.51872184912724));
#24014=CARTESIAN_POINT('Ctrl Pts',(-1.29813791800747,1.,1.51872184912724));
#24015=CARTESIAN_POINT('Ctrl Pts',(-1.30024984366328,-1.,1.52439957861062));
#24016=CARTESIAN_POINT('Ctrl Pts',(-1.30024984366328,1.,1.52439957861062));
#24017=CARTESIAN_POINT('Ctrl Pts',(-1.30231064395568,-1.,1.53009970283891));
#24018=CARTESIAN_POINT('Ctrl Pts',(-1.30231064395568,1.,1.53009970283891));
#24019=CARTESIAN_POINT('Ctrl Pts',(-1.30432735639489,-1.,1.53582981268977));
#24020=CARTESIAN_POINT('Ctrl Pts',(-1.30432735639489,1.,1.53582981268977));
#24021=CARTESIAN_POINT('Ctrl Pts',(-1.30630475189556,-1.,1.54159462645432));
#24022=CARTESIAN_POINT('Ctrl Pts',(-1.30630475189556,1.,1.54159462645432));
#24023=CARTESIAN_POINT('Ctrl Pts',(-1.30824393907473,-1.,1.54739413957185));
#24024=CARTESIAN_POINT('Ctrl Pts',(-1.30824393907473,1.,1.54739413957185));
#24025=CARTESIAN_POINT('Ctrl Pts',(-1.31014393684222,-1.,1.55322568759481));
#24026=CARTESIAN_POINT('Ctrl Pts',(-1.31014393684222,1.,1.55322568759481));
#24027=CARTESIAN_POINT('Ctrl Pts',(-1.31200264341696,-1.,1.55908521254821));
#24028=CARTESIAN_POINT('Ctrl Pts',(-1.31200264341696,1.,1.55908521254821));
#24029=CARTESIAN_POINT('Ctrl Pts',(-1.31381795281002,-1.,1.56496872402353));
#24030=CARTESIAN_POINT('Ctrl Pts',(-1.31381795281002,1.,1.56496872402353));
#24031=CARTESIAN_POINT('Ctrl Pts',(-1.31558903860016,-1.,1.57087397835723));
#24032=CARTESIAN_POINT('Ctrl Pts',(-1.31558903860016,1.,1.57087397835723));
#24033=CARTESIAN_POINT('Ctrl Pts',(-1.31731642317187,-1.,1.5768005650559));
#24034=CARTESIAN_POINT('Ctrl Pts',(-1.31731642317187,1.,1.5768005650559));
#24035=CARTESIAN_POINT('Ctrl Pts',(-1.31900135021432,-1.,1.58274907898834));
#24036=CARTESIAN_POINT('Ctrl Pts',(-1.31900135021432,1.,1.58274907898834));
#24037=CARTESIAN_POINT('Ctrl Pts',(-1.32064537110892,-1.,1.58872057258245));
#24038=CARTESIAN_POINT('Ctrl Pts',(-1.32064537110892,1.,1.58872057258245));
#24039=CARTESIAN_POINT('Ctrl Pts',(-1.32224985747682,-1.,1.59471591079403));
#24040=CARTESIAN_POINT('Ctrl Pts',(-1.32224985747682,1.,1.59471591079403));
#24041=CARTESIAN_POINT('Ctrl Pts',(-1.32381550858256,-1.,1.60073511858687));
#24042=CARTESIAN_POINT('Ctrl Pts',(-1.32381550858256,1.,1.60073511858687));
#24043=CARTESIAN_POINT('Ctrl Pts',(-1.32534250785782,-1.,1.60677758290954));
#24044=CARTESIAN_POINT('Ctrl Pts',(-1.32534250785782,1.,1.60677758290954));
#24045=CARTESIAN_POINT('Ctrl Pts',(-1.32683074483356,-1.,1.6128423401575));
#24046=CARTESIAN_POINT('Ctrl Pts',(-1.32683074483356,1.,1.6128423401575));
#24047=CARTESIAN_POINT('Ctrl Pts',(-1.32828000610449,-1.,1.61892832270724));
#24048=CARTESIAN_POINT('Ctrl Pts',(-1.32828000610449,1.,1.61892832270724));
#24049=CARTESIAN_POINT('Ctrl Pts',(-1.3296901950568,-1.,1.62503464209797));
#24050=CARTESIAN_POINT('Ctrl Pts',(-1.3296901950568,1.,1.62503464209797));
#24051=CARTESIAN_POINT('Ctrl Pts',(-1.33106149345645,-1.,1.63116079730923));
#24052=CARTESIAN_POINT('Ctrl Pts',(-1.33106149345645,1.,1.63116079730923));
#24053=CARTESIAN_POINT('Ctrl Pts',(-1.33239425103724,-1.,1.63730653475089));
#24054=CARTESIAN_POINT('Ctrl Pts',(-1.33239425103724,1.,1.63730653475089));
#24055=CARTESIAN_POINT('Ctrl Pts',(-1.33368890676572,-1.,1.6434717485603));
#24056=CARTESIAN_POINT('Ctrl Pts',(-1.33368890676572,1.,1.6434717485603));
#24057=CARTESIAN_POINT('Ctrl Pts',(-1.33494590467993,-1.,1.6496563728683));
#24058=CARTESIAN_POINT('Ctrl Pts',(-1.33494590467993,1.,1.6496563728683));
#24059=CARTESIAN_POINT('Ctrl Pts',(-1.33616559745172,-1.,1.65586025952593));
#24060=CARTESIAN_POINT('Ctrl Pts',(-1.33616559745172,1.,1.65586025952593));
#24061=CARTESIAN_POINT('Ctrl Pts',(-1.33734820885262,-1.,1.66208312541983));
#24062=CARTESIAN_POINT('Ctrl Pts',(-1.33734820885262,1.,1.66208312541983));
#24063=CARTESIAN_POINT('Ctrl Pts',(-1.33849388654388,-1.,1.66832460783989));
#24064=CARTESIAN_POINT('Ctrl Pts',(-1.33849388654388,1.,1.66832460783989));
#24065=CARTESIAN_POINT('Ctrl Pts',(-1.3396027347034,-1.,1.67458429426086));
#24066=CARTESIAN_POINT('Ctrl Pts',(-1.3396027347034,1.,1.67458429426086));
#24067=CARTESIAN_POINT('Ctrl Pts',(-1.34067485185203,-1.,1.68086176030362));
#24068=CARTESIAN_POINT('Ctrl Pts',(-1.34067485185203,1.,1.68086176030362));
#24069=CARTESIAN_POINT('Ctrl Pts',(-1.341710374848,-1.,1.68715660868764));
#24070=CARTESIAN_POINT('Ctrl Pts',(-1.341710374848,1.,1.68715660868764));
#24071=CARTESIAN_POINT('Ctrl Pts',(-1.34270948206319,-1.,1.6934684849687));
#24072=CARTESIAN_POINT('Ctrl Pts',(-1.34270948206319,1.,1.6934684849687));
#24073=CARTESIAN_POINT('Ctrl Pts',(-1.34367237124483,-1.,1.69979707754427));
#24074=CARTESIAN_POINT('Ctrl Pts',(-1.34367237124483,1.,1.69979707754427));
#24075=CARTESIAN_POINT('Ctrl Pts',(-1.34459924533831,-1.,1.70614212266738));
#24076=CARTESIAN_POINT('Ctrl Pts',(-1.34459924533831,1.,1.70614212266738));
#24077=CARTESIAN_POINT('Ctrl Pts',(-1.34549029589416,-1.,1.71250340686822));
#24078=CARTESIAN_POINT('Ctrl Pts',(-1.34549029589416,1.,1.71250340686822));
#24079=CARTESIAN_POINT('Ctrl Pts',(-1.34634568653227,-1.,1.7188807715049));
#24080=CARTESIAN_POINT('Ctrl Pts',(-1.34634568653227,1.,1.7188807715049));
#24081=CARTESIAN_POINT('Ctrl Pts',(-1.34716554819527,-1.,1.72527410680674));
#24082=CARTESIAN_POINT('Ctrl Pts',(-1.34716554819527,1.,1.72527410680674));
#24083=CARTESIAN_POINT('Ctrl Pts',(-1.34779309152035,-1.,1.7304014965394));
#24084=CARTESIAN_POINT('Ctrl Pts',(-1.34779309152035,1.,1.7304014965394));
#24085=CARTESIAN_POINT('Ctrl Pts',(-1.34824783112887,-1.,1.73425417885907));
#24086=CARTESIAN_POINT('Ctrl Pts',(-1.34824783112887,1.,1.73425417885907));
#24087=CARTESIAN_POINT('Ctrl Pts',(-1.34854391898045,-1.,1.73682580585691));
#24088=CARTESIAN_POINT('Ctrl Pts',(-1.34854391898045,1.,1.73682580585691));
#24089=CARTESIAN_POINT('Ctrl Pts',(-1.34869019493419,-1.,1.73811241238545));
#24090=CARTESIAN_POINT('Ctrl Pts',(-1.34869019493419,1.,1.73811241238545));
#24091=CARTESIAN_POINT('',(-1.15624053661742,1.,1.31362392696032));
#24092=CARTESIAN_POINT('Ctrl Pts',(-1.15624053661742,1.,1.31362392696032));
#24093=CARTESIAN_POINT('Ctrl Pts',(-1.15950888730809,1.,1.31722977216397));
#24094=CARTESIAN_POINT('Ctrl Pts',(-1.16589330093588,1.,1.32428080721772));
#24095=CARTESIAN_POINT('Ctrl Pts',(-1.17501305789857,1.,1.33437539347008));
#24096=CARTESIAN_POINT('Ctrl Pts',(-1.18625865667441,1.,1.34687054001093));
#24097=CARTESIAN_POINT('Ctrl Pts',(-1.1987959077932,1.,1.36088705043885));
#24098=CARTESIAN_POINT('Ctrl Pts',(-1.20982812925645,1.,1.37331915607905));
#24099=CARTESIAN_POINT('Ctrl Pts',(-1.21938737280852,1.,1.38420564527715));
#24100=CARTESIAN_POINT('Ctrl Pts',(-1.22752961899387,1.,1.39361389568796));
#24101=CARTESIAN_POINT('Ctrl Pts',(-1.23434087290423,1.,1.40164708206106));
#24102=CARTESIAN_POINT('Ctrl Pts',(-1.23994455029534,1.,1.40845295531283));
#24103=CARTESIAN_POINT('Ctrl Pts',(-1.24450600513056,1.,1.41422913175179));
#24104=CARTESIAN_POINT('Ctrl Pts',(-1.24824430986571,1.,1.41923722596025));
#24105=CARTESIAN_POINT('Ctrl Pts',(-1.2514145557001,1.,1.42378102115575));
#24106=CARTESIAN_POINT('Ctrl Pts',(-1.25426945222639,1.,1.42815938799387));
#24107=CARTESIAN_POINT('Ctrl Pts',(-1.25702687965755,1.,1.43262645609691));
#24108=CARTESIAN_POINT('Ctrl Pts',(-1.25983531012005,1.,1.43734919180848));
#24109=CARTESIAN_POINT('Ctrl Pts',(-1.26273903323859,1.,1.44236470511303));
#24110=CARTESIAN_POINT('Ctrl Pts',(-1.26570925118868,1.,1.44761985001662));
#24111=CARTESIAN_POINT('Ctrl Pts',(-1.2686778680489,1.,1.45301422764247));
#24112=CARTESIAN_POINT('Ctrl Pts',(-1.27156805265289,1.,1.45843906294697));
#24113=CARTESIAN_POINT('Ctrl Pts',(-1.27433119897822,1.,1.46382431332476));
#24114=CARTESIAN_POINT('Ctrl Pts',(-1.27696414831089,1.,1.46916035917133));
#24115=CARTESIAN_POINT('Ctrl Pts',(-1.2794891824849,1.,1.4744717526707));
#24116=CARTESIAN_POINT('Ctrl Pts',(-1.28194158939517,1.,1.47980070347095));
#24117=CARTESIAN_POINT('Ctrl Pts',(-1.28435533880201,1.,1.4851881711891));
#24118=CARTESIAN_POINT('Ctrl Pts',(-1.2867467611644,1.,1.4906522831278));
#24119=CARTESIAN_POINT('Ctrl Pts',(-1.28911506584254,1.,1.49618896881754));
#24120=CARTESIAN_POINT('Ctrl Pts',(-1.29145022885181,1.,1.50178230149776));
#24121=CARTESIAN_POINT('Ctrl Pts',(-1.29373841372842,1.,1.50741159078365));
#24122=CARTESIAN_POINT('Ctrl Pts',(-1.29596850710509,1.,1.51305994241402));
#24123=CARTESIAN_POINT('Ctrl Pts',(-1.29813791800747,1.,1.51872184912724));
#24124=CARTESIAN_POINT('Ctrl Pts',(-1.30024984366328,1.,1.52439957861062));
#24125=CARTESIAN_POINT('Ctrl Pts',(-1.30231064395568,1.,1.53009970283891));
#24126=CARTESIAN_POINT('Ctrl Pts',(-1.30432735639489,1.,1.53582981268977));
#24127=CARTESIAN_POINT('Ctrl Pts',(-1.30630475189556,1.,1.54159462645432));
#24128=CARTESIAN_POINT('Ctrl Pts',(-1.30824393907473,1.,1.54739413957185));
#24129=CARTESIAN_POINT('Ctrl Pts',(-1.31014393684222,1.,1.55322568759481));
#24130=CARTESIAN_POINT('Ctrl Pts',(-1.31200264341696,1.,1.55908521254821));
#24131=CARTESIAN_POINT('Ctrl Pts',(-1.31381795281002,1.,1.56496872402353));
#24132=CARTESIAN_POINT('Ctrl Pts',(-1.31558903860016,1.,1.57087397835723));
#24133=CARTESIAN_POINT('Ctrl Pts',(-1.31731642317187,1.,1.5768005650559));
#24134=CARTESIAN_POINT('Ctrl Pts',(-1.31900135021432,1.,1.58274907898834));
#24135=CARTESIAN_POINT('Ctrl Pts',(-1.32064537110892,1.,1.58872057258245));
#24136=CARTESIAN_POINT('Ctrl Pts',(-1.32224985747682,1.,1.59471591079403));
#24137=CARTESIAN_POINT('Ctrl Pts',(-1.32381550858256,1.,1.60073511858687));
#24138=CARTESIAN_POINT('Ctrl Pts',(-1.32534250785782,1.,1.60677758290954));
#24139=CARTESIAN_POINT('Ctrl Pts',(-1.32683074483356,1.,1.6128423401575));
#24140=CARTESIAN_POINT('Ctrl Pts',(-1.32828000610449,1.,1.61892832270724));
#24141=CARTESIAN_POINT('Ctrl Pts',(-1.3296901950568,1.,1.62503464209797));
#24142=CARTESIAN_POINT('Ctrl Pts',(-1.33106149345645,1.,1.63116079730923));
#24143=CARTESIAN_POINT('Ctrl Pts',(-1.33239425103724,1.,1.63730653475089));
#24144=CARTESIAN_POINT('Ctrl Pts',(-1.33368890676572,1.,1.6434717485603));
#24145=CARTESIAN_POINT('Ctrl Pts',(-1.33494590467993,1.,1.6496563728683));
#24146=CARTESIAN_POINT('Ctrl Pts',(-1.33616559745172,1.,1.65586025952593));
#24147=CARTESIAN_POINT('Ctrl Pts',(-1.33734820885262,1.,1.66208312541983));
#24148=CARTESIAN_POINT('Ctrl Pts',(-1.33849388654388,1.,1.66832460783989));
#24149=CARTESIAN_POINT('Ctrl Pts',(-1.3396027347034,1.,1.67458429426086));
#24150=CARTESIAN_POINT('Ctrl Pts',(-1.34067485185203,1.,1.68086176030362));
#24151=CARTESIAN_POINT('Ctrl Pts',(-1.341710374848,1.,1.68715660868764));
#24152=CARTESIAN_POINT('Ctrl Pts',(-1.34270948206319,1.,1.6934684849687));
#24153=CARTESIAN_POINT('Ctrl Pts',(-1.34367237124483,1.,1.69979707754427));
#24154=CARTESIAN_POINT('Ctrl Pts',(-1.34459924533831,1.,1.70614212266738));
#24155=CARTESIAN_POINT('Ctrl Pts',(-1.34549029589416,1.,1.71250340686822));
#24156=CARTESIAN_POINT('Ctrl Pts',(-1.34634568653227,1.,1.7188807715049));
#24157=CARTESIAN_POINT('Ctrl Pts',(-1.34716554819527,1.,1.72527410680674));
#24158=CARTESIAN_POINT('Ctrl Pts',(-1.34779309152035,1.,1.7304014965394));
#24159=CARTESIAN_POINT('Ctrl Pts',(-1.34824783112887,1.,1.73425417885907));
#24160=CARTESIAN_POINT('Ctrl Pts',(-1.34854391898045,1.,1.73682580585691));
#24161=CARTESIAN_POINT('Ctrl Pts',(-1.34869019493419,1.,1.73811241238545));
#24162=CARTESIAN_POINT('',(-1.15624053661742,0.,1.31362392696032));
#24163=CARTESIAN_POINT('Origin',(0.,0.,0.));
#24164=CARTESIAN_POINT('',(-1.31362392696033,1.,1.15624053661742));
#24165=CARTESIAN_POINT('Origin',(0.,1.,0.));
#24166=CARTESIAN_POINT('',(-1.31362392696033,0.,1.15624053661742));
#24167=CARTESIAN_POINT('Ctrl Pts',(-1.73811241238545,-1.,1.34869019493419));
#24168=CARTESIAN_POINT('Ctrl Pts',(-1.73811241238545,1.,1.34869019493419));
#24169=CARTESIAN_POINT('Ctrl Pts',(-1.73682580585819,-1.,1.34854391898145));
#24170=CARTESIAN_POINT('Ctrl Pts',(-1.73682580585819,1.,1.34854391898145));
#24171=CARTESIAN_POINT('Ctrl Pts',(-1.73425417886255,-1.,1.34824783113158));
#24172=CARTESIAN_POINT('Ctrl Pts',(-1.73425417886255,1.,1.34824783113158));
#24173=CARTESIAN_POINT('Ctrl Pts',(-1.73040149654497,-1.,1.3477930915247));
#24174=CARTESIAN_POINT('Ctrl Pts',(-1.73040149654497,1.,1.3477930915247));
#24175=CARTESIAN_POINT('Ctrl Pts',(-1.72527410681298,-1.,1.34716554820013));
#24176=CARTESIAN_POINT('Ctrl Pts',(-1.72527410681298,1.,1.34716554820013));
#24177=CARTESIAN_POINT('Ctrl Pts',(-1.7188807715095,-1.,1.34634568653586));
#24178=CARTESIAN_POINT('Ctrl Pts',(-1.7188807715095,1.,1.34634568653586));
#24179=CARTESIAN_POINT('Ctrl Pts',(-1.71250340687011,-1.,1.34549029589563));
#24180=CARTESIAN_POINT('Ctrl Pts',(-1.71250340687011,1.,1.34549029589563));
#24181=CARTESIAN_POINT('Ctrl Pts',(-1.70614212266676,-1.,1.34459924533783));
#24182=CARTESIAN_POINT('Ctrl Pts',(-1.70614212266676,1.,1.34459924533783));
#24183=CARTESIAN_POINT('Ctrl Pts',(-1.69979707754221,-1.,1.34367237124322));
#24184=CARTESIAN_POINT('Ctrl Pts',(-1.69979707754221,1.,1.34367237124322));
#24185=CARTESIAN_POINT('Ctrl Pts',(-1.6934684849664,-1.,1.34270948206139));
#24186=CARTESIAN_POINT('Ctrl Pts',(-1.6934684849664,1.,1.34270948206139));
#24187=CARTESIAN_POINT('Ctrl Pts',(-1.68715660868602,-1.,1.34171037484673));
#24188=CARTESIAN_POINT('Ctrl Pts',(-1.68715660868602,1.,1.34171037484673));
#24189=CARTESIAN_POINT('Ctrl Pts',(-1.68086176030308,-1.,1.3406748518516));
#24190=CARTESIAN_POINT('Ctrl Pts',(-1.68086176030308,1.,1.3406748518516));
#24191=CARTESIAN_POINT('Ctrl Pts',(-1.67458429426126,-1.,1.33960273470372));
#24192=CARTESIAN_POINT('Ctrl Pts',(-1.67458429426126,1.,1.33960273470372));
#24193=CARTESIAN_POINT('Ctrl Pts',(-1.66832460784078,-1.,1.33849388654458));
#24194=CARTESIAN_POINT('Ctrl Pts',(-1.66832460784078,1.,1.33849388654458));
#24195=CARTESIAN_POINT('Ctrl Pts',(-1.66208312542073,-1.,1.33734820885331));
#24196=CARTESIAN_POINT('Ctrl Pts',(-1.66208312542073,1.,1.33734820885331));
#24197=CARTESIAN_POINT('Ctrl Pts',(-1.65586025952651,-1.,1.33616559745217));
#24198=CARTESIAN_POINT('Ctrl Pts',(-1.65586025952651,1.,1.33616559745217));
#24199=CARTESIAN_POINT('Ctrl Pts',(-1.64965637286843,-1.,1.33494590468003));
#24200=CARTESIAN_POINT('Ctrl Pts',(-1.64965637286843,1.,1.33494590468003));
#24201=CARTESIAN_POINT('Ctrl Pts',(-1.64347174856007,-1.,1.33368890676554));
#24202=CARTESIAN_POINT('Ctrl Pts',(-1.64347174856007,1.,1.33368890676554));
#24203=CARTESIAN_POINT('Ctrl Pts',(-1.6373065347505,-1.,1.33239425103694));
#24204=CARTESIAN_POINT('Ctrl Pts',(-1.6373065347505,1.,1.33239425103694));
#24205=CARTESIAN_POINT('Ctrl Pts',(-1.63116079730887,-1.,1.33106149345618));
#24206=CARTESIAN_POINT('Ctrl Pts',(-1.63116079730887,1.,1.33106149345618));
#24207=CARTESIAN_POINT('Ctrl Pts',(-1.62503464209777,-1.,1.32969019505665));
#24208=CARTESIAN_POINT('Ctrl Pts',(-1.62503464209777,1.,1.32969019505665));
#24209=CARTESIAN_POINT('Ctrl Pts',(-1.61892832270723,-1.,1.32828000610448));
#24210=CARTESIAN_POINT('Ctrl Pts',(-1.61892832270723,1.,1.32828000610448));
#24211=CARTESIAN_POINT('Ctrl Pts',(-1.61284234015762,-1.,1.32683074483365));
#24212=CARTESIAN_POINT('Ctrl Pts',(-1.61284234015762,1.,1.32683074483365));
#24213=CARTESIAN_POINT('Ctrl Pts',(-1.6067775829097,-1.,1.32534250785794));
#24214=CARTESIAN_POINT('Ctrl Pts',(-1.6067775829097,1.,1.32534250785794));
#24215=CARTESIAN_POINT('Ctrl Pts',(-1.600735118587,-1.,1.32381550858266));
#24216=CARTESIAN_POINT('Ctrl Pts',(-1.600735118587,1.,1.32381550858266));
#24217=CARTESIAN_POINT('Ctrl Pts',(-1.59471591079408,-1.,1.32224985747686));
#24218=CARTESIAN_POINT('Ctrl Pts',(-1.59471591079408,1.,1.32224985747686));
#24219=CARTESIAN_POINT('Ctrl Pts',(-1.58872057258244,-1.,1.32064537110891));
#24220=CARTESIAN_POINT('Ctrl Pts',(-1.58872057258244,1.,1.32064537110891));
#24221=CARTESIAN_POINT('Ctrl Pts',(-1.58274907898829,-1.,1.31900135021428));
#24222=CARTESIAN_POINT('Ctrl Pts',(-1.58274907898829,1.,1.31900135021428));
#24223=CARTESIAN_POINT('Ctrl Pts',(-1.57680056505585,-1.,1.31731642317183));
#24224=CARTESIAN_POINT('Ctrl Pts',(-1.57680056505585,1.,1.31731642317183));
#24225=CARTESIAN_POINT('Ctrl Pts',(-1.57087397835721,-1.,1.31558903860015));
#24226=CARTESIAN_POINT('Ctrl Pts',(-1.57087397835721,1.,1.31558903860015));
#24227=CARTESIAN_POINT('Ctrl Pts',(-1.56496872402352,-1.,1.31381795281002));
#24228=CARTESIAN_POINT('Ctrl Pts',(-1.56496872402352,1.,1.31381795281002));
#24229=CARTESIAN_POINT('Ctrl Pts',(-1.55908521254822,-1.,1.31200264341696));
#24230=CARTESIAN_POINT('Ctrl Pts',(-1.55908521254822,1.,1.31200264341696));
#24231=CARTESIAN_POINT('Ctrl Pts',(-1.55322568759481,-1.,1.31014393684221));
#24232=CARTESIAN_POINT('Ctrl Pts',(-1.55322568759481,1.,1.31014393684221));
#24233=CARTESIAN_POINT('Ctrl Pts',(-1.54739413957183,-1.,1.30824393907471));
#24234=CARTESIAN_POINT('Ctrl Pts',(-1.54739413957183,1.,1.30824393907471));
#24235=CARTESIAN_POINT('Ctrl Pts',(-1.54159462645428,-1.,1.30630475189553));
#24236=CARTESIAN_POINT('Ctrl Pts',(-1.54159462645428,1.,1.30630475189553));
#24237=CARTESIAN_POINT('Ctrl Pts',(-1.53582981268976,-1.,1.30432735639487));
#24238=CARTESIAN_POINT('Ctrl Pts',(-1.53582981268976,1.,1.30432735639487));
#24239=CARTESIAN_POINT('Ctrl Pts',(-1.53009970283893,-1.,1.3023106439557));
#24240=CARTESIAN_POINT('Ctrl Pts',(-1.53009970283893,1.,1.3023106439557));
#24241=CARTESIAN_POINT('Ctrl Pts',(-1.5243995786107,-1.,1.30024984366334));
#24242=CARTESIAN_POINT('Ctrl Pts',(-1.5243995786107,1.,1.30024984366334));
#24243=CARTESIAN_POINT('Ctrl Pts',(-1.51872184912735,-1.,1.29813791800757));
#24244=CARTESIAN_POINT('Ctrl Pts',(-1.51872184912735,1.,1.29813791800757));
#24245=CARTESIAN_POINT('Ctrl Pts',(-1.51305994241412,-1.,1.29596850710518));
#24246=CARTESIAN_POINT('Ctrl Pts',(-1.51305994241412,1.,1.29596850710518));
#24247=CARTESIAN_POINT('Ctrl Pts',(-1.50741159078367,-1.,1.29373841372843));
#24248=CARTESIAN_POINT('Ctrl Pts',(-1.50741159078367,1.,1.29373841372843));
#24249=CARTESIAN_POINT('Ctrl Pts',(-1.50178230149764,-1.,1.29145022885171));
#24250=CARTESIAN_POINT('Ctrl Pts',(-1.50178230149764,1.,1.29145022885171));
#24251=CARTESIAN_POINT('Ctrl Pts',(-1.49618896881729,-1.,1.28911506584232));
#24252=CARTESIAN_POINT('Ctrl Pts',(-1.49618896881729,1.,1.28911506584232));
#24253=CARTESIAN_POINT('Ctrl Pts',(-1.4906522831275,-1.,1.28674676116415));
#24254=CARTESIAN_POINT('Ctrl Pts',(-1.4906522831275,1.,1.28674676116415));
#24255=CARTESIAN_POINT('Ctrl Pts',(-1.48518817118891,-1.,1.28435533880184));
#24256=CARTESIAN_POINT('Ctrl Pts',(-1.48518817118891,1.,1.28435533880184));
#24257=CARTESIAN_POINT('Ctrl Pts',(-1.47980070347102,-1.,1.28194158939522));
#24258=CARTESIAN_POINT('Ctrl Pts',(-1.47980070347102,1.,1.28194158939522));
#24259=CARTESIAN_POINT('Ctrl Pts',(-1.4744717526711,-1.,1.27948918248524));
#24260=CARTESIAN_POINT('Ctrl Pts',(-1.4744717526711,1.,1.27948918248524));
#24261=CARTESIAN_POINT('Ctrl Pts',(-1.46916035917197,-1.,1.27696414831144));
#24262=CARTESIAN_POINT('Ctrl Pts',(-1.46916035917197,1.,1.27696414831144));
#24263=CARTESIAN_POINT('Ctrl Pts',(-1.4638243133254,-1.,1.27433119897877));
#24264=CARTESIAN_POINT('Ctrl Pts',(-1.4638243133254,1.,1.27433119897877));
#24265=CARTESIAN_POINT('Ctrl Pts',(-1.45843906294725,-1.,1.27156805265312));
#24266=CARTESIAN_POINT('Ctrl Pts',(-1.45843906294725,1.,1.27156805265312));
#24267=CARTESIAN_POINT('Ctrl Pts',(-1.45301422764205,-1.,1.26867786804854));
#24268=CARTESIAN_POINT('Ctrl Pts',(-1.45301422764205,1.,1.26867786804854));
#24269=CARTESIAN_POINT('Ctrl Pts',(-1.44761985001544,-1.,1.26570925118767));
#24270=CARTESIAN_POINT('Ctrl Pts',(-1.44761985001544,1.,1.26570925118767));
#24271=CARTESIAN_POINT('Ctrl Pts',(-1.44236470511145,-1.,1.26273903323723));
#24272=CARTESIAN_POINT('Ctrl Pts',(-1.44236470511145,1.,1.26273903323723));
#24273=CARTESIAN_POINT('Ctrl Pts',(-1.43734919180719,-1.,1.25983531011894));
#24274=CARTESIAN_POINT('Ctrl Pts',(-1.43734919180719,1.,1.25983531011894));
#24275=CARTESIAN_POINT('Ctrl Pts',(-1.43262645609679,-1.,1.25702687965744));
#24276=CARTESIAN_POINT('Ctrl Pts',(-1.43262645609679,1.,1.25702687965744));
#24277=CARTESIAN_POINT('Ctrl Pts',(-1.42815938799555,-1.,1.25426945222783));
#24278=CARTESIAN_POINT('Ctrl Pts',(-1.42815938799555,1.,1.25426945222783));
#24279=CARTESIAN_POINT('Ctrl Pts',(-1.42378102115911,-1.,1.25141455570299));
#24280=CARTESIAN_POINT('Ctrl Pts',(-1.42378102115911,1.,1.25141455570299));
#24281=CARTESIAN_POINT('Ctrl Pts',(-1.41923722596421,-1.,1.24824430986911));
#24282=CARTESIAN_POINT('Ctrl Pts',(-1.41923722596421,1.,1.24824430986911));
#24283=CARTESIAN_POINT('Ctrl Pts',(-1.41422913175437,-1.,1.24450600513278));
#24284=CARTESIAN_POINT('Ctrl Pts',(-1.41422913175437,1.,1.24450600513278));
#24285=CARTESIAN_POINT('Ctrl Pts',(-1.40845295531151,-1.,1.23994455029421));
#24286=CARTESIAN_POINT('Ctrl Pts',(-1.40845295531151,1.,1.23994455029421));
#24287=CARTESIAN_POINT('Ctrl Pts',(-1.40164708205345,-1.,1.23434087289768));
#24288=CARTESIAN_POINT('Ctrl Pts',(-1.40164708205345,1.,1.23434087289768));
#24289=CARTESIAN_POINT('Ctrl Pts',(-1.39361389567257,-1.,1.22752961898063));
#24290=CARTESIAN_POINT('Ctrl Pts',(-1.39361389567257,1.,1.22752961898063));
#24291=CARTESIAN_POINT('Ctrl Pts',(-1.38420564525391,-1.,1.21938737278853));
#24292=CARTESIAN_POINT('Ctrl Pts',(-1.38420564525391,1.,1.21938737278853));
#24293=CARTESIAN_POINT('Ctrl Pts',(-1.37331915604962,-1.,1.20982812923113));
#24294=CARTESIAN_POINT('Ctrl Pts',(-1.37331915604962,1.,1.20982812923113));
#24295=CARTESIAN_POINT('Ctrl Pts',(-1.36088705040677,-1.,1.1987959077656));
#24296=CARTESIAN_POINT('Ctrl Pts',(-1.36088705040677,1.,1.1987959077656));
#24297=CARTESIAN_POINT('Ctrl Pts',(-1.34687053998157,-1.,1.18625865664915));
#24298=CARTESIAN_POINT('Ctrl Pts',(-1.34687053998157,1.,1.18625865664915));
#24299=CARTESIAN_POINT('Ctrl Pts',(-1.33437539344842,-1.,1.17501305787994));
#24300=CARTESIAN_POINT('Ctrl Pts',(-1.33437539344842,1.,1.17501305787994));
#24301=CARTESIAN_POINT('Ctrl Pts',(-1.32428080720544,-1.,1.16589330092532));
#24302=CARTESIAN_POINT('Ctrl Pts',(-1.32428080720544,1.,1.16589330092532));
#24303=CARTESIAN_POINT('Ctrl Pts',(-1.3172297721596,-1.,1.15950888730433));
#24304=CARTESIAN_POINT('Ctrl Pts',(-1.3172297721596,1.,1.15950888730433));
#24305=CARTESIAN_POINT('Ctrl Pts',(-1.31362392696033,-1.,1.15624053661742));
#24306=CARTESIAN_POINT('Ctrl Pts',(-1.31362392696033,1.,1.15624053661742));
#24307=CARTESIAN_POINT('',(-1.73811241238545,1.,1.34869019493419));
#24308=CARTESIAN_POINT('Ctrl Pts',(-1.73811241238545,1.,1.34869019493419));
#24309=CARTESIAN_POINT('Ctrl Pts',(-1.73682580585819,1.,1.34854391898145));
#24310=CARTESIAN_POINT('Ctrl Pts',(-1.73425417886255,1.,1.34824783113158));
#24311=CARTESIAN_POINT('Ctrl Pts',(-1.73040149654497,1.,1.3477930915247));
#24312=CARTESIAN_POINT('Ctrl Pts',(-1.72527410681298,1.,1.34716554820013));
#24313=CARTESIAN_POINT('Ctrl Pts',(-1.7188807715095,1.,1.34634568653586));
#24314=CARTESIAN_POINT('Ctrl Pts',(-1.71250340687011,1.,1.34549029589563));
#24315=CARTESIAN_POINT('Ctrl Pts',(-1.70614212266676,1.,1.34459924533783));
#24316=CARTESIAN_POINT('Ctrl Pts',(-1.69979707754221,1.,1.34367237124322));
#24317=CARTESIAN_POINT('Ctrl Pts',(-1.6934684849664,1.,1.34270948206139));
#24318=CARTESIAN_POINT('Ctrl Pts',(-1.68715660868602,1.,1.34171037484673));
#24319=CARTESIAN_POINT('Ctrl Pts',(-1.68086176030308,1.,1.3406748518516));
#24320=CARTESIAN_POINT('Ctrl Pts',(-1.67458429426126,1.,1.33960273470372));
#24321=CARTESIAN_POINT('Ctrl Pts',(-1.66832460784078,1.,1.33849388654458));
#24322=CARTESIAN_POINT('Ctrl Pts',(-1.66208312542073,1.,1.33734820885331));
#24323=CARTESIAN_POINT('Ctrl Pts',(-1.65586025952651,1.,1.33616559745217));
#24324=CARTESIAN_POINT('Ctrl Pts',(-1.64965637286843,1.,1.33494590468003));
#24325=CARTESIAN_POINT('Ctrl Pts',(-1.64347174856007,1.,1.33368890676554));
#24326=CARTESIAN_POINT('Ctrl Pts',(-1.6373065347505,1.,1.33239425103694));
#24327=CARTESIAN_POINT('Ctrl Pts',(-1.63116079730887,1.,1.33106149345618));
#24328=CARTESIAN_POINT('Ctrl Pts',(-1.62503464209777,1.,1.32969019505665));
#24329=CARTESIAN_POINT('Ctrl Pts',(-1.61892832270723,1.,1.32828000610448));
#24330=CARTESIAN_POINT('Ctrl Pts',(-1.61284234015762,1.,1.32683074483365));
#24331=CARTESIAN_POINT('Ctrl Pts',(-1.6067775829097,1.,1.32534250785794));
#24332=CARTESIAN_POINT('Ctrl Pts',(-1.600735118587,1.,1.32381550858266));
#24333=CARTESIAN_POINT('Ctrl Pts',(-1.59471591079408,1.,1.32224985747686));
#24334=CARTESIAN_POINT('Ctrl Pts',(-1.58872057258244,1.,1.32064537110891));
#24335=CARTESIAN_POINT('Ctrl Pts',(-1.58274907898829,1.,1.31900135021428));
#24336=CARTESIAN_POINT('Ctrl Pts',(-1.57680056505585,1.,1.31731642317183));
#24337=CARTESIAN_POINT('Ctrl Pts',(-1.57087397835721,1.,1.31558903860015));
#24338=CARTESIAN_POINT('Ctrl Pts',(-1.56496872402352,1.,1.31381795281002));
#24339=CARTESIAN_POINT('Ctrl Pts',(-1.55908521254822,1.,1.31200264341696));
#24340=CARTESIAN_POINT('Ctrl Pts',(-1.55322568759481,1.,1.31014393684221));
#24341=CARTESIAN_POINT('Ctrl Pts',(-1.54739413957183,1.,1.30824393907471));
#24342=CARTESIAN_POINT('Ctrl Pts',(-1.54159462645428,1.,1.30630475189553));
#24343=CARTESIAN_POINT('Ctrl Pts',(-1.53582981268976,1.,1.30432735639487));
#24344=CARTESIAN_POINT('Ctrl Pts',(-1.53009970283893,1.,1.3023106439557));
#24345=CARTESIAN_POINT('Ctrl Pts',(-1.5243995786107,1.,1.30024984366334));
#24346=CARTESIAN_POINT('Ctrl Pts',(-1.51872184912735,1.,1.29813791800757));
#24347=CARTESIAN_POINT('Ctrl Pts',(-1.51305994241412,1.,1.29596850710518));
#24348=CARTESIAN_POINT('Ctrl Pts',(-1.50741159078367,1.,1.29373841372843));
#24349=CARTESIAN_POINT('Ctrl Pts',(-1.50178230149764,1.,1.29145022885171));
#24350=CARTESIAN_POINT('Ctrl Pts',(-1.49618896881729,1.,1.28911506584232));
#24351=CARTESIAN_POINT('Ctrl Pts',(-1.4906522831275,1.,1.28674676116415));
#24352=CARTESIAN_POINT('Ctrl Pts',(-1.48518817118891,1.,1.28435533880184));
#24353=CARTESIAN_POINT('Ctrl Pts',(-1.47980070347102,1.,1.28194158939522));
#24354=CARTESIAN_POINT('Ctrl Pts',(-1.4744717526711,1.,1.27948918248524));
#24355=CARTESIAN_POINT('Ctrl Pts',(-1.46916035917197,1.,1.27696414831144));
#24356=CARTESIAN_POINT('Ctrl Pts',(-1.4638243133254,1.,1.27433119897877));
#24357=CARTESIAN_POINT('Ctrl Pts',(-1.45843906294725,1.,1.27156805265312));
#24358=CARTESIAN_POINT('Ctrl Pts',(-1.45301422764205,1.,1.26867786804854));
#24359=CARTESIAN_POINT('Ctrl Pts',(-1.44761985001544,1.,1.26570925118767));
#24360=CARTESIAN_POINT('Ctrl Pts',(-1.44236470511145,1.,1.26273903323723));
#24361=CARTESIAN_POINT('Ctrl Pts',(-1.43734919180719,1.,1.25983531011894));
#24362=CARTESIAN_POINT('Ctrl Pts',(-1.43262645609679,1.,1.25702687965744));
#24363=CARTESIAN_POINT('Ctrl Pts',(-1.42815938799555,1.,1.25426945222783));
#24364=CARTESIAN_POINT('Ctrl Pts',(-1.42378102115911,1.,1.25141455570299));
#24365=CARTESIAN_POINT('Ctrl Pts',(-1.41923722596421,1.,1.24824430986911));
#24366=CARTESIAN_POINT('Ctrl Pts',(-1.41422913175437,1.,1.24450600513278));
#24367=CARTESIAN_POINT('Ctrl Pts',(-1.40845295531151,1.,1.23994455029421));
#24368=CARTESIAN_POINT('Ctrl Pts',(-1.40164708205345,1.,1.23434087289768));
#24369=CARTESIAN_POINT('Ctrl Pts',(-1.39361389567257,1.,1.22752961898063));
#24370=CARTESIAN_POINT('Ctrl Pts',(-1.38420564525391,1.,1.21938737278853));
#24371=CARTESIAN_POINT('Ctrl Pts',(-1.37331915604962,1.,1.20982812923113));
#24372=CARTESIAN_POINT('Ctrl Pts',(-1.36088705040677,1.,1.1987959077656));
#24373=CARTESIAN_POINT('Ctrl Pts',(-1.34687053998157,1.,1.18625865664915));
#24374=CARTESIAN_POINT('Ctrl Pts',(-1.33437539344842,1.,1.17501305787994));
#24375=CARTESIAN_POINT('Ctrl Pts',(-1.32428080720544,1.,1.16589330092532));
#24376=CARTESIAN_POINT('Ctrl Pts',(-1.3172297721596,1.,1.15950888730433));
#24377=CARTESIAN_POINT('Ctrl Pts',(-1.31362392696033,1.,1.15624053661742));
#24378=CARTESIAN_POINT('',(-1.73811241238545,0.,1.34869019493419));
#24379=CARTESIAN_POINT('Origin',(-1.81978687191668,0.,1.23627494547115));
#24380=CARTESIAN_POINT('',(-1.81978687191668,1.,1.23627494547115));
#24381=CARTESIAN_POINT('',(-1.73811241238545,1.,1.34869019493419));
#24382=CARTESIAN_POINT('',(-1.81978687191668,0.,1.23627494547115));
#24383=CARTESIAN_POINT('Ctrl Pts',(-1.5055822144029,-1.,0.892032620296855));
#24384=CARTESIAN_POINT('Ctrl Pts',(-1.5055822144029,1.,0.892032620296855));
#24385=CARTESIAN_POINT('Ctrl Pts',(-1.50980486807181,-1.,0.894452006967538));
#24386=CARTESIAN_POINT('Ctrl Pts',(-1.50980486807181,1.,0.894452006967538));
#24387=CARTESIAN_POINT('Ctrl Pts',(-1.51805569591479,-1.,0.89918504749193));
#24388=CARTESIAN_POINT('Ctrl Pts',(-1.51805569591479,1.,0.89918504749193));
#24389=CARTESIAN_POINT('Ctrl Pts',(-1.52984849890434,-1.,0.905967409640499));
#24390=CARTESIAN_POINT('Ctrl Pts',(-1.52984849890434,1.,0.905967409640499));
#24391=CARTESIAN_POINT('Ctrl Pts',(-1.54440491152808,-1.,0.91437591904658));
#24392=CARTESIAN_POINT('Ctrl Pts',(-1.54440491152808,1.,0.91437591904658));
#24393=CARTESIAN_POINT('Ctrl Pts',(-1.56065988582509,-1.,0.923832188966322));
#24394=CARTESIAN_POINT('Ctrl Pts',(-1.56065988582509,1.,0.923832188966322));
#24395=CARTESIAN_POINT('Ctrl Pts',(-1.57499388385561,-1.,0.932246680128849));
#24396=CARTESIAN_POINT('Ctrl Pts',(-1.57499388385561,1.,0.932246680128849));
#24397=CARTESIAN_POINT('Ctrl Pts',(-1.58744937489796,-1.,0.939646377909319));
#24398=CARTESIAN_POINT('Ctrl Pts',(-1.58744937489796,1.,0.939646377909319));
#24399=CARTESIAN_POINT('Ctrl Pts',(-1.59810042045408,-1.,0.946078063325796));
#24400=CARTESIAN_POINT('Ctrl Pts',(-1.59810042045408,1.,0.946078063325796));
#24401=CARTESIAN_POINT('Ctrl Pts',(-1.60706069897794,-1.,0.951613284361248));
#24402=CARTESIAN_POINT('Ctrl Pts',(-1.60706069897794,1.,0.951613284361248));
#24403=CARTESIAN_POINT('Ctrl Pts',(-1.61449324337233,-1.,0.956354422921573));
#24404=CARTESIAN_POINT('Ctrl Pts',(-1.61449324337233,1.,0.956354422921573));
#24405=CARTESIAN_POINT('Ctrl Pts',(-1.62061638139929,-1.,0.960438326099958));
#24406=CARTESIAN_POINT('Ctrl Pts',(-1.62061638139929,1.,0.960438326099958));
#24407=CARTESIAN_POINT('Ctrl Pts',(-1.6257193066974,-1.,0.964046107037821));
#24408=CARTESIAN_POINT('Ctrl Pts',(-1.6257193066974,1.,0.964046107037821));
#24409=CARTESIAN_POINT('Ctrl Pts',(-1.63013849959083,-1.,0.967387853228041));
#24410=CARTESIAN_POINT('Ctrl Pts',(-1.63013849959083,1.,0.967387853228041));
#24411=CARTESIAN_POINT('Ctrl Pts',(-1.63420665729609,-1.,0.970669715996356));
#24412=CARTESIAN_POINT('Ctrl Pts',(-1.63420665729609,1.,0.970669715996356));
#24413=CARTESIAN_POINT('Ctrl Pts',(-1.63820952658157,-1.,0.974066058287501));
#24414=CARTESIAN_POINT('Ctrl Pts',(-1.63820952658157,1.,0.974066058287501));
#24415=CARTESIAN_POINT('Ctrl Pts',(-1.64233990826831,-1.,0.977689794120297));
#24416=CARTESIAN_POINT('Ctrl Pts',(-1.64233990826831,1.,0.977689794120297));
#24417=CARTESIAN_POINT('Ctrl Pts',(-1.64665139190834,-1.,0.981562530940574));
#24418=CARTESIAN_POINT('Ctrl Pts',(-1.64665139190834,1.,0.981562530940574));
#24419=CARTESIAN_POINT('Ctrl Pts',(-1.6511001661277,-1.,0.985642622921626));
#24420=CARTESIAN_POINT('Ctrl Pts',(-1.6511001661277,1.,0.985642622921626));
#24421=CARTESIAN_POINT('Ctrl Pts',(-1.65559044289746,-1.,0.98985562785445));
#24422=CARTESIAN_POINT('Ctrl Pts',(-1.65559044289746,1.,0.98985562785445));
#24423=CARTESIAN_POINT('Ctrl Pts',(-1.66001553809916,-1.,0.994121836661116));
#24424=CARTESIAN_POINT('Ctrl Pts',(-1.66001553809916,1.,0.994121836661116));
#24425=CARTESIAN_POINT('Ctrl Pts',(-1.66430758030304,-1.,0.998389654952317));
#24426=CARTESIAN_POINT('Ctrl Pts',(-1.66430758030304,1.,0.998389654952317));
#24427=CARTESIAN_POINT('Ctrl Pts',(-1.66846059277231,-1.,1.00265091003682));
#24428=CARTESIAN_POINT('Ctrl Pts',(-1.66846059277231,1.,1.00265091003682));
#24429=CARTESIAN_POINT('Ctrl Pts',(-1.67250335383248,-1.,1.00692206696387));
#24430=CARTESIAN_POINT('Ctrl Pts',(-1.67250335383248,1.,1.00692206696387));
#24431=CARTESIAN_POINT('Ctrl Pts',(-1.67648246776457,-1.,1.01123236493507));
#24432=CARTESIAN_POINT('Ctrl Pts',(-1.67648246776457,1.,1.01123236493507));
#24433=CARTESIAN_POINT('Ctrl Pts',(-1.6804428989482,-1.,1.01561026162787));
#24434=CARTESIAN_POINT('Ctrl Pts',(-1.6804428989482,1.,1.01561026162787));
#24435=CARTESIAN_POINT('Ctrl Pts',(-1.68440578021739,-1.,1.02006795074222));
#24436=CARTESIAN_POINT('Ctrl Pts',(-1.68440578021739,1.,1.02006795074222));
#24437=CARTESIAN_POINT('Ctrl Pts',(-1.68836910178475,-1.,1.02460180535272));
#24438=CARTESIAN_POINT('Ctrl Pts',(-1.68836910178475,1.,1.02460180535272));
#24439=CARTESIAN_POINT('Ctrl Pts',(-1.69231840863471,-1.,1.02919977579155));
#24440=CARTESIAN_POINT('Ctrl Pts',(-1.69231840863471,1.,1.02919977579155));
#24441=CARTESIAN_POINT('Ctrl Pts',(-1.69623414782769,-1.,1.03384646003587));
#24442=CARTESIAN_POINT('Ctrl Pts',(-1.69623414782769,1.,1.03384646003587));
#24443=CARTESIAN_POINT('Ctrl Pts',(-1.70010052930951,-1.,1.03852922490782));
#24444=CARTESIAN_POINT('Ctrl Pts',(-1.70010052930951,1.,1.03852922490782));
#24445=CARTESIAN_POINT('Ctrl Pts',(-1.70391338707969,-1.,1.04324363334546));
#24446=CARTESIAN_POINT('Ctrl Pts',(-1.70391338707969,1.,1.04324363334546));
#24447=CARTESIAN_POINT('Ctrl Pts',(-1.70767646263641,-1.,1.0479908540499));
#24448=CARTESIAN_POINT('Ctrl Pts',(-1.70767646263641,1.,1.0479908540499));
#24449=CARTESIAN_POINT('Ctrl Pts',(-1.71139783543986,-1.,1.05277517202854));
#24450=CARTESIAN_POINT('Ctrl Pts',(-1.71139783543986,1.,1.05277517202854));
#24451=CARTESIAN_POINT('Ctrl Pts',(-1.71508654427022,-1.,1.05760163192481));
#24452=CARTESIAN_POINT('Ctrl Pts',(-1.71508654427022,1.,1.05760163192481));
#24453=CARTESIAN_POINT('Ctrl Pts',(-1.71874858456908,-1.,1.0624732468065));
#24454=CARTESIAN_POINT('Ctrl Pts',(-1.71874858456908,1.,1.0624732468065));
#24455=CARTESIAN_POINT('Ctrl Pts',(-1.72238500928456,-1.,1.06738966975463));
#24456=CARTESIAN_POINT('Ctrl Pts',(-1.72238500928456,1.,1.06738966975463));
#24457=CARTESIAN_POINT('Ctrl Pts',(-1.72599406198489,-1.,1.07234866990252));
#24458=CARTESIAN_POINT('Ctrl Pts',(-1.72599406198489,1.,1.07234866990252));
#24459=CARTESIAN_POINT('Ctrl Pts',(-1.72957248977424,-1.,1.0773470373727));
#24460=CARTESIAN_POINT('Ctrl Pts',(-1.72957248977424,1.,1.0773470373727));
#24461=CARTESIAN_POINT('Ctrl Pts',(-1.73311705663407,-1.,1.08238162784749));
#24462=CARTESIAN_POINT('Ctrl Pts',(-1.73311705663407,1.,1.08238162784749));
#24463=CARTESIAN_POINT('Ctrl Pts',(-1.73662628326093,-1.,1.08745056285429));
#24464=CARTESIAN_POINT('Ctrl Pts',(-1.73662628326093,1.,1.08745056285429));
#24465=CARTESIAN_POINT('Ctrl Pts',(-1.74010053962252,-1.,1.09255329056496));
#24466=CARTESIAN_POINT('Ctrl Pts',(-1.74010053962252,1.,1.09255329056496));
#24467=CARTESIAN_POINT('Ctrl Pts',(-1.74354119236212,-1.,1.09768999241229));
#24468=CARTESIAN_POINT('Ctrl Pts',(-1.74354119236212,1.,1.09768999241229));
#24469=CARTESIAN_POINT('Ctrl Pts',(-1.74695004214924,-1.,1.10286118991144));
#24470=CARTESIAN_POINT('Ctrl Pts',(-1.74695004214924,1.,1.10286118991144));
#24471=CARTESIAN_POINT('Ctrl Pts',(-1.75032866075914,-1.,1.10806728183003));
#24472=CARTESIAN_POINT('Ctrl Pts',(-1.75032866075914,1.,1.10806728183003));
#24473=CARTESIAN_POINT('Ctrl Pts',(-1.75367772094617,-1.,1.11330807582542));
#24474=CARTESIAN_POINT('Ctrl Pts',(-1.75367772094617,1.,1.11330807582542));
#24475=CARTESIAN_POINT('Ctrl Pts',(-1.75699720772089,-1.,1.11858293216752));
#24476=CARTESIAN_POINT('Ctrl Pts',(-1.75699720772089,1.,1.11858293216752));
#24477=CARTESIAN_POINT('Ctrl Pts',(-1.76028671825084,-1.,1.12389096855078));
#24478=CARTESIAN_POINT('Ctrl Pts',(-1.76028671825084,1.,1.12389096855078));
#24479=CARTESIAN_POINT('Ctrl Pts',(-1.76354571966171,-1.,1.12923123555076));
#24480=CARTESIAN_POINT('Ctrl Pts',(-1.76354571966171,1.,1.12923123555076));
#24481=CARTESIAN_POINT('Ctrl Pts',(-1.76677384551883,-1.,1.13460291804635));
#24482=CARTESIAN_POINT('Ctrl Pts',(-1.76677384551883,1.,1.13460291804635));
#24483=CARTESIAN_POINT('Ctrl Pts',(-1.76997111386806,-1.,1.14000548337));
#24484=CARTESIAN_POINT('Ctrl Pts',(-1.76997111386806,1.,1.14000548337));
#24485=CARTESIAN_POINT('Ctrl Pts',(-1.77313777896234,-1.,1.14543858226948));
#24486=CARTESIAN_POINT('Ctrl Pts',(-1.77313777896234,1.,1.14543858226948));
#24487=CARTESIAN_POINT('Ctrl Pts',(-1.77627422557034,-1.,1.15090197841531));
#24488=CARTESIAN_POINT('Ctrl Pts',(-1.77627422557034,1.,1.15090197841531));
#24489=CARTESIAN_POINT('Ctrl Pts',(-1.77938085564261,-1.,1.15639547194689));
#24490=CARTESIAN_POINT('Ctrl Pts',(-1.77938085564261,1.,1.15639547194689));
#24491=CARTESIAN_POINT('Ctrl Pts',(-1.78245795880949,-1.,1.16191881298458));
#24492=CARTESIAN_POINT('Ctrl Pts',(-1.78245795880949,1.,1.16191881298458));
#24493=CARTESIAN_POINT('Ctrl Pts',(-1.78550566040349,-1.,1.16747166312239));
#24494=CARTESIAN_POINT('Ctrl Pts',(-1.78550566040349,1.,1.16747166312239));
#24495=CARTESIAN_POINT('Ctrl Pts',(-1.78852398877523,-1.,1.17305363177265));
#24496=CARTESIAN_POINT('Ctrl Pts',(-1.78852398877523,1.,1.17305363177265));
#24497=CARTESIAN_POINT('Ctrl Pts',(-1.79151291552646,-1.,1.17866429440781));
#24498=CARTESIAN_POINT('Ctrl Pts',(-1.79151291552646,1.,1.17866429440781));
#24499=CARTESIAN_POINT('Ctrl Pts',(-1.79447240321572,-1.,1.18430321697471));
#24500=CARTESIAN_POINT('Ctrl Pts',(-1.79447240321572,1.,1.18430321697471));
#24501=CARTESIAN_POINT('Ctrl Pts',(-1.79740245923649,-1.,1.1899699793456));
#24502=CARTESIAN_POINT('Ctrl Pts',(-1.79740245923649,1.,1.1899699793456));
#24503=CARTESIAN_POINT('Ctrl Pts',(-1.80030314370121,-1.,1.19566418930405));
#24504=CARTESIAN_POINT('Ctrl Pts',(-1.80030314370121,1.,1.19566418930405));
#24505=CARTESIAN_POINT('Ctrl Pts',(-1.8031745483882,-1.,1.2013854893912));
#24506=CARTESIAN_POINT('Ctrl Pts',(-1.8031745483882,1.,1.2013854893912));
#24507=CARTESIAN_POINT('Ctrl Pts',(-1.80601678480772,-1.,1.20713356605519));
#24508=CARTESIAN_POINT('Ctrl Pts',(-1.80601678480772,1.,1.20713356605519));
#24509=CARTESIAN_POINT('Ctrl Pts',(-1.80882996916931,-1.,1.2129081570818));
#24510=CARTESIAN_POINT('Ctrl Pts',(-1.80882996916931,1.,1.2129081570818));
#24511=CARTESIAN_POINT('Ctrl Pts',(-1.81161420806172,-1.,1.2187090610323));
#24512=CARTESIAN_POINT('Ctrl Pts',(-1.81161420806172,1.,1.2187090610323));
#24513=CARTESIAN_POINT('Ctrl Pts',(-1.81436959209778,-1.,1.22453613304507));
#24514=CARTESIAN_POINT('Ctrl Pts',(-1.81436959209778,1.,1.22453613304507));
#24515=CARTESIAN_POINT('Ctrl Pts',(-1.81655087183054,-1.,1.22921864890975));
#24516=CARTESIAN_POINT('Ctrl Pts',(-1.81655087183054,1.,1.22921864890975));
#24517=CARTESIAN_POINT('Ctrl Pts',(-1.81817389920914,-1.,1.23274224526804));
#24518=CARTESIAN_POINT('Ctrl Pts',(-1.81817389920914,1.,1.23274224526804));
#24519=CARTESIAN_POINT('Ctrl Pts',(-1.81925017193531,-1.,1.23509651170384));
#24520=CARTESIAN_POINT('Ctrl Pts',(-1.81925017193531,1.,1.23509651170384));
#24521=CARTESIAN_POINT('Ctrl Pts',(-1.81978687191668,-1.,1.23627494547115));
#24522=CARTESIAN_POINT('Ctrl Pts',(-1.81978687191668,1.,1.23627494547115));
#24523=CARTESIAN_POINT('',(-1.5055822144029,1.,0.892032620296855));
#24524=CARTESIAN_POINT('Ctrl Pts',(-1.5055822144029,1.,0.892032620296855));
#24525=CARTESIAN_POINT('Ctrl Pts',(-1.50980486807181,1.,0.894452006967538));
#24526=CARTESIAN_POINT('Ctrl Pts',(-1.51805569591479,1.,0.89918504749193));
#24527=CARTESIAN_POINT('Ctrl Pts',(-1.52984849890434,1.,0.905967409640499));
#24528=CARTESIAN_POINT('Ctrl Pts',(-1.54440491152808,1.,0.91437591904658));
#24529=CARTESIAN_POINT('Ctrl Pts',(-1.56065988582509,1.,0.923832188966322));
#24530=CARTESIAN_POINT('Ctrl Pts',(-1.57499388385561,1.,0.932246680128849));
#24531=CARTESIAN_POINT('Ctrl Pts',(-1.58744937489796,1.,0.939646377909319));
#24532=CARTESIAN_POINT('Ctrl Pts',(-1.59810042045408,1.,0.946078063325796));
#24533=CARTESIAN_POINT('Ctrl Pts',(-1.60706069897794,1.,0.951613284361248));
#24534=CARTESIAN_POINT('Ctrl Pts',(-1.61449324337233,1.,0.956354422921573));
#24535=CARTESIAN_POINT('Ctrl Pts',(-1.62061638139929,1.,0.960438326099958));
#24536=CARTESIAN_POINT('Ctrl Pts',(-1.6257193066974,1.,0.964046107037821));
#24537=CARTESIAN_POINT('Ctrl Pts',(-1.63013849959083,1.,0.967387853228041));
#24538=CARTESIAN_POINT('Ctrl Pts',(-1.63420665729609,1.,0.970669715996356));
#24539=CARTESIAN_POINT('Ctrl Pts',(-1.63820952658157,1.,0.974066058287501));
#24540=CARTESIAN_POINT('Ctrl Pts',(-1.64233990826831,1.,0.977689794120297));
#24541=CARTESIAN_POINT('Ctrl Pts',(-1.64665139190834,1.,0.981562530940574));
#24542=CARTESIAN_POINT('Ctrl Pts',(-1.6511001661277,1.,0.985642622921626));
#24543=CARTESIAN_POINT('Ctrl Pts',(-1.65559044289746,1.,0.98985562785445));
#24544=CARTESIAN_POINT('Ctrl Pts',(-1.66001553809916,1.,0.994121836661116));
#24545=CARTESIAN_POINT('Ctrl Pts',(-1.66430758030304,1.,0.998389654952317));
#24546=CARTESIAN_POINT('Ctrl Pts',(-1.66846059277231,1.,1.00265091003682));
#24547=CARTESIAN_POINT('Ctrl Pts',(-1.67250335383248,1.,1.00692206696387));
#24548=CARTESIAN_POINT('Ctrl Pts',(-1.67648246776457,1.,1.01123236493507));
#24549=CARTESIAN_POINT('Ctrl Pts',(-1.6804428989482,1.,1.01561026162787));
#24550=CARTESIAN_POINT('Ctrl Pts',(-1.68440578021739,1.,1.02006795074222));
#24551=CARTESIAN_POINT('Ctrl Pts',(-1.68836910178475,1.,1.02460180535272));
#24552=CARTESIAN_POINT('Ctrl Pts',(-1.69231840863471,1.,1.02919977579155));
#24553=CARTESIAN_POINT('Ctrl Pts',(-1.69623414782769,1.,1.03384646003587));
#24554=CARTESIAN_POINT('Ctrl Pts',(-1.70010052930951,1.,1.03852922490782));
#24555=CARTESIAN_POINT('Ctrl Pts',(-1.70391338707969,1.,1.04324363334546));
#24556=CARTESIAN_POINT('Ctrl Pts',(-1.70767646263641,1.,1.0479908540499));
#24557=CARTESIAN_POINT('Ctrl Pts',(-1.71139783543986,1.,1.05277517202854));
#24558=CARTESIAN_POINT('Ctrl Pts',(-1.71508654427022,1.,1.05760163192481));
#24559=CARTESIAN_POINT('Ctrl Pts',(-1.71874858456908,1.,1.0624732468065));
#24560=CARTESIAN_POINT('Ctrl Pts',(-1.72238500928456,1.,1.06738966975463));
#24561=CARTESIAN_POINT('Ctrl Pts',(-1.72599406198489,1.,1.07234866990252));
#24562=CARTESIAN_POINT('Ctrl Pts',(-1.72957248977424,1.,1.0773470373727));
#24563=CARTESIAN_POINT('Ctrl Pts',(-1.73311705663407,1.,1.08238162784749));
#24564=CARTESIAN_POINT('Ctrl Pts',(-1.73662628326093,1.,1.08745056285429));
#24565=CARTESIAN_POINT('Ctrl Pts',(-1.74010053962252,1.,1.09255329056496));
#24566=CARTESIAN_POINT('Ctrl Pts',(-1.74354119236212,1.,1.09768999241229));
#24567=CARTESIAN_POINT('Ctrl Pts',(-1.74695004214924,1.,1.10286118991144));
#24568=CARTESIAN_POINT('Ctrl Pts',(-1.75032866075914,1.,1.10806728183003));
#24569=CARTESIAN_POINT('Ctrl Pts',(-1.75367772094617,1.,1.11330807582542));
#24570=CARTESIAN_POINT('Ctrl Pts',(-1.75699720772089,1.,1.11858293216752));
#24571=CARTESIAN_POINT('Ctrl Pts',(-1.76028671825084,1.,1.12389096855078));
#24572=CARTESIAN_POINT('Ctrl Pts',(-1.76354571966171,1.,1.12923123555076));
#24573=CARTESIAN_POINT('Ctrl Pts',(-1.76677384551883,1.,1.13460291804635));
#24574=CARTESIAN_POINT('Ctrl Pts',(-1.76997111386806,1.,1.14000548337));
#24575=CARTESIAN_POINT('Ctrl Pts',(-1.77313777896234,1.,1.14543858226948));
#24576=CARTESIAN_POINT('Ctrl Pts',(-1.77627422557034,1.,1.15090197841531));
#24577=CARTESIAN_POINT('Ctrl Pts',(-1.77938085564261,1.,1.15639547194689));
#24578=CARTESIAN_POINT('Ctrl Pts',(-1.78245795880949,1.,1.16191881298458));
#24579=CARTESIAN_POINT('Ctrl Pts',(-1.78550566040349,1.,1.16747166312239));
#24580=CARTESIAN_POINT('Ctrl Pts',(-1.78852398877523,1.,1.17305363177265));
#24581=CARTESIAN_POINT('Ctrl Pts',(-1.79151291552646,1.,1.17866429440781));
#24582=CARTESIAN_POINT('Ctrl Pts',(-1.79447240321572,1.,1.18430321697471));
#24583=CARTESIAN_POINT('Ctrl Pts',(-1.79740245923649,1.,1.1899699793456));
#24584=CARTESIAN_POINT('Ctrl Pts',(-1.80030314370121,1.,1.19566418930405));
#24585=CARTESIAN_POINT('Ctrl Pts',(-1.8031745483882,1.,1.2013854893912));
#24586=CARTESIAN_POINT('Ctrl Pts',(-1.80601678480772,1.,1.20713356605519));
#24587=CARTESIAN_POINT('Ctrl Pts',(-1.80882996916931,1.,1.2129081570818));
#24588=CARTESIAN_POINT('Ctrl Pts',(-1.81161420806172,1.,1.2187090610323));
#24589=CARTESIAN_POINT('Ctrl Pts',(-1.81436959209778,1.,1.22453613304507));
#24590=CARTESIAN_POINT('Ctrl Pts',(-1.81655087183054,1.,1.22921864890975));
#24591=CARTESIAN_POINT('Ctrl Pts',(-1.81817389920914,1.,1.23274224526804));
#24592=CARTESIAN_POINT('Ctrl Pts',(-1.81925017193531,1.,1.23509651170384));
#24593=CARTESIAN_POINT('Ctrl Pts',(-1.81978687191668,1.,1.23627494547115));
#24594=CARTESIAN_POINT('',(-1.5055822144029,0.,0.892032620296856));
#24595=CARTESIAN_POINT('Origin',(0.,0.,0.));
#24596=CARTESIAN_POINT('',(-1.60662857109684,1.,0.693717979106305));
#24597=CARTESIAN_POINT('Origin',(0.,1.,0.));
#24598=CARTESIAN_POINT('',(-1.60662857109684,0.,0.693717979106306));
#24599=CARTESIAN_POINT('Ctrl Pts',(-2.0698113262342,-1.,0.7455743247944));
#24600=CARTESIAN_POINT('Ctrl Pts',(-2.0698113262342,1.,0.7455743247944));
#24601=CARTESIAN_POINT('Ctrl Pts',(-2.06854248895728,-1.,0.745832791378367));
#24602=CARTESIAN_POINT('Ctrl Pts',(-2.06854248895728,1.,0.745832791378367));
#24603=CARTESIAN_POINT('Ctrl Pts',(-2.06600523016815,-1.,0.7463458715442));
#24604=CARTESIAN_POINT('Ctrl Pts',(-2.06600523016815,1.,0.7463458715442));
#24605=CARTESIAN_POINT('Ctrl Pts',(-2.06220058927826,-1.,0.747103932787919));
#24606=CARTESIAN_POINT('Ctrl Pts',(-2.06220058927826,1.,0.747103932787919));
#24607=CARTESIAN_POINT('Ctrl Pts',(-2.05713023031006,-1.,0.748091554183802));
#24608=CARTESIAN_POINT('Ctrl Pts',(-2.05713023031006,1.,0.748091554183802));
#24609=CARTESIAN_POINT('Ctrl Pts',(-2.05079645592154,-1.,0.749287468665046));
#24610=CARTESIAN_POINT('Ctrl Pts',(-2.05079645592154,1.,0.749287468665046));
#24611=CARTESIAN_POINT('Ctrl Pts',(-2.04446689147979,-1.,0.750444657875576));
#24612=CARTESIAN_POINT('Ctrl Pts',(-2.04446689147979,1.,0.750444657875576));
#24613=CARTESIAN_POINT('Ctrl Pts',(-2.03814160092099,-1.,0.751562963361115));
#24614=CARTESIAN_POINT('Ctrl Pts',(-2.03814160092099,1.,0.751562963361115));
#24615=CARTESIAN_POINT('Ctrl Pts',(-2.03182068456221,-1.,0.752642180487211));
#24616=CARTESIAN_POINT('Ctrl Pts',(-2.03182068456221,1.,0.752642180487211));
#24617=CARTESIAN_POINT('Ctrl Pts',(-2.02550428623313,-1.,0.753682061112768));
#24618=CARTESIAN_POINT('Ctrl Pts',(-2.02550428623313,1.,0.753682061112768));
#24619=CARTESIAN_POINT('Ctrl Pts',(-2.01919259405809,-1.,0.754682330722816));
#24620=CARTESIAN_POINT('Ctrl Pts',(-2.01919259405809,1.,0.754682330722816));
#24621=CARTESIAN_POINT('Ctrl Pts',(-2.01288584328084,-1.,0.755642704957865));
#24622=CARTESIAN_POINT('Ctrl Pts',(-2.01288584328084,1.,0.755642704957865));
#24623=CARTESIAN_POINT('Ctrl Pts',(-2.0065843158773,-1.,0.75656290464667));
#24624=CARTESIAN_POINT('Ctrl Pts',(-2.0065843158773,1.,0.75656290464667));
#24625=CARTESIAN_POINT('Ctrl Pts',(-2.00028834739178,-1.,0.757442676862724));
#24626=CARTESIAN_POINT('Ctrl Pts',(-2.00028834739178,1.,0.757442676862724));
#24627=CARTESIAN_POINT('Ctrl Pts',(-1.99399831098817,-1.,0.758281796766761));
#24628=CARTESIAN_POINT('Ctrl Pts',(-1.99399831098817,1.,0.758281796766761));
#24629=CARTESIAN_POINT('Ctrl Pts',(-1.98771456680874,-1.,0.759080037802488));
#24630=CARTESIAN_POINT('Ctrl Pts',(-1.98771456680874,1.,0.759080037802488));
#24631=CARTESIAN_POINT('Ctrl Pts',(-1.98143741418172,-1.,0.75983714745219));
#24632=CARTESIAN_POINT('Ctrl Pts',(-1.98143741418172,1.,0.75983714745219));
#24633=CARTESIAN_POINT('Ctrl Pts',(-1.97516705321494,-1.,0.760552825409757));
#24634=CARTESIAN_POINT('Ctrl Pts',(-1.97516705321494,1.,0.760552825409757));
#24635=CARTESIAN_POINT('Ctrl Pts',(-1.96890351582499,-1.,0.76122669048382));
#24636=CARTESIAN_POINT('Ctrl Pts',(-1.96890351582499,1.,0.76122669048382));
#24637=CARTESIAN_POINT('Ctrl Pts',(-1.96264672744186,-1.,0.761858300014423));
#24638=CARTESIAN_POINT('Ctrl Pts',(-1.96264672744186,1.,0.761858300014423));
#24639=CARTESIAN_POINT('Ctrl Pts',(-1.95639665309869,-1.,0.762447203806179));
#24640=CARTESIAN_POINT('Ctrl Pts',(-1.95639665309869,1.,0.762447203806179));
#24641=CARTESIAN_POINT('Ctrl Pts',(-1.95015342590024,-1.,0.762992990878769));
#24642=CARTESIAN_POINT('Ctrl Pts',(-1.95015342590024,1.,0.762992990878769));
#24643=CARTESIAN_POINT('Ctrl Pts',(-1.9439174661764,-1.,0.763495333538629));
#24644=CARTESIAN_POINT('Ctrl Pts',(-1.9439174661764,1.,0.763495333538629));
#24645=CARTESIAN_POINT('Ctrl Pts',(-1.93768964875886,-1.,0.763954049121458));
#24646=CARTESIAN_POINT('Ctrl Pts',(-1.93768964875886,1.,0.763954049121458));
#24647=CARTESIAN_POINT('Ctrl Pts',(-1.93147105496382,-1.,0.76436901067394));
#24648=CARTESIAN_POINT('Ctrl Pts',(-1.93147105496382,1.,0.76436901067394));
#24649=CARTESIAN_POINT('Ctrl Pts',(-1.92526263537048,-1.,0.764740025488211));
#24650=CARTESIAN_POINT('Ctrl Pts',(-1.92526263537048,1.,0.764740025488211));
#24651=CARTESIAN_POINT('Ctrl Pts',(-1.91906491634196,-1.,0.765066729667088));
#24652=CARTESIAN_POINT('Ctrl Pts',(-1.91906491634196,1.,0.765066729667088));
#24653=CARTESIAN_POINT('Ctrl Pts',(-1.91287765805169,-1.,0.765348465884722));
#24654=CARTESIAN_POINT('Ctrl Pts',(-1.91287765805169,1.,0.765348465884722));
#24655=CARTESIAN_POINT('Ctrl Pts',(-1.90669961402356,-1.,0.765584196937919));
#24656=CARTESIAN_POINT('Ctrl Pts',(-1.90669961402356,1.,0.765584196937919));
#24657=CARTESIAN_POINT('Ctrl Pts',(-1.90052930393596,-1.,0.765772772593386));
#24658=CARTESIAN_POINT('Ctrl Pts',(-1.90052930393596,1.,0.765772772593386));
#24659=CARTESIAN_POINT('Ctrl Pts',(-1.89436577771388,-1.,0.765913193856978));
#24660=CARTESIAN_POINT('Ctrl Pts',(-1.89436577771388,1.,0.765913193856978));
#24661=CARTESIAN_POINT('Ctrl Pts',(-1.88820926433409,-1.,0.766004837062091));
#24662=CARTESIAN_POINT('Ctrl Pts',(-1.88820926433409,1.,0.766004837062091));
#24663=CARTESIAN_POINT('Ctrl Pts',(-1.88206215302561,-1.,0.766047794851864));
#24664=CARTESIAN_POINT('Ctrl Pts',(-1.88206215302561,1.,0.766047794851864));
#24665=CARTESIAN_POINT('Ctrl Pts',(-1.87592888967883,-1.,0.766042837036744));
#24666=CARTESIAN_POINT('Ctrl Pts',(-1.87592888967883,1.,0.766042837036744));
#24667=CARTESIAN_POINT('Ctrl Pts',(-1.86981398314341,-1.,0.765990708546091));
#24668=CARTESIAN_POINT('Ctrl Pts',(-1.86981398314341,1.,0.765990708546091));
#24669=CARTESIAN_POINT('Ctrl Pts',(-1.86372027063312,-1.,0.765891519092547));
#24670=CARTESIAN_POINT('Ctrl Pts',(-1.86372027063312,1.,0.765891519092547));
#24671=CARTESIAN_POINT('Ctrl Pts',(-1.85764741390394,-1.,0.765744212909318));
#24672=CARTESIAN_POINT('Ctrl Pts',(-1.85764741390394,1.,0.765744212909318));
#24673=CARTESIAN_POINT('Ctrl Pts',(-1.85158945130063,-1.,0.765545710619062));
#24674=CARTESIAN_POINT('Ctrl Pts',(-1.85158945130063,1.,0.765545710619062));
#24675=CARTESIAN_POINT('Ctrl Pts',(-1.84553698875924,-1.,0.765291664862029));
#24676=CARTESIAN_POINT('Ctrl Pts',(-1.84553698875924,1.,0.765291664862029));
#24677=CARTESIAN_POINT('Ctrl Pts',(-1.83948181064835,-1.,0.764978057881737));
#24678=CARTESIAN_POINT('Ctrl Pts',(-1.83948181064835,1.,0.764978057881737));
#24679=CARTESIAN_POINT('Ctrl Pts',(-1.83342077227142,-1.,0.764602549687853));
#24680=CARTESIAN_POINT('Ctrl Pts',(-1.83342077227142,1.,0.764602549687853));
#24681=CARTESIAN_POINT('Ctrl Pts',(-1.82735991200065,-1.,0.764165902605995));
#24682=CARTESIAN_POINT('Ctrl Pts',(-1.82735991200065,1.,0.764165902605995));
#24683=CARTESIAN_POINT('Ctrl Pts',(-1.82131873145266,-1.,0.763673465462726));
#24684=CARTESIAN_POINT('Ctrl Pts',(-1.82131873145266,1.,0.763673465462726));
#24685=CARTESIAN_POINT('Ctrl Pts',(-1.8153211840553,-1.,0.763132003836634));
#24686=CARTESIAN_POINT('Ctrl Pts',(-1.8153211840553,1.,0.763132003836634));
#24687=CARTESIAN_POINT('Ctrl Pts',(-1.80938551463965,-1.,0.762546129463938));
#24688=CARTESIAN_POINT('Ctrl Pts',(-1.80938551463965,1.,0.762546129463938));
#24689=CARTESIAN_POINT('Ctrl Pts',(-1.80351583877342,-1.,0.761915336443547));
#24690=CARTESIAN_POINT('Ctrl Pts',(-1.80351583877342,1.,0.761915336443547));
#24691=CARTESIAN_POINT('Ctrl Pts',(-1.79768986997783,-1.,0.761229695230558));
#24692=CARTESIAN_POINT('Ctrl Pts',(-1.79768986997783,1.,0.761229695230558));
#24693=CARTESIAN_POINT('Ctrl Pts',(-1.7918581561088,-1.,0.760469555880749));
#24694=CARTESIAN_POINT('Ctrl Pts',(-1.7918581561088,1.,0.760469555880749));
#24695=CARTESIAN_POINT('Ctrl Pts',(-1.78596964884604,-1.,0.759614401110189));
#24696=CARTESIAN_POINT('Ctrl Pts',(-1.78596964884604,1.,0.759614401110189));
#24697=CARTESIAN_POINT('Ctrl Pts',(-1.77999411220945,-1.,0.758650626677518));
#24698=CARTESIAN_POINT('Ctrl Pts',(-1.77999411220945,1.,0.758650626677518));
#24699=CARTESIAN_POINT('Ctrl Pts',(-1.77394167108292,-1.,0.757578264077029));
#24700=CARTESIAN_POINT('Ctrl Pts',(-1.77394167108292,1.,0.757578264077029));
#24701=CARTESIAN_POINT('Ctrl Pts',(-1.76789396002998,-1.,0.75642189602781));
#24702=CARTESIAN_POINT('Ctrl Pts',(-1.76789396002998,1.,0.75642189602781));
#24703=CARTESIAN_POINT('Ctrl Pts',(-1.76197817240128,-1.,0.755220979974461));
#24704=CARTESIAN_POINT('Ctrl Pts',(-1.76197817240128,1.,0.755220979974461));
#24705=CARTESIAN_POINT('Ctrl Pts',(-1.75631083600019,-1.,0.754009254027829));
#24706=CARTESIAN_POINT('Ctrl Pts',(-1.75631083600019,1.,0.754009254027829));
#24707=CARTESIAN_POINT('Ctrl Pts',(-1.75095139468794,-1.,0.752797683531314));
#24708=CARTESIAN_POINT('Ctrl Pts',(-1.75095139468794,1.,0.752797683531314));
#24709=CARTESIAN_POINT('Ctrl Pts',(-1.74585086852502,-1.,0.751555614164482));
#24710=CARTESIAN_POINT('Ctrl Pts',(-1.74585086852502,1.,0.751555614164482));
#24711=CARTESIAN_POINT('Ctrl Pts',(-1.74080458267114,-1.,0.750193435981249));
#24712=CARTESIAN_POINT('Ctrl Pts',(-1.74080458267114,1.,0.750193435981249));
#24713=CARTESIAN_POINT('Ctrl Pts',(-1.7355035168033,-1.,0.74858246295687));
#24714=CARTESIAN_POINT('Ctrl Pts',(-1.7355035168033,1.,0.74858246295687));
#24715=CARTESIAN_POINT('Ctrl Pts',(-1.72958533647714,-1.,0.746574710097752));
#24716=CARTESIAN_POINT('Ctrl Pts',(-1.72958533647714,1.,0.746574710097752));
#24717=CARTESIAN_POINT('Ctrl Pts',(-1.72268229916769,-1.,0.744021445433093));
#24718=CARTESIAN_POINT('Ctrl Pts',(-1.72268229916769,1.,0.744021445433093));
#24719=CARTESIAN_POINT('Ctrl Pts',(-1.71447789751001,-1.,0.74079516202821));
#24720=CARTESIAN_POINT('Ctrl Pts',(-1.71447789751001,1.,0.74079516202821));
#24721=CARTESIAN_POINT('Ctrl Pts',(-1.70473309004249,-1.,0.736799665716932));
#24722=CARTESIAN_POINT('Ctrl Pts',(-1.70473309004249,1.,0.736799665716932));
#24723=CARTESIAN_POINT('Ctrl Pts',(-1.69326921972915,-1.,0.731963238685357));
#24724=CARTESIAN_POINT('Ctrl Pts',(-1.69326921972915,1.,0.731963238685357));
#24725=CARTESIAN_POINT('Ctrl Pts',(-1.67996158451922,-1.,0.726235967982445));
#24726=CARTESIAN_POINT('Ctrl Pts',(-1.67996158451922,1.,0.726235967982445));
#24727=CARTESIAN_POINT('Ctrl Pts',(-1.66472880551777,-1.,0.71958543378795));
#24728=CARTESIAN_POINT('Ctrl Pts',(-1.66472880551777,1.,0.71958543378795));
#24729=CARTESIAN_POINT('Ctrl Pts',(-1.64752408828442,-1.,0.711993139340447));
#24730=CARTESIAN_POINT('Ctrl Pts',(-1.64752408828442,1.,0.711993139340447));
#24731=CARTESIAN_POINT('Ctrl Pts',(-1.6321654166204,-1.,0.705159151977294));
#24732=CARTESIAN_POINT('Ctrl Pts',(-1.6321654166204,1.,0.705159151977294));
#24733=CARTESIAN_POINT('Ctrl Pts',(-1.61974673471117,-1.,0.699605146398837));
#24734=CARTESIAN_POINT('Ctrl Pts',(-1.61974673471117,1.,0.699605146398837));
#24735=CARTESIAN_POINT('Ctrl Pts',(-1.61106790957619,-1.,0.69571209787897));
#24736=CARTESIAN_POINT('Ctrl Pts',(-1.61106790957619,1.,0.69571209787897));
#24737=CARTESIAN_POINT('Ctrl Pts',(-1.60662857109684,-1.,0.693717979106305));
#24738=CARTESIAN_POINT('Ctrl Pts',(-1.60662857109684,1.,0.693717979106305));
#24739=CARTESIAN_POINT('',(-2.0698113262342,1.,0.7455743247944));
#24740=CARTESIAN_POINT('Ctrl Pts',(-2.0698113262342,1.,0.7455743247944));
#24741=CARTESIAN_POINT('Ctrl Pts',(-2.06854248895728,1.,0.745832791378367));
#24742=CARTESIAN_POINT('Ctrl Pts',(-2.06600523016815,1.,0.7463458715442));
#24743=CARTESIAN_POINT('Ctrl Pts',(-2.06220058927826,1.,0.747103932787919));
#24744=CARTESIAN_POINT('Ctrl Pts',(-2.05713023031006,1.,0.748091554183802));
#24745=CARTESIAN_POINT('Ctrl Pts',(-2.05079645592154,1.,0.749287468665046));
#24746=CARTESIAN_POINT('Ctrl Pts',(-2.04446689147979,1.,0.750444657875576));
#24747=CARTESIAN_POINT('Ctrl Pts',(-2.03814160092099,1.,0.751562963361115));
#24748=CARTESIAN_POINT('Ctrl Pts',(-2.03182068456221,1.,0.752642180487211));
#24749=CARTESIAN_POINT('Ctrl Pts',(-2.02550428623313,1.,0.753682061112768));
#24750=CARTESIAN_POINT('Ctrl Pts',(-2.01919259405809,1.,0.754682330722816));
#24751=CARTESIAN_POINT('Ctrl Pts',(-2.01288584328084,1.,0.755642704957865));
#24752=CARTESIAN_POINT('Ctrl Pts',(-2.0065843158773,1.,0.75656290464667));
#24753=CARTESIAN_POINT('Ctrl Pts',(-2.00028834739178,1.,0.757442676862724));
#24754=CARTESIAN_POINT('Ctrl Pts',(-1.99399831098817,1.,0.758281796766761));
#24755=CARTESIAN_POINT('Ctrl Pts',(-1.98771456680874,1.,0.759080037802488));
#24756=CARTESIAN_POINT('Ctrl Pts',(-1.98143741418172,1.,0.75983714745219));
#24757=CARTESIAN_POINT('Ctrl Pts',(-1.97516705321494,1.,0.760552825409757));
#24758=CARTESIAN_POINT('Ctrl Pts',(-1.96890351582499,1.,0.76122669048382));
#24759=CARTESIAN_POINT('Ctrl Pts',(-1.96264672744186,1.,0.761858300014423));
#24760=CARTESIAN_POINT('Ctrl Pts',(-1.95639665309869,1.,0.762447203806179));
#24761=CARTESIAN_POINT('Ctrl Pts',(-1.95015342590024,1.,0.762992990878769));
#24762=CARTESIAN_POINT('Ctrl Pts',(-1.9439174661764,1.,0.763495333538629));
#24763=CARTESIAN_POINT('Ctrl Pts',(-1.93768964875886,1.,0.763954049121458));
#24764=CARTESIAN_POINT('Ctrl Pts',(-1.93147105496382,1.,0.76436901067394));
#24765=CARTESIAN_POINT('Ctrl Pts',(-1.92526263537048,1.,0.764740025488211));
#24766=CARTESIAN_POINT('Ctrl Pts',(-1.91906491634196,1.,0.765066729667088));
#24767=CARTESIAN_POINT('Ctrl Pts',(-1.91287765805169,1.,0.765348465884722));
#24768=CARTESIAN_POINT('Ctrl Pts',(-1.90669961402356,1.,0.765584196937919));
#24769=CARTESIAN_POINT('Ctrl Pts',(-1.90052930393596,1.,0.765772772593386));
#24770=CARTESIAN_POINT('Ctrl Pts',(-1.89436577771388,1.,0.765913193856978));
#24771=CARTESIAN_POINT('Ctrl Pts',(-1.88820926433409,1.,0.766004837062091));
#24772=CARTESIAN_POINT('Ctrl Pts',(-1.88206215302561,1.,0.766047794851864));
#24773=CARTESIAN_POINT('Ctrl Pts',(-1.87592888967883,1.,0.766042837036744));
#24774=CARTESIAN_POINT('Ctrl Pts',(-1.86981398314341,1.,0.765990708546091));
#24775=CARTESIAN_POINT('Ctrl Pts',(-1.86372027063312,1.,0.765891519092547));
#24776=CARTESIAN_POINT('Ctrl Pts',(-1.85764741390394,1.,0.765744212909318));
#24777=CARTESIAN_POINT('Ctrl Pts',(-1.85158945130063,1.,0.765545710619062));
#24778=CARTESIAN_POINT('Ctrl Pts',(-1.84553698875924,1.,0.765291664862029));
#24779=CARTESIAN_POINT('Ctrl Pts',(-1.83948181064835,1.,0.764978057881737));
#24780=CARTESIAN_POINT('Ctrl Pts',(-1.83342077227142,1.,0.764602549687853));
#24781=CARTESIAN_POINT('Ctrl Pts',(-1.82735991200065,1.,0.764165902605995));
#24782=CARTESIAN_POINT('Ctrl Pts',(-1.82131873145266,1.,0.763673465462726));
#24783=CARTESIAN_POINT('Ctrl Pts',(-1.8153211840553,1.,0.763132003836634));
#24784=CARTESIAN_POINT('Ctrl Pts',(-1.80938551463965,1.,0.762546129463938));
#24785=CARTESIAN_POINT('Ctrl Pts',(-1.80351583877342,1.,0.761915336443547));
#24786=CARTESIAN_POINT('Ctrl Pts',(-1.79768986997783,1.,0.761229695230558));
#24787=CARTESIAN_POINT('Ctrl Pts',(-1.7918581561088,1.,0.760469555880749));
#24788=CARTESIAN_POINT('Ctrl Pts',(-1.78596964884604,1.,0.759614401110189));
#24789=CARTESIAN_POINT('Ctrl Pts',(-1.77999411220945,1.,0.758650626677518));
#24790=CARTESIAN_POINT('Ctrl Pts',(-1.77394167108292,1.,0.757578264077029));
#24791=CARTESIAN_POINT('Ctrl Pts',(-1.76789396002998,1.,0.75642189602781));
#24792=CARTESIAN_POINT('Ctrl Pts',(-1.76197817240128,1.,0.755220979974461));
#24793=CARTESIAN_POINT('Ctrl Pts',(-1.75631083600019,1.,0.754009254027829));
#24794=CARTESIAN_POINT('Ctrl Pts',(-1.75095139468794,1.,0.752797683531314));
#24795=CARTESIAN_POINT('Ctrl Pts',(-1.74585086852502,1.,0.751555614164482));
#24796=CARTESIAN_POINT('Ctrl Pts',(-1.74080458267114,1.,0.750193435981249));
#24797=CARTESIAN_POINT('Ctrl Pts',(-1.7355035168033,1.,0.74858246295687));
#24798=CARTESIAN_POINT('Ctrl Pts',(-1.72958533647714,1.,0.746574710097752));
#24799=CARTESIAN_POINT('Ctrl Pts',(-1.72268229916769,1.,0.744021445433093));
#24800=CARTESIAN_POINT('Ctrl Pts',(-1.71447789751001,1.,0.74079516202821));
#24801=CARTESIAN_POINT('Ctrl Pts',(-1.70473309004249,1.,0.736799665716932));
#24802=CARTESIAN_POINT('Ctrl Pts',(-1.69326921972915,1.,0.731963238685357));
#24803=CARTESIAN_POINT('Ctrl Pts',(-1.67996158451922,1.,0.726235967982445));
#24804=CARTESIAN_POINT('Ctrl Pts',(-1.66472880551777,1.,0.71958543378795));
#24805=CARTESIAN_POINT('Ctrl Pts',(-1.64752408828442,1.,0.711993139340447));
#24806=CARTESIAN_POINT('Ctrl Pts',(-1.6321654166204,1.,0.705159151977294));
#24807=CARTESIAN_POINT('Ctrl Pts',(-1.61974673471117,1.,0.699605146398837));
#24808=CARTESIAN_POINT('Ctrl Pts',(-1.61106790957619,1.,0.69571209787897));
#24809=CARTESIAN_POINT('Ctrl Pts',(-1.60662857109684,1.,0.693717979106305));
#24810=CARTESIAN_POINT('',(-2.0698113262342,0.,0.7455743247944));
#24811=CARTESIAN_POINT('Origin',(-2.11275013067528,0.,0.61342227326009));
#24812=CARTESIAN_POINT('',(-2.11275013067528,1.,0.61342227326009));
#24813=CARTESIAN_POINT('',(-2.0698113262342,1.,0.7455743247944));
#24814=CARTESIAN_POINT('',(-2.11275013067528,0.,0.61342227326009));
#24815=CARTESIAN_POINT('Ctrl Pts',(-1.7075470150345,-1.,0.383122945602004));
#24816=CARTESIAN_POINT('Ctrl Pts',(-1.7075470150345,1.,0.383122945602004));
#24817=CARTESIAN_POINT('Ctrl Pts',(-1.71231062891958,-1.,0.384119047315542));
#24818=CARTESIAN_POINT('Ctrl Pts',(-1.71231062891958,1.,0.384119047315542));
#24819=CARTESIAN_POINT('Ctrl Pts',(-1.72162022246158,-1.,0.38607079032701));
#24820=CARTESIAN_POINT('Ctrl Pts',(-1.72162022246158,1.,0.38607079032701));
#24821=CARTESIAN_POINT('Ctrl Pts',(-1.7349317097561,-1.,0.388877023509191));
#24822=CARTESIAN_POINT('Ctrl Pts',(-1.7349317097561,1.,0.388877023509191));
#24823=CARTESIAN_POINT('Ctrl Pts',(-1.75137405313962,-1.,0.392375812294307));
#24824=CARTESIAN_POINT('Ctrl Pts',(-1.75137405313962,1.,0.392375812294307));
#24825=CARTESIAN_POINT('Ctrl Pts',(-1.7697556004756,-1.,0.39634619612042));
#24826=CARTESIAN_POINT('Ctrl Pts',(-1.7697556004756,1.,0.39634619612042));
#24827=CARTESIAN_POINT('Ctrl Pts',(-1.78598826347533,-1.,0.39991940378308));
#24828=CARTESIAN_POINT('Ctrl Pts',(-1.78598826347533,1.,0.39991940378308));
#24829=CARTESIAN_POINT('Ctrl Pts',(-1.80012077176221,-1.,0.403107976170441));
#24830=CARTESIAN_POINT('Ctrl Pts',(-1.80012077176221,1.,0.403107976170441));
#24831=CARTESIAN_POINT('Ctrl Pts',(-1.81223801813988,-1.,0.405933518411838));
#24832=CARTESIAN_POINT('Ctrl Pts',(-1.81223801813988,1.,0.405933518411838));
#24833=CARTESIAN_POINT('Ctrl Pts',(-1.8224702267854,-1.,0.408428948108533));
#24834=CARTESIAN_POINT('Ctrl Pts',(-1.8224702267854,1.,0.408428948108533));
#24835=CARTESIAN_POINT('Ctrl Pts',(-1.83100408895216,-1.,0.410641256301675));
#24836=CARTESIAN_POINT('Ctrl Pts',(-1.83100408895216,1.,0.410641256301675));
#24837=CARTESIAN_POINT('Ctrl Pts',(-1.83808953475839,-1.,0.412633125322161));
#24838=CARTESIAN_POINT('Ctrl Pts',(-1.83808953475839,1.,0.412633125322161));
#24839=CARTESIAN_POINT('Ctrl Pts',(-1.8440575707371,-1.,0.41448743825434));
#24840=CARTESIAN_POINT('Ctrl Pts',(-1.8440575707371,1.,0.41448743825434));
#24841=CARTESIAN_POINT('Ctrl Pts',(-1.84929312929882,-1.,0.416300022038864));
#24842=CARTESIAN_POINT('Ctrl Pts',(-1.84929312929882,1.,0.416300022038864));
#24843=CARTESIAN_POINT('Ctrl Pts',(-1.85417632856234,-1.,0.418164129143534));
#24844=CARTESIAN_POINT('Ctrl Pts',(-1.85417632856234,1.,0.418164129143534));
#24845=CARTESIAN_POINT('Ctrl Pts',(-1.85903281096686,-1.,0.420157287975619));
#24846=CARTESIAN_POINT('Ctrl Pts',(-1.85903281096686,1.,0.420157287975619));
#24847=CARTESIAN_POINT('Ctrl Pts',(-1.86408083334028,-1.,0.422327307418275));
#24848=CARTESIAN_POINT('Ctrl Pts',(-1.86408083334028,1.,0.422327307418275));
#24849=CARTESIAN_POINT('Ctrl Pts',(-1.86937803944323,-1.,0.424678177291359));
#24850=CARTESIAN_POINT('Ctrl Pts',(-1.86937803944323,1.,0.424678177291359));
#24851=CARTESIAN_POINT('Ctrl Pts',(-1.87486989291484,-1.,0.427183828519102));
#24852=CARTESIAN_POINT('Ctrl Pts',(-1.87486989291484,1.,0.427183828519102));
#24853=CARTESIAN_POINT('Ctrl Pts',(-1.88044229001832,-1.,0.429803062482344));
#24854=CARTESIAN_POINT('Ctrl Pts',(-1.88044229001832,1.,0.429803062482344));
#24855=CARTESIAN_POINT('Ctrl Pts',(-1.88596913666793,-1.,0.432493038548748));
#24856=CARTESIAN_POINT('Ctrl Pts',(-1.88596913666793,1.,0.432493038548748));
#24857=CARTESIAN_POINT('Ctrl Pts',(-1.89136993975504,-1.,0.435225660963383));
#24858=CARTESIAN_POINT('Ctrl Pts',(-1.89136993975504,1.,0.435225660963383));
#24859=CARTESIAN_POINT('Ctrl Pts',(-1.89663648956466,-1.,0.437995003948244));
#24860=CARTESIAN_POINT('Ctrl Pts',(-1.89663648956466,1.,0.437995003948244));
#24861=CARTESIAN_POINT('Ctrl Pts',(-1.90180124389086,-1.,0.440807833704038));
#24862=CARTESIAN_POINT('Ctrl Pts',(-1.90180124389086,1.,0.440807833704038));
#24863=CARTESIAN_POINT('Ctrl Pts',(-1.90691756144898,-1.,0.44367755684915));
#24864=CARTESIAN_POINT('Ctrl Pts',(-1.90691756144898,1.,0.44367755684915));
#24865=CARTESIAN_POINT('Ctrl Pts',(-1.9120369998112,-1.,0.446617343485711));
#24866=CARTESIAN_POINT('Ctrl Pts',(-1.9120369998112,1.,0.446617343485711));
#24867=CARTESIAN_POINT('Ctrl Pts',(-1.91718342555755,-1.,0.449632260106662));
#24868=CARTESIAN_POINT('Ctrl Pts',(-1.91718342555755,1.,0.449632260106662));
#24869=CARTESIAN_POINT('Ctrl Pts',(-1.92235380648502,-1.,0.452719478359432));
#24870=CARTESIAN_POINT('Ctrl Pts',(-1.92235380648502,1.,0.452719478359432));
#24871=CARTESIAN_POINT('Ctrl Pts',(-1.92753067150476,-1.,0.455872005174371));
#24872=CARTESIAN_POINT('Ctrl Pts',(-1.92753067150476,1.,0.455872005174371));
#24873=CARTESIAN_POINT('Ctrl Pts',(-1.93269066517934,-1.,0.459081234547926));
#24874=CARTESIAN_POINT('Ctrl Pts',(-1.93269066517934,1.,0.459081234547926));
#24875=CARTESIAN_POINT('Ctrl Pts',(-1.93781486640821,-1.,0.462340031009056));
#24876=CARTESIAN_POINT('Ctrl Pts',(-1.93781486640821,1.,0.462340031009056));
#24877=CARTESIAN_POINT('Ctrl Pts',(-1.9428979419619,-1.,0.46564546202603));
#24878=CARTESIAN_POINT('Ctrl Pts',(-1.9428979419619,1.,0.46564546202603));
#24879=CARTESIAN_POINT('Ctrl Pts',(-1.94794381136514,-1.,0.468997482913135));
#24880=CARTESIAN_POINT('Ctrl Pts',(-1.94794381136514,1.,0.468997482913135));
#24881=CARTESIAN_POINT('Ctrl Pts',(-1.95296148278133,-1.,0.472397672264072));
#24882=CARTESIAN_POINT('Ctrl Pts',(-1.95296148278133,1.,0.472397672264072));
#24883=CARTESIAN_POINT('Ctrl Pts',(-1.95796111148177,-1.,0.475848034683176));
#24884=CARTESIAN_POINT('Ctrl Pts',(-1.95796111148177,1.,0.475848034683176));
#24885=CARTESIAN_POINT('Ctrl Pts',(-1.96294933055943,-1.,0.479349583074855));
#24886=CARTESIAN_POINT('Ctrl Pts',(-1.96294933055943,1.,0.479349583074855));
#24887=CARTESIAN_POINT('Ctrl Pts',(-1.96792703422362,-1.,0.48290166212069));
#24888=CARTESIAN_POINT('Ctrl Pts',(-1.96792703422362,1.,0.48290166212069));
#24889=CARTESIAN_POINT('Ctrl Pts',(-1.97289186263272,-1.,0.486502692907659));
#24890=CARTESIAN_POINT('Ctrl Pts',(-1.97289186263272,1.,0.486502692907659));
#24891=CARTESIAN_POINT('Ctrl Pts',(-1.97783973019229,-1.,0.490150627860952));
#24892=CARTESIAN_POINT('Ctrl Pts',(-1.97783973019229,1.,0.490150627860952));
#24893=CARTESIAN_POINT('Ctrl Pts',(-1.98276658761821,-1.,0.493843476541494));
#24894=CARTESIAN_POINT('Ctrl Pts',(-1.98276658761821,1.,0.493843476541494));
#24895=CARTESIAN_POINT('Ctrl Pts',(-1.98767044752932,-1.,0.497579909545574));
#24896=CARTESIAN_POINT('Ctrl Pts',(-1.98767044752932,1.,0.497579909545574));
#24897=CARTESIAN_POINT('Ctrl Pts',(-1.99255149126155,-1.,0.501359287727146));
#24898=CARTESIAN_POINT('Ctrl Pts',(-1.99255149126155,1.,0.501359287727146));
#24899=CARTESIAN_POINT('Ctrl Pts',(-1.99741107463572,-1.,0.505181361323026));
#24900=CARTESIAN_POINT('Ctrl Pts',(-1.99741107463572,1.,0.505181361323026));
#24901=CARTESIAN_POINT('Ctrl Pts',(-2.00225107134734,-1.,0.509046069886157));
#24902=CARTESIAN_POINT('Ctrl Pts',(-2.00225107134734,1.,0.509046069886157));
#24903=CARTESIAN_POINT('Ctrl Pts',(-2.00707309946949,-1.,0.512953306961792));
#24904=CARTESIAN_POINT('Ctrl Pts',(-2.00707309946949,1.,0.512953306961792));
#24905=CARTESIAN_POINT('Ctrl Pts',(-2.01187773939242,-1.,0.516902681728687));
#24906=CARTESIAN_POINT('Ctrl Pts',(-2.01187773939242,1.,0.516902681728687));
#24907=CARTESIAN_POINT('Ctrl Pts',(-2.01666477917286,-1.,0.52089359039937));
#24908=CARTESIAN_POINT('Ctrl Pts',(-2.01666477917286,1.,0.52089359039937));
#24909=CARTESIAN_POINT('Ctrl Pts',(-2.02143356304698,-1.,0.524925318333476));
#24910=CARTESIAN_POINT('Ctrl Pts',(-2.02143356304698,1.,0.524925318333476));
#24911=CARTESIAN_POINT('Ctrl Pts',(-2.0261832908329,-1.,0.528997127241914));
#24912=CARTESIAN_POINT('Ctrl Pts',(-2.0261832908329,1.,0.528997127241914));
#24913=CARTESIAN_POINT('Ctrl Pts',(-2.03091336214426,-1.,0.533108355132976));
#24914=CARTESIAN_POINT('Ctrl Pts',(-2.03091336214426,1.,0.533108355132976));
#24915=CARTESIAN_POINT('Ctrl Pts',(-2.03562362954037,-1.,0.537258489833262));
#24916=CARTESIAN_POINT('Ctrl Pts',(-2.03562362954037,1.,0.537258489833262));
#24917=CARTESIAN_POINT('Ctrl Pts',(-2.04031422690527,-1.,0.541447120615659));
#24918=CARTESIAN_POINT('Ctrl Pts',(-2.04031422690527,1.,0.541447120615659));
#24919=CARTESIAN_POINT('Ctrl Pts',(-2.04498544714588,-1.,0.54567390381743));
#24920=CARTESIAN_POINT('Ctrl Pts',(-2.04498544714588,1.,0.54567390381743));
#24921=CARTESIAN_POINT('Ctrl Pts',(-2.04963761077958,-1.,0.549938525150295));
#24922=CARTESIAN_POINT('Ctrl Pts',(-2.04963761077958,1.,0.549938525150295));
#24923=CARTESIAN_POINT('Ctrl Pts',(-2.05427091604413,-1.,0.554240657463906));
#24924=CARTESIAN_POINT('Ctrl Pts',(-2.05427091604413,1.,0.554240657463906));
#24925=CARTESIAN_POINT('Ctrl Pts',(-2.05888537756462,-1.,0.558579940185151));
#24926=CARTESIAN_POINT('Ctrl Pts',(-2.05888537756462,1.,0.558579940185151));
#24927=CARTESIAN_POINT('Ctrl Pts',(-2.06348090160589,-1.,0.562955993082261));
#24928=CARTESIAN_POINT('Ctrl Pts',(-2.06348090160589,1.,0.562955993082261));
#24929=CARTESIAN_POINT('Ctrl Pts',(-2.06805732997334,-1.,0.567368421181087));
#24930=CARTESIAN_POINT('Ctrl Pts',(-2.06805732997334,1.,0.567368421181087));
#24931=CARTESIAN_POINT('Ctrl Pts',(-2.07261449292824,-1.,0.571816823242603));
#24932=CARTESIAN_POINT('Ctrl Pts',(-2.07261449292824,1.,0.571816823242603));
#24933=CARTESIAN_POINT('Ctrl Pts',(-2.07715226767559,-1.,0.576300797416844));
#24934=CARTESIAN_POINT('Ctrl Pts',(-2.07715226767559,1.,0.576300797416844));
#24935=CARTESIAN_POINT('Ctrl Pts',(-2.08167059018418,-1.,0.580819952108063));
#24936=CARTESIAN_POINT('Ctrl Pts',(-2.08167059018418,1.,0.580819952108063));
#24937=CARTESIAN_POINT('Ctrl Pts',(-2.08616943727951,-1.,0.585373918991617));
#24938=CARTESIAN_POINT('Ctrl Pts',(-2.08616943727951,1.,0.585373918991617));
#24939=CARTESIAN_POINT('Ctrl Pts',(-2.09064881812129,-1.,0.589962365403406));
#24940=CARTESIAN_POINT('Ctrl Pts',(-2.09064881812129,1.,0.589962365403406));
#24941=CARTESIAN_POINT('Ctrl Pts',(-2.0951087622027,-1.,0.594585006052162));
#24942=CARTESIAN_POINT('Ctrl Pts',(-2.0951087622027,1.,0.594585006052162));
#24943=CARTESIAN_POINT('Ctrl Pts',(-2.0995493086477,-1.,0.599241616420533));
#24944=CARTESIAN_POINT('Ctrl Pts',(-2.0995493086477,1.,0.599241616420533));
#24945=CARTESIAN_POINT('Ctrl Pts',(-2.10397049886949,-1.,0.60393203073603));
#24946=CARTESIAN_POINT('Ctrl Pts',(-2.10397049886949,1.,0.60393203073603));
#24947=CARTESIAN_POINT('Ctrl Pts',(-2.1074919961518,-1.,0.607711315454876));
#24948=CARTESIAN_POINT('Ctrl Pts',(-2.1074919961518,1.,0.607711315454876));
#24949=CARTESIAN_POINT('Ctrl Pts',(-2.11012443807238,-1.,0.610560911689899));
#24950=CARTESIAN_POINT('Ctrl Pts',(-2.11012443807238,1.,0.610560911689899));
#24951=CARTESIAN_POINT('Ctrl Pts',(-2.11187554259986,-1.,0.6124673655618));
#24952=CARTESIAN_POINT('Ctrl Pts',(-2.11187554259986,1.,0.6124673655618));
#24953=CARTESIAN_POINT('Ctrl Pts',(-2.11275013067528,-1.,0.61342227326009));
#24954=CARTESIAN_POINT('Ctrl Pts',(-2.11275013067528,1.,0.61342227326009));
#24955=CARTESIAN_POINT('',(-1.7075470150345,1.,0.383122945602004));
#24956=CARTESIAN_POINT('Ctrl Pts',(-1.7075470150345,1.,0.383122945602004));
#24957=CARTESIAN_POINT('Ctrl Pts',(-1.71231062891958,1.,0.384119047315542));
#24958=CARTESIAN_POINT('Ctrl Pts',(-1.72162022246158,1.,0.38607079032701));
#24959=CARTESIAN_POINT('Ctrl Pts',(-1.7349317097561,1.,0.388877023509191));
#24960=CARTESIAN_POINT('Ctrl Pts',(-1.75137405313962,1.,0.392375812294307));
#24961=CARTESIAN_POINT('Ctrl Pts',(-1.7697556004756,1.,0.39634619612042));
#24962=CARTESIAN_POINT('Ctrl Pts',(-1.78598826347533,1.,0.39991940378308));
#24963=CARTESIAN_POINT('Ctrl Pts',(-1.80012077176221,1.,0.403107976170441));
#24964=CARTESIAN_POINT('Ctrl Pts',(-1.81223801813988,1.,0.405933518411838));
#24965=CARTESIAN_POINT('Ctrl Pts',(-1.8224702267854,1.,0.408428948108533));
#24966=CARTESIAN_POINT('Ctrl Pts',(-1.83100408895216,1.,0.410641256301675));
#24967=CARTESIAN_POINT('Ctrl Pts',(-1.83808953475839,1.,0.412633125322161));
#24968=CARTESIAN_POINT('Ctrl Pts',(-1.8440575707371,1.,0.41448743825434));
#24969=CARTESIAN_POINT('Ctrl Pts',(-1.84929312929882,1.,0.416300022038864));
#24970=CARTESIAN_POINT('Ctrl Pts',(-1.85417632856234,1.,0.418164129143534));
#24971=CARTESIAN_POINT('Ctrl Pts',(-1.85903281096686,1.,0.420157287975619));
#24972=CARTESIAN_POINT('Ctrl Pts',(-1.86408083334028,1.,0.422327307418275));
#24973=CARTESIAN_POINT('Ctrl Pts',(-1.86937803944323,1.,0.424678177291359));
#24974=CARTESIAN_POINT('Ctrl Pts',(-1.87486989291484,1.,0.427183828519102));
#24975=CARTESIAN_POINT('Ctrl Pts',(-1.88044229001832,1.,0.429803062482344));
#24976=CARTESIAN_POINT('Ctrl Pts',(-1.88596913666793,1.,0.432493038548748));
#24977=CARTESIAN_POINT('Ctrl Pts',(-1.89136993975504,1.,0.435225660963383));
#24978=CARTESIAN_POINT('Ctrl Pts',(-1.89663648956466,1.,0.437995003948244));
#24979=CARTESIAN_POINT('Ctrl Pts',(-1.90180124389086,1.,0.440807833704038));
#24980=CARTESIAN_POINT('Ctrl Pts',(-1.90691756144898,1.,0.44367755684915));
#24981=CARTESIAN_POINT('Ctrl Pts',(-1.9120369998112,1.,0.446617343485711));
#24982=CARTESIAN_POINT('Ctrl Pts',(-1.91718342555755,1.,0.449632260106662));
#24983=CARTESIAN_POINT('Ctrl Pts',(-1.92235380648502,1.,0.452719478359432));
#24984=CARTESIAN_POINT('Ctrl Pts',(-1.92753067150476,1.,0.455872005174371));
#24985=CARTESIAN_POINT('Ctrl Pts',(-1.93269066517934,1.,0.459081234547926));
#24986=CARTESIAN_POINT('Ctrl Pts',(-1.93781486640821,1.,0.462340031009056));
#24987=CARTESIAN_POINT('Ctrl Pts',(-1.9428979419619,1.,0.46564546202603));
#24988=CARTESIAN_POINT('Ctrl Pts',(-1.94794381136514,1.,0.468997482913135));
#24989=CARTESIAN_POINT('Ctrl Pts',(-1.95296148278133,1.,0.472397672264072));
#24990=CARTESIAN_POINT('Ctrl Pts',(-1.95796111148177,1.,0.475848034683176));
#24991=CARTESIAN_POINT('Ctrl Pts',(-1.96294933055943,1.,0.479349583074855));
#24992=CARTESIAN_POINT('Ctrl Pts',(-1.96792703422362,1.,0.48290166212069));
#24993=CARTESIAN_POINT('Ctrl Pts',(-1.97289186263272,1.,0.486502692907659));
#24994=CARTESIAN_POINT('Ctrl Pts',(-1.97783973019229,1.,0.490150627860952));
#24995=CARTESIAN_POINT('Ctrl Pts',(-1.98276658761821,1.,0.493843476541494));
#24996=CARTESIAN_POINT('Ctrl Pts',(-1.98767044752932,1.,0.497579909545574));
#24997=CARTESIAN_POINT('Ctrl Pts',(-1.99255149126155,1.,0.501359287727146));
#24998=CARTESIAN_POINT('Ctrl Pts',(-1.99741107463572,1.,0.505181361323026));
#24999=CARTESIAN_POINT('Ctrl Pts',(-2.00225107134734,1.,0.509046069886157));
#25000=CARTESIAN_POINT('Ctrl Pts',(-2.00707309946949,1.,0.512953306961792));
#25001=CARTESIAN_POINT('Ctrl Pts',(-2.01187773939242,1.,0.516902681728687));
#25002=CARTESIAN_POINT('Ctrl Pts',(-2.01666477917286,1.,0.52089359039937));
#25003=CARTESIAN_POINT('Ctrl Pts',(-2.02143356304698,1.,0.524925318333476));
#25004=CARTESIAN_POINT('Ctrl Pts',(-2.0261832908329,1.,0.528997127241914));
#25005=CARTESIAN_POINT('Ctrl Pts',(-2.03091336214426,1.,0.533108355132976));
#25006=CARTESIAN_POINT('Ctrl Pts',(-2.03562362954037,1.,0.537258489833262));
#25007=CARTESIAN_POINT('Ctrl Pts',(-2.04031422690527,1.,0.541447120615659));
#25008=CARTESIAN_POINT('Ctrl Pts',(-2.04498544714588,1.,0.54567390381743));
#25009=CARTESIAN_POINT('Ctrl Pts',(-2.04963761077958,1.,0.549938525150295));
#25010=CARTESIAN_POINT('Ctrl Pts',(-2.05427091604413,1.,0.554240657463906));
#25011=CARTESIAN_POINT('Ctrl Pts',(-2.05888537756462,1.,0.558579940185151));
#25012=CARTESIAN_POINT('Ctrl Pts',(-2.06348090160589,1.,0.562955993082261));
#25013=CARTESIAN_POINT('Ctrl Pts',(-2.06805732997334,1.,0.567368421181087));
#25014=CARTESIAN_POINT('Ctrl Pts',(-2.07261449292824,1.,0.571816823242603));
#25015=CARTESIAN_POINT('Ctrl Pts',(-2.07715226767559,1.,0.576300797416844));
#25016=CARTESIAN_POINT('Ctrl Pts',(-2.08167059018418,1.,0.580819952108063));
#25017=CARTESIAN_POINT('Ctrl Pts',(-2.08616943727951,1.,0.585373918991617));
#25018=CARTESIAN_POINT('Ctrl Pts',(-2.09064881812129,1.,0.589962365403406));
#25019=CARTESIAN_POINT('Ctrl Pts',(-2.0951087622027,1.,0.594585006052162));
#25020=CARTESIAN_POINT('Ctrl Pts',(-2.0995493086477,1.,0.599241616420533));
#25021=CARTESIAN_POINT('Ctrl Pts',(-2.10397049886949,1.,0.60393203073603));
#25022=CARTESIAN_POINT('Ctrl Pts',(-2.1074919961518,1.,0.607711315454876));
#25023=CARTESIAN_POINT('Ctrl Pts',(-2.11012443807238,1.,0.610560911689899));
#25024=CARTESIAN_POINT('Ctrl Pts',(-2.11187554259986,1.,0.6124673655618));
#25025=CARTESIAN_POINT('Ctrl Pts',(-2.11275013067528,1.,0.61342227326009));
#25026=CARTESIAN_POINT('',(-1.7075470150345,0.,0.383122945602003));
#25027=CARTESIAN_POINT('Origin',(0.,0.,0.));
#25028=CARTESIAN_POINT('',(-1.74236521665491,1.,0.163289472382896));
#25029=CARTESIAN_POINT('Origin',(0.,1.,0.));
#25030=CARTESIAN_POINT('',(-1.74236521665491,0.,0.163289472382896));
#25031=CARTESIAN_POINT('Ctrl Pts',(-2.19890268624765,-1.,0.069476445021958));
#25032=CARTESIAN_POINT('Ctrl Pts',(-2.19890268624765,1.,0.069476445021958));
#25033=CARTESIAN_POINT('Ctrl Pts',(-2.19777582085423,-1.,0.0701143536325489));
#25034=CARTESIAN_POINT('Ctrl Pts',(-2.19777582085423,1.,0.0701143536325489));
#25035=CARTESIAN_POINT('Ctrl Pts',(-2.19552129484002,-1.,0.0713863779526153));
#25036=CARTESIAN_POINT('Ctrl Pts',(-2.19552129484002,1.,0.0713863779526153));
#25037=CARTESIAN_POINT('Ctrl Pts',(-2.19213712013662,-1.,0.0732830357306724));
#25038=CARTESIAN_POINT('Ctrl Pts',(-2.19213712013662,1.,0.0732830357306724));
#25039=CARTESIAN_POINT('Ctrl Pts',(-2.1876201139953,-1.,0.0757891465836146));
#25040=CARTESIAN_POINT('Ctrl Pts',(-2.1876201139953,1.,0.0757891465836146));
#25041=CARTESIAN_POINT('Ctrl Pts',(-2.18196589448887,-1.,0.0788837727685241));
#25042=CARTESIAN_POINT('Ctrl Pts',(-2.18196589448887,1.,0.0788837727685241));
#25043=CARTESIAN_POINT('Ctrl Pts',(-2.176303712113,-1.,0.0819402680872764));
#25044=CARTESIAN_POINT('Ctrl Pts',(-2.176303712113,1.,0.0819402680872764));
#25045=CARTESIAN_POINT('Ctrl Pts',(-2.17063357870952,-1.,0.0849584620835371));
#25046=CARTESIAN_POINT('Ctrl Pts',(-2.17063357870952,1.,0.0849584620835371));
#25047=CARTESIAN_POINT('Ctrl Pts',(-2.16495552645014,-1.,0.0879381291386921));
#25048=CARTESIAN_POINT('Ctrl Pts',(-2.16495552645014,1.,0.0879381291386921));
#25049=CARTESIAN_POINT('Ctrl Pts',(-2.15926961544516,-1.,0.0908789888107264));
#25050=CARTESIAN_POINT('Ctrl Pts',(-2.15926961544516,1.,0.0908789888107264));
#25051=CARTESIAN_POINT('Ctrl Pts',(-2.1535759397817,-1.,0.0937807218867642));
#25052=CARTESIAN_POINT('Ctrl Pts',(-2.1535759397817,1.,0.0937807218867642));
#25053=CARTESIAN_POINT('Ctrl Pts',(-2.14787463531795,-1.,0.0966429852305457));
#25054=CARTESIAN_POINT('Ctrl Pts',(-2.14787463531795,1.,0.0966429852305457));
#25055=CARTESIAN_POINT('Ctrl Pts',(-2.14216588396025,-1.,0.0994654261990914));
#25056=CARTESIAN_POINT('Ctrl Pts',(-2.14216588396025,1.,0.0994654261990914));
#25057=CARTESIAN_POINT('Ctrl Pts',(-2.13644992667165,-1.,0.1022477005561));
#25058=CARTESIAN_POINT('Ctrl Pts',(-2.13644992667165,1.,0.1022477005561));
#25059=CARTESIAN_POINT('Ctrl Pts',(-2.13072704887293,-1.,0.104989479152739));
#25060=CARTESIAN_POINT('Ctrl Pts',(-2.13072704887293,1.,0.104989479152739));
#25061=CARTESIAN_POINT('Ctrl Pts',(-2.12499752307,-1.,0.10769043523109));
#25062=CARTESIAN_POINT('Ctrl Pts',(-2.12499752307,1.,0.10769043523109));
#25063=CARTESIAN_POINT('Ctrl Pts',(-2.11926155590865,-1.,0.110350236135025));
#25064=CARTESIAN_POINT('Ctrl Pts',(-2.11926155590865,1.,0.110350236135025));
#25065=CARTESIAN_POINT('Ctrl Pts',(-2.11351924490306,-1.,0.112968534419737));
#25066=CARTESIAN_POINT('Ctrl Pts',(-2.11351924490306,1.,0.112968534419737));
#25067=CARTESIAN_POINT('Ctrl Pts',(-2.10777050261309,-1.,0.115544957687926));
#25068=CARTESIAN_POINT('Ctrl Pts',(-2.10777050261309,1.,0.115544957687926));
#25069=CARTESIAN_POINT('Ctrl Pts',(-2.102015121329,-1.,0.118079107988355));
#25070=CARTESIAN_POINT('Ctrl Pts',(-2.102015121329,1.,0.118079107988355));
#25071=CARTESIAN_POINT('Ctrl Pts',(-2.0962529286773,-1.,0.120570567965122));
#25072=CARTESIAN_POINT('Ctrl Pts',(-2.0962529286773,1.,0.120570567965122));
#25073=CARTESIAN_POINT('Ctrl Pts',(-2.09048392424825,-1.,0.123018905621083));
#25074=CARTESIAN_POINT('Ctrl Pts',(-2.09048392424825,1.,0.123018905621083));
#25075=CARTESIAN_POINT('Ctrl Pts',(-2.08470840653643,-1.,0.125423679412061));
#25076=CARTESIAN_POINT('Ctrl Pts',(-2.08470840653643,1.,0.125423679412061));
#25077=CARTESIAN_POINT('Ctrl Pts',(-2.07892715110987,-1.,0.12778444527612));
#25078=CARTESIAN_POINT('Ctrl Pts',(-2.07892715110987,1.,0.12778444527612));
#25079=CARTESIAN_POINT('Ctrl Pts',(-2.07314114713063,-1.,0.130100748328403));
#25080=CARTESIAN_POINT('Ctrl Pts',(-2.07314114713063,1.,0.130100748328403));
#25081=CARTESIAN_POINT('Ctrl Pts',(-2.06735123910326,-1.,0.13237211154771));
#25082=CARTESIAN_POINT('Ctrl Pts',(-2.06735123910326,1.,0.13237211154771));
#25083=CARTESIAN_POINT('Ctrl Pts',(-2.06155781517842,-1.,0.134598026192106));
#25084=CARTESIAN_POINT('Ctrl Pts',(-2.06155781517842,1.,0.134598026192106));
#25085=CARTESIAN_POINT('Ctrl Pts',(-2.05576044414264,-1.,0.136777941218043));
#25086=CARTESIAN_POINT('Ctrl Pts',(-2.05576044414264,1.,0.136777941218043));
#25087=CARTESIAN_POINT('Ctrl Pts',(-2.04995762001328,-1.,0.138911255368966));
#25088=CARTESIAN_POINT('Ctrl Pts',(-2.04995762001328,1.,0.138911255368966));
#25089=CARTESIAN_POINT('Ctrl Pts',(-2.04414757947916,-1.,0.140997332152546));
#25090=CARTESIAN_POINT('Ctrl Pts',(-2.04414757947916,1.,0.140997332152546));
#25091=CARTESIAN_POINT('Ctrl Pts',(-2.03832911025912,-1.,0.143035515058209));
#25092=CARTESIAN_POINT('Ctrl Pts',(-2.03832911025912,1.,0.143035515058209));
#25093=CARTESIAN_POINT('Ctrl Pts',(-2.03250223739942,-1.,0.145025140186057));
#25094=CARTESIAN_POINT('Ctrl Pts',(-2.03250223739942,1.,0.145025140186057));
#25095=CARTESIAN_POINT('Ctrl Pts',(-2.02666926182017,-1.,0.146965557332583));
#25096=CARTESIAN_POINT('Ctrl Pts',(-2.02666926182017,1.,0.146965557332583));
#25097=CARTESIAN_POINT('Ctrl Pts',(-2.02083464969894,-1.,0.148856124775337));
#25098=CARTESIAN_POINT('Ctrl Pts',(-2.02083464969894,1.,0.148856124775337));
#25099=CARTESIAN_POINT('Ctrl Pts',(-2.01500291940238,-1.,0.150696157673078));
#25100=CARTESIAN_POINT('Ctrl Pts',(-2.01500291940238,1.,0.150696157673078));
#25101=CARTESIAN_POINT('Ctrl Pts',(-2.00917680318424,-1.,0.15248488362145));
#25102=CARTESIAN_POINT('Ctrl Pts',(-2.00917680318424,1.,0.15248488362145));
#25103=CARTESIAN_POINT('Ctrl Pts',(-2.00335565310543,-1.,0.154221403049722));
#25104=CARTESIAN_POINT('Ctrl Pts',(-2.00335565310543,1.,0.154221403049722));
#25105=CARTESIAN_POINT('Ctrl Pts',(-1.99753284771497,-1.,0.155904629548783));
#25106=CARTESIAN_POINT('Ctrl Pts',(-1.99753284771497,1.,0.155904629548783));
#25107=CARTESIAN_POINT('Ctrl Pts',(-1.99169810931908,-1.,0.157533331459227));
#25108=CARTESIAN_POINT('Ctrl Pts',(-1.99169810931908,1.,0.157533331459227));
#25109=CARTESIAN_POINT('Ctrl Pts',(-1.98584238283292,-1.,0.159106226437299));
#25110=CARTESIAN_POINT('Ctrl Pts',(-1.98584238283292,1.,0.159106226437299));
#25111=CARTESIAN_POINT('Ctrl Pts',(-1.97996195437559,-1.,0.160622060784611));
#25112=CARTESIAN_POINT('Ctrl Pts',(-1.97996195437559,1.,0.160622060784611));
#25113=CARTESIAN_POINT('Ctrl Pts',(-1.97406280235188,-1.,0.162079693556288));
#25114=CARTESIAN_POINT('Ctrl Pts',(-1.97406280235188,1.,0.162079693556288));
#25115=CARTESIAN_POINT('Ctrl Pts',(-1.96816512677967,-1.,0.163478185457734));
#25116=CARTESIAN_POINT('Ctrl Pts',(-1.96816512677967,1.,0.163478185457734));
#25117=CARTESIAN_POINT('Ctrl Pts',(-1.96229379940136,-1.,0.164816568920269));
#25118=CARTESIAN_POINT('Ctrl Pts',(-1.96229379940136,1.,0.164816568920269));
#25119=CARTESIAN_POINT('Ctrl Pts',(-1.9564675971873,-1.,0.166093592002812));
#25120=CARTESIAN_POINT('Ctrl Pts',(-1.9564675971873,1.,0.166093592002812));
#25121=CARTESIAN_POINT('Ctrl Pts',(-1.95069027794294,-1.,0.167307501784475));
#25122=CARTESIAN_POINT('Ctrl Pts',(-1.95069027794294,1.,0.167307501784475));
#25123=CARTESIAN_POINT('Ctrl Pts',(-1.94493757756931,-1.,0.168455741607556));
#25124=CARTESIAN_POINT('Ctrl Pts',(-1.94493757756931,1.,0.168455741607556));
#25125=CARTESIAN_POINT('Ctrl Pts',(-1.93915639211581,-1.,0.169534904817491));
#25126=CARTESIAN_POINT('Ctrl Pts',(-1.93915639211581,1.,0.169534904817491));
#25127=CARTESIAN_POINT('Ctrl Pts',(-1.93329183155539,-1.,0.170541253116201));
#25128=CARTESIAN_POINT('Ctrl Pts',(-1.93329183155539,1.,0.170541253116201));
#25129=CARTESIAN_POINT('Ctrl Pts',(-1.92731093582036,-1.,0.171471191532988));
#25130=CARTESIAN_POINT('Ctrl Pts',(-1.92731093582036,1.,0.171471191532988));
#25131=CARTESIAN_POINT('Ctrl Pts',(-1.9212233439798,-1.,0.172321621259514));
#25132=CARTESIAN_POINT('Ctrl Pts',(-1.9212233439798,1.,0.172321621259514));
#25133=CARTESIAN_POINT('Ctrl Pts',(-1.91511429159527,-1.,0.173090695383496));
#25134=CARTESIAN_POINT('Ctrl Pts',(-1.91511429159527,1.,0.173090695383496));
#25135=CARTESIAN_POINT('Ctrl Pts',(-1.90911693975267,-1.,0.173776635257817));
#25136=CARTESIAN_POINT('Ctrl Pts',(-1.90911693975267,1.,0.173776635257817));
#25137=CARTESIAN_POINT('Ctrl Pts',(-1.90335253862834,-1.,0.174375518661085));
#25138=CARTESIAN_POINT('Ctrl Pts',(-1.90335253862834,1.,0.174375518661085));
#25139=CARTESIAN_POINT('Ctrl Pts',(-1.89788101117132,-1.,0.174879405091263));
#25140=CARTESIAN_POINT('Ctrl Pts',(-1.89788101117132,1.,0.174879405091263));
#25141=CARTESIAN_POINT('Ctrl Pts',(-1.892646301985,-1.,0.175274276190844));
#25142=CARTESIAN_POINT('Ctrl Pts',(-1.892646301985,1.,0.175274276190844));
#25143=CARTESIAN_POINT('Ctrl Pts',(-1.88742606273259,-1.,0.175538155840648));
#25144=CARTESIAN_POINT('Ctrl Pts',(-1.88742606273259,1.,0.175538155840648));
#25145=CARTESIAN_POINT('Ctrl Pts',(-1.88188663145367,-1.,0.175644148889698));
#25146=CARTESIAN_POINT('Ctrl Pts',(-1.88188663145367,1.,0.175644148889698));
#25147=CARTESIAN_POINT('Ctrl Pts',(-1.87563767773588,-1.,0.175563480746485));
#25148=CARTESIAN_POINT('Ctrl Pts',(-1.87563767773588,1.,0.175563480746485));
#25149=CARTESIAN_POINT('Ctrl Pts',(-1.86828349694799,-1.,0.175268337590758));
#25150=CARTESIAN_POINT('Ctrl Pts',(-1.86828349694799,1.,0.175268337590758));
#25151=CARTESIAN_POINT('Ctrl Pts',(-1.85948367088837,-1.,0.17473525927603));
#25152=CARTESIAN_POINT('Ctrl Pts',(-1.85948367088837,1.,0.17473525927603));
#25153=CARTESIAN_POINT('Ctrl Pts',(-1.8489811319852,-1.,0.173946627587731));
#25154=CARTESIAN_POINT('Ctrl Pts',(-1.8489811319852,1.,0.173946627587731));
#25155=CARTESIAN_POINT('Ctrl Pts',(-1.83658380527692,-1.,0.1728894428919));
#25156=CARTESIAN_POINT('Ctrl Pts',(-1.83658380527692,1.,0.1728894428919));
#25157=CARTESIAN_POINT('Ctrl Pts',(-1.82215766811545,-1.,0.171554770204119));
#25158=CARTESIAN_POINT('Ctrl Pts',(-1.82215766811545,1.,0.171554770204119));
#25159=CARTESIAN_POINT('Ctrl Pts',(-1.80561530629706,-1.,0.169936923904608));
#25160=CARTESIAN_POINT('Ctrl Pts',(-1.80561530629706,1.,0.169936923904608));
#25161=CARTESIAN_POINT('Ctrl Pts',(-1.7869064998507,-1.,0.168032772805197));
#25162=CARTESIAN_POINT('Ctrl Pts',(-1.7869064998507,1.,0.168032772805197));
#25163=CARTESIAN_POINT('Ctrl Pts',(-1.77018771684844,-1.,0.1662793551464));
#25164=CARTESIAN_POINT('Ctrl Pts',(-1.77018771684844,1.,0.1662793551464));
#25165=CARTESIAN_POINT('Ctrl Pts',(-1.75666056638427,-1.,0.164834765707158));
#25166=CARTESIAN_POINT('Ctrl Pts',(-1.75666056638427,1.,0.164834765707158));
#25167=CARTESIAN_POINT('Ctrl Pts',(-1.7472034950333,-1.,0.163814161002002));
#25168=CARTESIAN_POINT('Ctrl Pts',(-1.7472034950333,1.,0.163814161002002));
#25169=CARTESIAN_POINT('Ctrl Pts',(-1.74236521665491,-1.,0.163289472382896));
#25170=CARTESIAN_POINT('Ctrl Pts',(-1.74236521665491,1.,0.163289472382896));
#25171=CARTESIAN_POINT('',(-2.19890268624765,1.,0.069476445021958));
#25172=CARTESIAN_POINT('Ctrl Pts',(-2.19890268624765,1.,0.069476445021958));
#25173=CARTESIAN_POINT('Ctrl Pts',(-2.19777582085423,1.,0.0701143536325489));
#25174=CARTESIAN_POINT('Ctrl Pts',(-2.19552129484002,1.,0.0713863779526153));
#25175=CARTESIAN_POINT('Ctrl Pts',(-2.19213712013662,1.,0.0732830357306724));
#25176=CARTESIAN_POINT('Ctrl Pts',(-2.1876201139953,1.,0.0757891465836146));
#25177=CARTESIAN_POINT('Ctrl Pts',(-2.18196589448887,1.,0.0788837727685241));
#25178=CARTESIAN_POINT('Ctrl Pts',(-2.176303712113,1.,0.0819402680872764));
#25179=CARTESIAN_POINT('Ctrl Pts',(-2.17063357870952,1.,0.0849584620835371));
#25180=CARTESIAN_POINT('Ctrl Pts',(-2.16495552645014,1.,0.0879381291386921));
#25181=CARTESIAN_POINT('Ctrl Pts',(-2.15926961544516,1.,0.0908789888107264));
#25182=CARTESIAN_POINT('Ctrl Pts',(-2.1535759397817,1.,0.0937807218867642));
#25183=CARTESIAN_POINT('Ctrl Pts',(-2.14787463531795,1.,0.0966429852305457));
#25184=CARTESIAN_POINT('Ctrl Pts',(-2.14216588396025,1.,0.0994654261990914));
#25185=CARTESIAN_POINT('Ctrl Pts',(-2.13644992667165,1.,0.1022477005561));
#25186=CARTESIAN_POINT('Ctrl Pts',(-2.13072704887293,1.,0.104989479152739));
#25187=CARTESIAN_POINT('Ctrl Pts',(-2.12499752307,1.,0.10769043523109));
#25188=CARTESIAN_POINT('Ctrl Pts',(-2.11926155590865,1.,0.110350236135025));
#25189=CARTESIAN_POINT('Ctrl Pts',(-2.11351924490306,1.,0.112968534419737));
#25190=CARTESIAN_POINT('Ctrl Pts',(-2.10777050261309,1.,0.115544957687926));
#25191=CARTESIAN_POINT('Ctrl Pts',(-2.102015121329,1.,0.118079107988355));
#25192=CARTESIAN_POINT('Ctrl Pts',(-2.0962529286773,1.,0.120570567965122));
#25193=CARTESIAN_POINT('Ctrl Pts',(-2.09048392424825,1.,0.123018905621083));
#25194=CARTESIAN_POINT('Ctrl Pts',(-2.08470840653643,1.,0.125423679412061));
#25195=CARTESIAN_POINT('Ctrl Pts',(-2.07892715110987,1.,0.12778444527612));
#25196=CARTESIAN_POINT('Ctrl Pts',(-2.07314114713063,1.,0.130100748328403));
#25197=CARTESIAN_POINT('Ctrl Pts',(-2.06735123910326,1.,0.13237211154771));
#25198=CARTESIAN_POINT('Ctrl Pts',(-2.06155781517842,1.,0.134598026192106));
#25199=CARTESIAN_POINT('Ctrl Pts',(-2.05576044414264,1.,0.136777941218043));
#25200=CARTESIAN_POINT('Ctrl Pts',(-2.04995762001328,1.,0.138911255368966));
#25201=CARTESIAN_POINT('Ctrl Pts',(-2.04414757947916,1.,0.140997332152546));
#25202=CARTESIAN_POINT('Ctrl Pts',(-2.03832911025912,1.,0.143035515058209));
#25203=CARTESIAN_POINT('Ctrl Pts',(-2.03250223739942,1.,0.145025140186057));
#25204=CARTESIAN_POINT('Ctrl Pts',(-2.02666926182017,1.,0.146965557332583));
#25205=CARTESIAN_POINT('Ctrl Pts',(-2.02083464969894,1.,0.148856124775337));
#25206=CARTESIAN_POINT('Ctrl Pts',(-2.01500291940238,1.,0.150696157673078));
#25207=CARTESIAN_POINT('Ctrl Pts',(-2.00917680318424,1.,0.15248488362145));
#25208=CARTESIAN_POINT('Ctrl Pts',(-2.00335565310543,1.,0.154221403049722));
#25209=CARTESIAN_POINT('Ctrl Pts',(-1.99753284771497,1.,0.155904629548783));
#25210=CARTESIAN_POINT('Ctrl Pts',(-1.99169810931908,1.,0.157533331459227));
#25211=CARTESIAN_POINT('Ctrl Pts',(-1.98584238283292,1.,0.159106226437299));
#25212=CARTESIAN_POINT('Ctrl Pts',(-1.97996195437559,1.,0.160622060784611));
#25213=CARTESIAN_POINT('Ctrl Pts',(-1.97406280235188,1.,0.162079693556288));
#25214=CARTESIAN_POINT('Ctrl Pts',(-1.96816512677967,1.,0.163478185457734));
#25215=CARTESIAN_POINT('Ctrl Pts',(-1.96229379940136,1.,0.164816568920269));
#25216=CARTESIAN_POINT('Ctrl Pts',(-1.9564675971873,1.,0.166093592002812));
#25217=CARTESIAN_POINT('Ctrl Pts',(-1.95069027794294,1.,0.167307501784475));
#25218=CARTESIAN_POINT('Ctrl Pts',(-1.94493757756931,1.,0.168455741607556));
#25219=CARTESIAN_POINT('Ctrl Pts',(-1.93915639211581,1.,0.169534904817491));
#25220=CARTESIAN_POINT('Ctrl Pts',(-1.93329183155539,1.,0.170541253116201));
#25221=CARTESIAN_POINT('Ctrl Pts',(-1.92731093582036,1.,0.171471191532988));
#25222=CARTESIAN_POINT('Ctrl Pts',(-1.9212233439798,1.,0.172321621259514));
#25223=CARTESIAN_POINT('Ctrl Pts',(-1.91511429159527,1.,0.173090695383496));
#25224=CARTESIAN_POINT('Ctrl Pts',(-1.90911693975267,1.,0.173776635257817));
#25225=CARTESIAN_POINT('Ctrl Pts',(-1.90335253862834,1.,0.174375518661085));
#25226=CARTESIAN_POINT('Ctrl Pts',(-1.89788101117132,1.,0.174879405091263));
#25227=CARTESIAN_POINT('Ctrl Pts',(-1.892646301985,1.,0.175274276190844));
#25228=CARTESIAN_POINT('Ctrl Pts',(-1.88742606273259,1.,0.175538155840648));
#25229=CARTESIAN_POINT('Ctrl Pts',(-1.88188663145367,1.,0.175644148889698));
#25230=CARTESIAN_POINT('Ctrl Pts',(-1.87563767773588,1.,0.175563480746485));
#25231=CARTESIAN_POINT('Ctrl Pts',(-1.86828349694799,1.,0.175268337590758));
#25232=CARTESIAN_POINT('Ctrl Pts',(-1.85948367088837,1.,0.17473525927603));
#25233=CARTESIAN_POINT('Ctrl Pts',(-1.8489811319852,1.,0.173946627587731));
#25234=CARTESIAN_POINT('Ctrl Pts',(-1.83658380527692,1.,0.1728894428919));
#25235=CARTESIAN_POINT('Ctrl Pts',(-1.82215766811545,1.,0.171554770204119));
#25236=CARTESIAN_POINT('Ctrl Pts',(-1.80561530629706,1.,0.169936923904608));
#25237=CARTESIAN_POINT('Ctrl Pts',(-1.7869064998507,1.,0.168032772805197));
#25238=CARTESIAN_POINT('Ctrl Pts',(-1.77018771684844,1.,0.1662793551464));
#25239=CARTESIAN_POINT('Ctrl Pts',(-1.75666056638427,1.,0.164834765707158));
#25240=CARTESIAN_POINT('Ctrl Pts',(-1.7472034950333,1.,0.163814161002002));
#25241=CARTESIAN_POINT('Ctrl Pts',(-1.74236521665491,1.,0.163289472382896));
#25242=CARTESIAN_POINT('',(-2.19890268624765,0.,0.069476445021958));
#25243=CARTESIAN_POINT('Origin',(-2.19890268624765,0.,-0.0694764450219585));
#25244=CARTESIAN_POINT('',(-2.19890268624765,1.,-0.0694764450219585));
#25245=CARTESIAN_POINT('',(-2.19890268624765,1.,0.069476445021958));
#25246=CARTESIAN_POINT('',(-2.19890268624765,0.,-0.0694764450219585));
#25247=CARTESIAN_POINT('Ctrl Pts',(-1.74236521665491,-1.,-0.163289472382896));
#25248=CARTESIAN_POINT('Ctrl Pts',(-1.74236521665491,1.,-0.163289472382896));
#25249=CARTESIAN_POINT('Ctrl Pts',(-1.74720349503904,-1.,-0.163814161002474));
#25250=CARTESIAN_POINT('Ctrl Pts',(-1.74720349503904,1.,-0.163814161002474));
#25251=CARTESIAN_POINT('Ctrl Pts',(-1.75666056640041,-1.,-0.164834765708484));
#25252=CARTESIAN_POINT('Ctrl Pts',(-1.75666056640041,1.,-0.164834765708484));
#25253=CARTESIAN_POINT('Ctrl Pts',(-1.77018771687692,-1.,-0.166279355148738));
#25254=CARTESIAN_POINT('Ctrl Pts',(-1.77018771687692,1.,-0.166279355148738));
#25255=CARTESIAN_POINT('Ctrl Pts',(-1.78690649988931,-1.,-0.16803277280837));
#25256=CARTESIAN_POINT('Ctrl Pts',(-1.78690649988931,1.,-0.16803277280837));
#25257=CARTESIAN_POINT('Ctrl Pts',(-1.80561530633924,-1.,-0.169936923908078));
#25258=CARTESIAN_POINT('Ctrl Pts',(-1.80561530633924,1.,-0.169936923908078));
#25259=CARTESIAN_POINT('Ctrl Pts',(-1.82215766815414,-1.,-0.171554770207306));
#25260=CARTESIAN_POINT('Ctrl Pts',(-1.82215766815414,1.,-0.171554770207306));
#25261=CARTESIAN_POINT('Ctrl Pts',(-1.83658380530747,-1.,-0.17288944289442));
#25262=CARTESIAN_POINT('Ctrl Pts',(-1.83658380530747,1.,-0.17288944289442));
#25263=CARTESIAN_POINT('Ctrl Pts',(-1.84898113200543,-1.,-0.173946627589401));
#25264=CARTESIAN_POINT('Ctrl Pts',(-1.84898113200543,1.,-0.173946627589401));
#25265=CARTESIAN_POINT('Ctrl Pts',(-1.85948367089838,-1.,-0.174735259276856));
#25266=CARTESIAN_POINT('Ctrl Pts',(-1.85948367089838,1.,-0.174735259276856));
#25267=CARTESIAN_POINT('Ctrl Pts',(-1.86828349694972,-1.,-0.175268337590901));
#25268=CARTESIAN_POINT('Ctrl Pts',(-1.86828349694972,1.,-0.175268337590901));
#25269=CARTESIAN_POINT('Ctrl Pts',(-1.87563767773249,-1.,-0.175563480746205));
#25270=CARTESIAN_POINT('Ctrl Pts',(-1.87563767773249,1.,-0.175563480746205));
#25271=CARTESIAN_POINT('Ctrl Pts',(-1.88188663144846,-1.,-0.175644148889271));
#25272=CARTESIAN_POINT('Ctrl Pts',(-1.88188663144846,1.,-0.175644148889271));
#25273=CARTESIAN_POINT('Ctrl Pts',(-1.88742606272818,-1.,-0.175538155840286));
#25274=CARTESIAN_POINT('Ctrl Pts',(-1.88742606272818,1.,-0.175538155840286));
#25275=CARTESIAN_POINT('Ctrl Pts',(-1.89264630198279,-1.,-0.175274276190664));
#25276=CARTESIAN_POINT('Ctrl Pts',(-1.89264630198279,1.,-0.175274276190664));
#25277=CARTESIAN_POINT('Ctrl Pts',(-1.89788101117148,-1.,-0.174879405091277));
#25278=CARTESIAN_POINT('Ctrl Pts',(-1.89788101117148,1.,-0.174879405091277));
#25279=CARTESIAN_POINT('Ctrl Pts',(-1.90335253863003,-1.,-0.174375518661222));
#25280=CARTESIAN_POINT('Ctrl Pts',(-1.90335253863003,1.,-0.174375518661222));
#25281=CARTESIAN_POINT('Ctrl Pts',(-1.90911693975475,-1.,-0.173776635257984));
#25282=CARTESIAN_POINT('Ctrl Pts',(-1.90911693975475,1.,-0.173776635257984));
#25283=CARTESIAN_POINT('Ctrl Pts',(-1.91511429159681,-1.,-0.173090695383619));
#25284=CARTESIAN_POINT('Ctrl Pts',(-1.91511429159681,1.,-0.173090695383619));
#25285=CARTESIAN_POINT('Ctrl Pts',(-1.92122334398034,-1.,-0.172321621259557));
#25286=CARTESIAN_POINT('Ctrl Pts',(-1.92122334398034,1.,-0.172321621259557));
#25287=CARTESIAN_POINT('Ctrl Pts',(-1.92731093582,-1.,-0.17147119153296));
#25288=CARTESIAN_POINT('Ctrl Pts',(-1.92731093582,1.,-0.17147119153296));
#25289=CARTESIAN_POINT('Ctrl Pts',(-1.93329183155455,-1.,-0.170541253116136));
#25290=CARTESIAN_POINT('Ctrl Pts',(-1.93329183155455,1.,-0.170541253116136));
#25291=CARTESIAN_POINT('Ctrl Pts',(-1.93915639211497,-1.,-0.169534904817425));
#25292=CARTESIAN_POINT('Ctrl Pts',(-1.93915639211497,1.,-0.169534904817425));
#25293=CARTESIAN_POINT('Ctrl Pts',(-1.94493757756879,-1.,-0.168455741607516));
#25294=CARTESIAN_POINT('Ctrl Pts',(-1.94493757756879,1.,-0.168455741607516));
#25295=CARTESIAN_POINT('Ctrl Pts',(-1.95069027794286,-1.,-0.167307501784469));
#25296=CARTESIAN_POINT('Ctrl Pts',(-1.95069027794286,1.,-0.167307501784469));
#25297=CARTESIAN_POINT('Ctrl Pts',(-1.95646759718755,-1.,-0.166093592002833));
#25298=CARTESIAN_POINT('Ctrl Pts',(-1.95646759718755,1.,-0.166093592002833));
#25299=CARTESIAN_POINT('Ctrl Pts',(-1.96229379940174,-1.,-0.1648165689203));
#25300=CARTESIAN_POINT('Ctrl Pts',(-1.96229379940174,1.,-0.1648165689203));
#25301=CARTESIAN_POINT('Ctrl Pts',(-1.96816512678,-1.,-0.16347818545776));
#25302=CARTESIAN_POINT('Ctrl Pts',(-1.96816512678,1.,-0.16347818545776));
#25303=CARTESIAN_POINT('Ctrl Pts',(-1.97406280235204,-1.,-0.162079693556302));
#25304=CARTESIAN_POINT('Ctrl Pts',(-1.97406280235204,1.,-0.162079693556302));
#25305=CARTESIAN_POINT('Ctrl Pts',(-1.97996195437557,-1.,-0.16062206078461));
#25306=CARTESIAN_POINT('Ctrl Pts',(-1.97996195437557,1.,-0.16062206078461));
#25307=CARTESIAN_POINT('Ctrl Pts',(-1.98584238283279,-1.,-0.159106226437289));
#25308=CARTESIAN_POINT('Ctrl Pts',(-1.98584238283279,1.,-0.159106226437289));
#25309=CARTESIAN_POINT('Ctrl Pts',(-1.99169810931893,-1.,-0.157533331459215));
#25310=CARTESIAN_POINT('Ctrl Pts',(-1.99169810931893,1.,-0.157533331459215));
#25311=CARTESIAN_POINT('Ctrl Pts',(-1.99753284771487,-1.,-0.155904629548775));
#25312=CARTESIAN_POINT('Ctrl Pts',(-1.99753284771487,1.,-0.155904629548775));
#25313=CARTESIAN_POINT('Ctrl Pts',(-2.00335565310539,-1.,-0.154221403049719));
#25314=CARTESIAN_POINT('Ctrl Pts',(-2.00335565310539,1.,-0.154221403049719));
#25315=CARTESIAN_POINT('Ctrl Pts',(-2.00917680318426,-1.,-0.152484883621452));
#25316=CARTESIAN_POINT('Ctrl Pts',(-2.00917680318426,1.,-0.152484883621452));
#25317=CARTESIAN_POINT('Ctrl Pts',(-2.01500291940243,-1.,-0.150696157673084));
#25318=CARTESIAN_POINT('Ctrl Pts',(-2.01500291940243,1.,-0.150696157673084));
#25319=CARTESIAN_POINT('Ctrl Pts',(-2.02083464969897,-1.,-0.148856124775343));
#25320=CARTESIAN_POINT('Ctrl Pts',(-2.02083464969897,1.,-0.148856124775343));
#25321=CARTESIAN_POINT('Ctrl Pts',(-2.02666926182017,-1.,-0.146965557332586));
#25322=CARTESIAN_POINT('Ctrl Pts',(-2.02666926182017,1.,-0.146965557332586));
#25323=CARTESIAN_POINT('Ctrl Pts',(-2.03250223739941,-1.,-0.145025140186058));
#25324=CARTESIAN_POINT('Ctrl Pts',(-2.03250223739941,1.,-0.145025140186058));
#25325=CARTESIAN_POINT('Ctrl Pts',(-2.03832911025913,-1.,-0.143035515058208));
#25326=CARTESIAN_POINT('Ctrl Pts',(-2.03832911025913,1.,-0.143035515058208));
#25327=CARTESIAN_POINT('Ctrl Pts',(-2.04414757947919,-1.,-0.140997332152545));
#25328=CARTESIAN_POINT('Ctrl Pts',(-2.04414757947919,1.,-0.140997332152545));
#25329=CARTESIAN_POINT('Ctrl Pts',(-2.04995762001333,-1.,-0.138911255368966));
#25330=CARTESIAN_POINT('Ctrl Pts',(-2.04995762001333,1.,-0.138911255368966));
#25331=CARTESIAN_POINT('Ctrl Pts',(-2.0557604441427,-1.,-0.136777941218044));
#25332=CARTESIAN_POINT('Ctrl Pts',(-2.0557604441427,1.,-0.136777941218044));
#25333=CARTESIAN_POINT('Ctrl Pts',(-2.06155781517844,-1.,-0.134598026192107));
#25334=CARTESIAN_POINT('Ctrl Pts',(-2.06155781517844,1.,-0.134598026192107));
#25335=CARTESIAN_POINT('Ctrl Pts',(-2.06735123910319,-1.,-0.13237211154771));
#25336=CARTESIAN_POINT('Ctrl Pts',(-2.06735123910319,1.,-0.13237211154771));
#25337=CARTESIAN_POINT('Ctrl Pts',(-2.07314114713047,-1.,-0.130100748328401));
#25338=CARTESIAN_POINT('Ctrl Pts',(-2.07314114713047,1.,-0.130100748328401));
#25339=CARTESIAN_POINT('Ctrl Pts',(-2.07892715110967,-1.,-0.127784445276116));
#25340=CARTESIAN_POINT('Ctrl Pts',(-2.07892715110967,1.,-0.127784445276116));
#25341=CARTESIAN_POINT('Ctrl Pts',(-2.08470840653628,-1.,-0.125423679412058));
#25342=CARTESIAN_POINT('Ctrl Pts',(-2.08470840653628,1.,-0.125423679412058));
#25343=CARTESIAN_POINT('Ctrl Pts',(-2.09048392424826,-1.,-0.123018905621083));
#25344=CARTESIAN_POINT('Ctrl Pts',(-2.09048392424826,1.,-0.123018905621083));
#25345=CARTESIAN_POINT('Ctrl Pts',(-2.09625292867756,-1.,-0.120570567965129));
#25346=CARTESIAN_POINT('Ctrl Pts',(-2.09625292867756,1.,-0.120570567965129));
#25347=CARTESIAN_POINT('Ctrl Pts',(-2.10201512132945,-1.,-0.118079107988368));
#25348=CARTESIAN_POINT('Ctrl Pts',(-2.10201512132945,1.,-0.118079107988368));
#25349=CARTESIAN_POINT('Ctrl Pts',(-2.10777050261359,-1.,-0.11554495768794));
#25350=CARTESIAN_POINT('Ctrl Pts',(-2.10777050261359,1.,-0.11554495768794));
#25351=CARTESIAN_POINT('Ctrl Pts',(-2.11351924490335,-1.,-0.112968534419746));
#25352=CARTESIAN_POINT('Ctrl Pts',(-2.11351924490335,1.,-0.112968534419746));
#25353=CARTESIAN_POINT('Ctrl Pts',(-2.11926155590849,-1.,-0.11035023613502));
#25354=CARTESIAN_POINT('Ctrl Pts',(-2.11926155590849,1.,-0.11035023613502));
#25355=CARTESIAN_POINT('Ctrl Pts',(-2.12499752306927,-1.,-0.107690435231068));
#25356=CARTESIAN_POINT('Ctrl Pts',(-2.12499752306927,1.,-0.107690435231068));
#25357=CARTESIAN_POINT('Ctrl Pts',(-2.1307270488718,-1.,-0.104989479152703));
#25358=CARTESIAN_POINT('Ctrl Pts',(-2.1307270488718,1.,-0.104989479152703));
#25359=CARTESIAN_POINT('Ctrl Pts',(-2.13644992667052,-1.,-0.102247700556064));
#25360=CARTESIAN_POINT('Ctrl Pts',(-2.13644992667052,1.,-0.102247700556064));
#25361=CARTESIAN_POINT('Ctrl Pts',(-2.14216588395974,-1.,-0.0994654261990744));
#25362=CARTESIAN_POINT('Ctrl Pts',(-2.14216588395974,1.,-0.0994654261990744));
#25363=CARTESIAN_POINT('Ctrl Pts',(-2.14787463531864,-1.,-0.096642985230569));
#25364=CARTESIAN_POINT('Ctrl Pts',(-2.14787463531864,1.,-0.096642985230569));
#25365=CARTESIAN_POINT('Ctrl Pts',(-2.15357593978377,-1.,-0.0937807218868346));
#25366=CARTESIAN_POINT('Ctrl Pts',(-2.15357593978377,1.,-0.0937807218868346));
#25367=CARTESIAN_POINT('Ctrl Pts',(-2.15926961544808,-1.,-0.0908789888108267));
#25368=CARTESIAN_POINT('Ctrl Pts',(-2.15926961544808,1.,-0.0908789888108267));
#25369=CARTESIAN_POINT('Ctrl Pts',(-2.16495552645275,-1.,-0.0879381291387824));
#25370=CARTESIAN_POINT('Ctrl Pts',(-2.16495552645275,1.,-0.0879381291387824));
#25371=CARTESIAN_POINT('Ctrl Pts',(-2.17063357871031,-1.,-0.0849584620835644));
#25372=CARTESIAN_POINT('Ctrl Pts',(-2.17063357871031,1.,-0.0849584620835644));
#25373=CARTESIAN_POINT('Ctrl Pts',(-2.1763037121106,-1.,-0.0819402680871941));
#25374=CARTESIAN_POINT('Ctrl Pts',(-2.1763037121106,1.,-0.0819402680871941));
#25375=CARTESIAN_POINT('Ctrl Pts',(-2.18196589448304,-1.,-0.0788837727683229));
#25376=CARTESIAN_POINT('Ctrl Pts',(-2.18196589448304,1.,-0.0788837727683229));
#25377=CARTESIAN_POINT('Ctrl Pts',(-2.1876201139874,-1.,-0.0757891465833413));
#25378=CARTESIAN_POINT('Ctrl Pts',(-2.1876201139874,1.,-0.0757891465833413));
#25379=CARTESIAN_POINT('Ctrl Pts',(-2.19213712012956,-1.,-0.0732830357304277));
#25380=CARTESIAN_POINT('Ctrl Pts',(-2.19213712012956,1.,-0.0732830357304277));
#25381=CARTESIAN_POINT('Ctrl Pts',(-2.19552129483562,-1.,-0.0713863779524629));
#25382=CARTESIAN_POINT('Ctrl Pts',(-2.19552129483562,1.,-0.0713863779524629));
#25383=CARTESIAN_POINT('Ctrl Pts',(-2.19777582085261,-1.,-0.0701143536324927));
#25384=CARTESIAN_POINT('Ctrl Pts',(-2.19777582085261,1.,-0.0701143536324927));
#25385=CARTESIAN_POINT('Ctrl Pts',(-2.19890268624765,-1.,-0.0694764450219585));
#25386=CARTESIAN_POINT('Ctrl Pts',(-2.19890268624765,1.,-0.0694764450219585));
#25387=CARTESIAN_POINT('',(-1.74236521665491,1.,-0.163289472382896));
#25388=CARTESIAN_POINT('Ctrl Pts',(-1.74236521665491,1.,-0.163289472382896));
#25389=CARTESIAN_POINT('Ctrl Pts',(-1.74720349503904,1.,-0.163814161002474));
#25390=CARTESIAN_POINT('Ctrl Pts',(-1.75666056640041,1.,-0.164834765708484));
#25391=CARTESIAN_POINT('Ctrl Pts',(-1.77018771687692,1.,-0.166279355148738));
#25392=CARTESIAN_POINT('Ctrl Pts',(-1.78690649988931,1.,-0.16803277280837));
#25393=CARTESIAN_POINT('Ctrl Pts',(-1.80561530633924,1.,-0.169936923908078));
#25394=CARTESIAN_POINT('Ctrl Pts',(-1.82215766815414,1.,-0.171554770207306));
#25395=CARTESIAN_POINT('Ctrl Pts',(-1.83658380530747,1.,-0.17288944289442));
#25396=CARTESIAN_POINT('Ctrl Pts',(-1.84898113200543,1.,-0.173946627589401));
#25397=CARTESIAN_POINT('Ctrl Pts',(-1.85948367089838,1.,-0.174735259276856));
#25398=CARTESIAN_POINT('Ctrl Pts',(-1.86828349694972,1.,-0.175268337590901));
#25399=CARTESIAN_POINT('Ctrl Pts',(-1.87563767773249,1.,-0.175563480746205));
#25400=CARTESIAN_POINT('Ctrl Pts',(-1.88188663144846,1.,-0.175644148889271));
#25401=CARTESIAN_POINT('Ctrl Pts',(-1.88742606272818,1.,-0.175538155840286));
#25402=CARTESIAN_POINT('Ctrl Pts',(-1.89264630198279,1.,-0.175274276190664));
#25403=CARTESIAN_POINT('Ctrl Pts',(-1.89788101117148,1.,-0.174879405091277));
#25404=CARTESIAN_POINT('Ctrl Pts',(-1.90335253863003,1.,-0.174375518661222));
#25405=CARTESIAN_POINT('Ctrl Pts',(-1.90911693975475,1.,-0.173776635257984));
#25406=CARTESIAN_POINT('Ctrl Pts',(-1.91511429159681,1.,-0.173090695383619));
#25407=CARTESIAN_POINT('Ctrl Pts',(-1.92122334398034,1.,-0.172321621259557));
#25408=CARTESIAN_POINT('Ctrl Pts',(-1.92731093582,1.,-0.17147119153296));
#25409=CARTESIAN_POINT('Ctrl Pts',(-1.93329183155455,1.,-0.170541253116136));
#25410=CARTESIAN_POINT('Ctrl Pts',(-1.93915639211497,1.,-0.169534904817425));
#25411=CARTESIAN_POINT('Ctrl Pts',(-1.94493757756879,1.,-0.168455741607516));
#25412=CARTESIAN_POINT('Ctrl Pts',(-1.95069027794286,1.,-0.167307501784469));
#25413=CARTESIAN_POINT('Ctrl Pts',(-1.95646759718755,1.,-0.166093592002833));
#25414=CARTESIAN_POINT('Ctrl Pts',(-1.96229379940174,1.,-0.1648165689203));
#25415=CARTESIAN_POINT('Ctrl Pts',(-1.96816512678,1.,-0.16347818545776));
#25416=CARTESIAN_POINT('Ctrl Pts',(-1.97406280235204,1.,-0.162079693556302));
#25417=CARTESIAN_POINT('Ctrl Pts',(-1.97996195437557,1.,-0.16062206078461));
#25418=CARTESIAN_POINT('Ctrl Pts',(-1.98584238283279,1.,-0.159106226437289));
#25419=CARTESIAN_POINT('Ctrl Pts',(-1.99169810931893,1.,-0.157533331459215));
#25420=CARTESIAN_POINT('Ctrl Pts',(-1.99753284771487,1.,-0.155904629548775));
#25421=CARTESIAN_POINT('Ctrl Pts',(-2.00335565310539,1.,-0.154221403049719));
#25422=CARTESIAN_POINT('Ctrl Pts',(-2.00917680318426,1.,-0.152484883621452));
#25423=CARTESIAN_POINT('Ctrl Pts',(-2.01500291940243,1.,-0.150696157673084));
#25424=CARTESIAN_POINT('Ctrl Pts',(-2.02083464969897,1.,-0.148856124775343));
#25425=CARTESIAN_POINT('Ctrl Pts',(-2.02666926182017,1.,-0.146965557332586));
#25426=CARTESIAN_POINT('Ctrl Pts',(-2.03250223739941,1.,-0.145025140186058));
#25427=CARTESIAN_POINT('Ctrl Pts',(-2.03832911025913,1.,-0.143035515058208));
#25428=CARTESIAN_POINT('Ctrl Pts',(-2.04414757947919,1.,-0.140997332152545));
#25429=CARTESIAN_POINT('Ctrl Pts',(-2.04995762001333,1.,-0.138911255368966));
#25430=CARTESIAN_POINT('Ctrl Pts',(-2.0557604441427,1.,-0.136777941218044));
#25431=CARTESIAN_POINT('Ctrl Pts',(-2.06155781517844,1.,-0.134598026192107));
#25432=CARTESIAN_POINT('Ctrl Pts',(-2.06735123910319,1.,-0.13237211154771));
#25433=CARTESIAN_POINT('Ctrl Pts',(-2.07314114713047,1.,-0.130100748328401));
#25434=CARTESIAN_POINT('Ctrl Pts',(-2.07892715110967,1.,-0.127784445276116));
#25435=CARTESIAN_POINT('Ctrl Pts',(-2.08470840653628,1.,-0.125423679412058));
#25436=CARTESIAN_POINT('Ctrl Pts',(-2.09048392424826,1.,-0.123018905621083));
#25437=CARTESIAN_POINT('Ctrl Pts',(-2.09625292867756,1.,-0.120570567965129));
#25438=CARTESIAN_POINT('Ctrl Pts',(-2.10201512132945,1.,-0.118079107988368));
#25439=CARTESIAN_POINT('Ctrl Pts',(-2.10777050261359,1.,-0.11554495768794));
#25440=CARTESIAN_POINT('Ctrl Pts',(-2.11351924490335,1.,-0.112968534419746));
#25441=CARTESIAN_POINT('Ctrl Pts',(-2.11926155590849,1.,-0.11035023613502));
#25442=CARTESIAN_POINT('Ctrl Pts',(-2.12499752306927,1.,-0.107690435231068));
#25443=CARTESIAN_POINT('Ctrl Pts',(-2.1307270488718,1.,-0.104989479152703));
#25444=CARTESIAN_POINT('Ctrl Pts',(-2.13644992667052,1.,-0.102247700556064));
#25445=CARTESIAN_POINT('Ctrl Pts',(-2.14216588395974,1.,-0.0994654261990744));
#25446=CARTESIAN_POINT('Ctrl Pts',(-2.14787463531864,1.,-0.096642985230569));
#25447=CARTESIAN_POINT('Ctrl Pts',(-2.15357593978377,1.,-0.0937807218868346));
#25448=CARTESIAN_POINT('Ctrl Pts',(-2.15926961544808,1.,-0.0908789888108267));
#25449=CARTESIAN_POINT('Ctrl Pts',(-2.16495552645275,1.,-0.0879381291387824));
#25450=CARTESIAN_POINT('Ctrl Pts',(-2.17063357871031,1.,-0.0849584620835644));
#25451=CARTESIAN_POINT('Ctrl Pts',(-2.1763037121106,1.,-0.0819402680871941));
#25452=CARTESIAN_POINT('Ctrl Pts',(-2.18196589448304,1.,-0.0788837727683229));
#25453=CARTESIAN_POINT('Ctrl Pts',(-2.1876201139874,1.,-0.0757891465833413));
#25454=CARTESIAN_POINT('Ctrl Pts',(-2.19213712012956,1.,-0.0732830357304277));
#25455=CARTESIAN_POINT('Ctrl Pts',(-2.19552129483562,1.,-0.0713863779524629));
#25456=CARTESIAN_POINT('Ctrl Pts',(-2.19777582085261,1.,-0.0701143536324927));
#25457=CARTESIAN_POINT('Ctrl Pts',(-2.19890268624765,1.,-0.0694764450219585));
#25458=CARTESIAN_POINT('',(-1.74236521665491,0.,-0.163289472382896));
#25459=CARTESIAN_POINT('Origin',(0.,0.,0.));
#25460=CARTESIAN_POINT('',(-1.7075470150345,1.,-0.383122945602004));
#25461=CARTESIAN_POINT('Origin',(0.,1.,0.));
#25462=CARTESIAN_POINT('',(-1.7075470150345,0.,-0.383122945602004));
#25463=CARTESIAN_POINT('Ctrl Pts',(-2.11275013067528,-1.,-0.61342227326009));
#25464=CARTESIAN_POINT('Ctrl Pts',(-2.11275013067528,1.,-0.61342227326009));
#25465=CARTESIAN_POINT('Ctrl Pts',(-2.11187554260142,-1.,-0.61246736556225));
#25466=CARTESIAN_POINT('Ctrl Pts',(-2.11187554260142,1.,-0.61246736556225));
#25467=CARTESIAN_POINT('Ctrl Pts',(-2.11012443807661,-1.,-0.610560911691113));
#25468=CARTESIAN_POINT('Ctrl Pts',(-2.11012443807661,1.,-0.610560911691113));
#25469=CARTESIAN_POINT('Ctrl Pts',(-2.10749199615859,-1.,-0.607711315456826));
#25470=CARTESIAN_POINT('Ctrl Pts',(-2.10749199615859,1.,-0.607711315456826));
#25471=CARTESIAN_POINT('Ctrl Pts',(-2.10397049887709,-1.,-0.603932030738212));
#25472=CARTESIAN_POINT('Ctrl Pts',(-2.10397049887709,1.,-0.603932030738212));
#25473=CARTESIAN_POINT('Ctrl Pts',(-2.09954930865331,-1.,-0.599241616422144));
#25474=CARTESIAN_POINT('Ctrl Pts',(-2.09954930865331,1.,-0.599241616422144));
#25475=CARTESIAN_POINT('Ctrl Pts',(-2.09510876220501,-1.,-0.594585006052823));
#25476=CARTESIAN_POINT('Ctrl Pts',(-2.09510876220501,1.,-0.594585006052823));
#25477=CARTESIAN_POINT('Ctrl Pts',(-2.09064881812053,-1.,-0.589962365403189));
#25478=CARTESIAN_POINT('Ctrl Pts',(-2.09064881812053,1.,-0.589962365403189));
#25479=CARTESIAN_POINT('Ctrl Pts',(-2.086169437277,-1.,-0.585373918990895));
#25480=CARTESIAN_POINT('Ctrl Pts',(-2.086169437277,1.,-0.585373918990895));
#25481=CARTESIAN_POINT('Ctrl Pts',(-2.08167059018138,-1.,-0.580819952107257));
#25482=CARTESIAN_POINT('Ctrl Pts',(-2.08167059018138,1.,-0.580819952107257));
#25483=CARTESIAN_POINT('Ctrl Pts',(-2.07715226767361,-1.,-0.576300797416274));
#25484=CARTESIAN_POINT('Ctrl Pts',(-2.07715226767361,1.,-0.576300797416274));
#25485=CARTESIAN_POINT('Ctrl Pts',(-2.07261449292757,-1.,-0.571816823242411));
#25486=CARTESIAN_POINT('Ctrl Pts',(-2.07261449292757,1.,-0.571816823242411));
#25487=CARTESIAN_POINT('Ctrl Pts',(-2.06805732997383,-1.,-0.567368421181229));
#25488=CARTESIAN_POINT('Ctrl Pts',(-2.06805732997383,1.,-0.567368421181229));
#25489=CARTESIAN_POINT('Ctrl Pts',(-2.06348090160697,-1.,-0.562955993082574));
#25490=CARTESIAN_POINT('Ctrl Pts',(-2.06348090160697,1.,-0.562955993082574));
#25491=CARTESIAN_POINT('Ctrl Pts',(-2.05888537756571,-1.,-0.558579940185467));
#25492=CARTESIAN_POINT('Ctrl Pts',(-2.05888537756571,1.,-0.558579940185467));
#25493=CARTESIAN_POINT('Ctrl Pts',(-2.05427091604482,-1.,-0.554240657464109));
#25494=CARTESIAN_POINT('Ctrl Pts',(-2.05427091604482,1.,-0.554240657464109));
#25495=CARTESIAN_POINT('Ctrl Pts',(-2.04963761077974,-1.,-0.549938525150342));
#25496=CARTESIAN_POINT('Ctrl Pts',(-2.04963761077974,1.,-0.549938525150342));
#25497=CARTESIAN_POINT('Ctrl Pts',(-2.0449854471456,-1.,-0.545673903817348));
#25498=CARTESIAN_POINT('Ctrl Pts',(-2.0449854471456,1.,-0.545673903817348));
#25499=CARTESIAN_POINT('Ctrl Pts',(-2.0403142269048,-1.,-0.54144712061552));
#25500=CARTESIAN_POINT('Ctrl Pts',(-2.0403142269048,1.,-0.54144712061552));
#25501=CARTESIAN_POINT('Ctrl Pts',(-2.03562362953993,-1.,-0.537258489833134));
#25502=CARTESIAN_POINT('Ctrl Pts',(-2.03562362953993,1.,-0.537258489833134));
#25503=CARTESIAN_POINT('Ctrl Pts',(-2.03091336214401,-1.,-0.533108355132905));
#25504=CARTESIAN_POINT('Ctrl Pts',(-2.03091336214401,1.,-0.533108355132905));
#25505=CARTESIAN_POINT('Ctrl Pts',(-2.02618329083289,-1.,-0.52899712724191));
#25506=CARTESIAN_POINT('Ctrl Pts',(-2.02618329083289,1.,-0.52899712724191));
#25507=CARTESIAN_POINT('Ctrl Pts',(-2.02143356304712,-1.,-0.524925318333518));
#25508=CARTESIAN_POINT('Ctrl Pts',(-2.02143356304712,1.,-0.524925318333518));
#25509=CARTESIAN_POINT('Ctrl Pts',(-2.01666477917305,-1.,-0.520893590399428));
#25510=CARTESIAN_POINT('Ctrl Pts',(-2.01666477917305,1.,-0.520893590399428));
#25511=CARTESIAN_POINT('Ctrl Pts',(-2.01187773939257,-1.,-0.516902681728733));
#25512=CARTESIAN_POINT('Ctrl Pts',(-2.01187773939257,1.,-0.516902681728733));
#25513=CARTESIAN_POINT('Ctrl Pts',(-2.00707309946955,-1.,-0.512953306961813));
#25514=CARTESIAN_POINT('Ctrl Pts',(-2.00707309946955,1.,-0.512953306961813));
#25515=CARTESIAN_POINT('Ctrl Pts',(-2.00225107134733,-1.,-0.509046069886152));
#25516=CARTESIAN_POINT('Ctrl Pts',(-2.00225107134733,1.,-0.509046069886152));
#25517=CARTESIAN_POINT('Ctrl Pts',(-1.99741107463567,-1.,-0.505181361323011));
#25518=CARTESIAN_POINT('Ctrl Pts',(-1.99741107463567,1.,-0.505181361323011));
#25519=CARTESIAN_POINT('Ctrl Pts',(-1.9925514912615,-1.,-0.501359287727129));
#25520=CARTESIAN_POINT('Ctrl Pts',(-1.9925514912615,1.,-0.501359287727129));
#25521=CARTESIAN_POINT('Ctrl Pts',(-1.98767044752929,-1.,-0.497579909545564));
#25522=CARTESIAN_POINT('Ctrl Pts',(-1.98767044752929,1.,-0.497579909545564));
#25523=CARTESIAN_POINT('Ctrl Pts',(-1.9827665876182,-1.,-0.493843476541492));
#25524=CARTESIAN_POINT('Ctrl Pts',(-1.9827665876182,1.,-0.493843476541492));
#25525=CARTESIAN_POINT('Ctrl Pts',(-1.97783973019229,-1.,-0.490150627860955));
#25526=CARTESIAN_POINT('Ctrl Pts',(-1.97783973019229,1.,-0.490150627860955));
#25527=CARTESIAN_POINT('Ctrl Pts',(-1.97289186263272,-1.,-0.486502692907661));
#25528=CARTESIAN_POINT('Ctrl Pts',(-1.97289186263272,1.,-0.486502692907661));
#25529=CARTESIAN_POINT('Ctrl Pts',(-1.96792703422358,-1.,-0.482901662120686));
#25530=CARTESIAN_POINT('Ctrl Pts',(-1.96792703422358,1.,-0.482901662120686));
#25531=CARTESIAN_POINT('Ctrl Pts',(-1.96294933055938,-1.,-0.479349583074846));
#25532=CARTESIAN_POINT('Ctrl Pts',(-1.96294933055938,1.,-0.479349583074846));
#25533=CARTESIAN_POINT('Ctrl Pts',(-1.95796111148175,-1.,-0.475848034683171));
#25534=CARTESIAN_POINT('Ctrl Pts',(-1.95796111148175,1.,-0.475848034683171));
#25535=CARTESIAN_POINT('Ctrl Pts',(-1.95296148278136,-1.,-0.472397672264079));
#25536=CARTESIAN_POINT('Ctrl Pts',(-1.95296148278136,1.,-0.472397672264079));
#25537=CARTESIAN_POINT('Ctrl Pts',(-1.94794381136524,-1.,-0.468997482913158));
#25538=CARTESIAN_POINT('Ctrl Pts',(-1.94794381136524,1.,-0.468997482913158));
#25539=CARTESIAN_POINT('Ctrl Pts',(-1.94289794196205,-1.,-0.465645462026064));
#25540=CARTESIAN_POINT('Ctrl Pts',(-1.94289794196205,1.,-0.465645462026064));
#25541=CARTESIAN_POINT('Ctrl Pts',(-1.93781486640834,-1.,-0.462340031009087));
#25542=CARTESIAN_POINT('Ctrl Pts',(-1.93781486640834,1.,-0.462340031009087));
#25543=CARTESIAN_POINT('Ctrl Pts',(-1.93269066517936,-1.,-0.459081234547931));
#25544=CARTESIAN_POINT('Ctrl Pts',(-1.93269066517936,1.,-0.459081234547931));
#25545=CARTESIAN_POINT('Ctrl Pts',(-1.92753067150461,-1.,-0.455872005174335));
#25546=CARTESIAN_POINT('Ctrl Pts',(-1.92753067150461,1.,-0.455872005174335));
#25547=CARTESIAN_POINT('Ctrl Pts',(-1.9223538064847,-1.,-0.452719478359356));
#25548=CARTESIAN_POINT('Ctrl Pts',(-1.9223538064847,1.,-0.452719478359356));
#25549=CARTESIAN_POINT('Ctrl Pts',(-1.91718342555717,-1.,-0.449632260106572));
#25550=CARTESIAN_POINT('Ctrl Pts',(-1.91718342555717,1.,-0.449632260106572));
#25551=CARTESIAN_POINT('Ctrl Pts',(-1.91203699981095,-1.,-0.446617343485651));
#25552=CARTESIAN_POINT('Ctrl Pts',(-1.91203699981095,1.,-0.446617343485651));
#25553=CARTESIAN_POINT('Ctrl Pts',(-1.90691756144906,-1.,-0.44367755684917));
#25554=CARTESIAN_POINT('Ctrl Pts',(-1.90691756144906,1.,-0.44367755684917));
#25555=CARTESIAN_POINT('Ctrl Pts',(-1.90180124389137,-1.,-0.44080783370416));
#25556=CARTESIAN_POINT('Ctrl Pts',(-1.90180124389137,1.,-0.44080783370416));
#25557=CARTESIAN_POINT('Ctrl Pts',(-1.89663648956549,-1.,-0.437995003948443));
#25558=CARTESIAN_POINT('Ctrl Pts',(-1.89663648956549,1.,-0.437995003948443));
#25559=CARTESIAN_POINT('Ctrl Pts',(-1.89136993975585,-1.,-0.43522566096358));
#25560=CARTESIAN_POINT('Ctrl Pts',(-1.89136993975585,1.,-0.43522566096358));
#25561=CARTESIAN_POINT('Ctrl Pts',(-1.88596913666828,-1.,-0.432493038548833));
#25562=CARTESIAN_POINT('Ctrl Pts',(-1.88596913666828,1.,-0.432493038548833));
#25563=CARTESIAN_POINT('Ctrl Pts',(-1.88044229001778,-1.,-0.429803062482217));
#25564=CARTESIAN_POINT('Ctrl Pts',(-1.88044229001778,1.,-0.429803062482217));
#25565=CARTESIAN_POINT('Ctrl Pts',(-1.87486989291333,-1.,-0.427183828518743));
#25566=CARTESIAN_POINT('Ctrl Pts',(-1.87486989291333,1.,-0.427183828518743));
#25567=CARTESIAN_POINT('Ctrl Pts',(-1.8693780394412,-1.,-0.424678177290876));
#25568=CARTESIAN_POINT('Ctrl Pts',(-1.8693780394412,1.,-0.424678177290876));
#25569=CARTESIAN_POINT('Ctrl Pts',(-1.86408083333863,-1.,-0.422327307417884));
#25570=CARTESIAN_POINT('Ctrl Pts',(-1.86408083333863,1.,-0.422327307417884));
#25571=CARTESIAN_POINT('Ctrl Pts',(-1.8590328109667,-1.,-0.420157287975583));
#25572=CARTESIAN_POINT('Ctrl Pts',(-1.8590328109667,1.,-0.420157287975583));
#25573=CARTESIAN_POINT('Ctrl Pts',(-1.8541763285645,-1.,-0.418164129144045));
#25574=CARTESIAN_POINT('Ctrl Pts',(-1.8541763285645,1.,-0.418164129144045));
#25575=CARTESIAN_POINT('Ctrl Pts',(-1.84929312930314,-1.,-0.416300022039885));
#25576=CARTESIAN_POINT('Ctrl Pts',(-1.84929312930314,1.,-0.416300022039885));
#25577=CARTESIAN_POINT('Ctrl Pts',(-1.84405757074218,-1.,-0.414487438255542));
#25578=CARTESIAN_POINT('Ctrl Pts',(-1.84405757074218,1.,-0.414487438255542));
#25579=CARTESIAN_POINT('Ctrl Pts',(-1.8380895347617,-1.,-0.412633125322945));
#25580=CARTESIAN_POINT('Ctrl Pts',(-1.8380895347617,1.,-0.412633125322945));
#25581=CARTESIAN_POINT('Ctrl Pts',(-1.83100408895047,-1.,-0.410641256301276));
#25582=CARTESIAN_POINT('Ctrl Pts',(-1.83100408895047,1.,-0.410641256301276));
#25583=CARTESIAN_POINT('Ctrl Pts',(-1.82247022677562,-1.,-0.408428948106227));
#25584=CARTESIAN_POINT('Ctrl Pts',(-1.82247022677562,1.,-0.408428948106227));
#25585=CARTESIAN_POINT('Ctrl Pts',(-1.81223801812013,-1.,-0.405933518407175));
#25586=CARTESIAN_POINT('Ctrl Pts',(-1.81223801812013,1.,-0.405933518407175));
#25587=CARTESIAN_POINT('Ctrl Pts',(-1.80012077173238,-1.,-0.403107976163396));
#25588=CARTESIAN_POINT('Ctrl Pts',(-1.80012077173238,1.,-0.403107976163396));
#25589=CARTESIAN_POINT('Ctrl Pts',(-1.78598826343754,-1.,-0.399919403774155));
#25590=CARTESIAN_POINT('Ctrl Pts',(-1.78598826343754,1.,-0.399919403774155));
#25591=CARTESIAN_POINT('Ctrl Pts',(-1.76975560043442,-1.,-0.396346196110688));
#25592=CARTESIAN_POINT('Ctrl Pts',(-1.76975560043442,1.,-0.396346196110688));
#25593=CARTESIAN_POINT('Ctrl Pts',(-1.75137405310193,-1.,-0.392375812285395));
#25594=CARTESIAN_POINT('Ctrl Pts',(-1.75137405310193,1.,-0.392375812285395));
#25595=CARTESIAN_POINT('Ctrl Pts',(-1.73493170972829,-1.,-0.388877023502615));
#25596=CARTESIAN_POINT('Ctrl Pts',(-1.73493170972829,1.,-0.388877023502615));
#25597=CARTESIAN_POINT('Ctrl Pts',(-1.72162022244582,-1.,-0.386070790323281));
#25598=CARTESIAN_POINT('Ctrl Pts',(-1.72162022244582,1.,-0.386070790323281));
#25599=CARTESIAN_POINT('Ctrl Pts',(-1.71231062891398,-1.,-0.384119047314215));
#25600=CARTESIAN_POINT('Ctrl Pts',(-1.71231062891398,1.,-0.384119047314215));
#25601=CARTESIAN_POINT('Ctrl Pts',(-1.7075470150345,-1.,-0.383122945602004));
#25602=CARTESIAN_POINT('Ctrl Pts',(-1.7075470150345,1.,-0.383122945602004));
#25603=CARTESIAN_POINT('',(-2.11275013067528,1.,-0.61342227326009));
#25604=CARTESIAN_POINT('Ctrl Pts',(-2.11275013067528,1.,-0.61342227326009));
#25605=CARTESIAN_POINT('Ctrl Pts',(-2.11187554260142,1.,-0.61246736556225));
#25606=CARTESIAN_POINT('Ctrl Pts',(-2.11012443807661,1.,-0.610560911691113));
#25607=CARTESIAN_POINT('Ctrl Pts',(-2.10749199615859,1.,-0.607711315456826));
#25608=CARTESIAN_POINT('Ctrl Pts',(-2.10397049887709,1.,-0.603932030738212));
#25609=CARTESIAN_POINT('Ctrl Pts',(-2.09954930865331,1.,-0.599241616422144));
#25610=CARTESIAN_POINT('Ctrl Pts',(-2.09510876220501,1.,-0.594585006052823));
#25611=CARTESIAN_POINT('Ctrl Pts',(-2.09064881812053,1.,-0.589962365403189));
#25612=CARTESIAN_POINT('Ctrl Pts',(-2.086169437277,1.,-0.585373918990895));
#25613=CARTESIAN_POINT('Ctrl Pts',(-2.08167059018138,1.,-0.580819952107257));
#25614=CARTESIAN_POINT('Ctrl Pts',(-2.07715226767361,1.,-0.576300797416274));
#25615=CARTESIAN_POINT('Ctrl Pts',(-2.07261449292757,1.,-0.571816823242411));
#25616=CARTESIAN_POINT('Ctrl Pts',(-2.06805732997383,1.,-0.567368421181229));
#25617=CARTESIAN_POINT('Ctrl Pts',(-2.06348090160697,1.,-0.562955993082574));
#25618=CARTESIAN_POINT('Ctrl Pts',(-2.05888537756571,1.,-0.558579940185467));
#25619=CARTESIAN_POINT('Ctrl Pts',(-2.05427091604482,1.,-0.554240657464109));
#25620=CARTESIAN_POINT('Ctrl Pts',(-2.04963761077974,1.,-0.549938525150342));
#25621=CARTESIAN_POINT('Ctrl Pts',(-2.0449854471456,1.,-0.545673903817348));
#25622=CARTESIAN_POINT('Ctrl Pts',(-2.0403142269048,1.,-0.54144712061552));
#25623=CARTESIAN_POINT('Ctrl Pts',(-2.03562362953993,1.,-0.537258489833134));
#25624=CARTESIAN_POINT('Ctrl Pts',(-2.03091336214401,1.,-0.533108355132905));
#25625=CARTESIAN_POINT('Ctrl Pts',(-2.02618329083289,1.,-0.52899712724191));
#25626=CARTESIAN_POINT('Ctrl Pts',(-2.02143356304712,1.,-0.524925318333518));
#25627=CARTESIAN_POINT('Ctrl Pts',(-2.01666477917305,1.,-0.520893590399428));
#25628=CARTESIAN_POINT('Ctrl Pts',(-2.01187773939257,1.,-0.516902681728733));
#25629=CARTESIAN_POINT('Ctrl Pts',(-2.00707309946955,1.,-0.512953306961813));
#25630=CARTESIAN_POINT('Ctrl Pts',(-2.00225107134733,1.,-0.509046069886152));
#25631=CARTESIAN_POINT('Ctrl Pts',(-1.99741107463567,1.,-0.505181361323011));
#25632=CARTESIAN_POINT('Ctrl Pts',(-1.9925514912615,1.,-0.501359287727129));
#25633=CARTESIAN_POINT('Ctrl Pts',(-1.98767044752929,1.,-0.497579909545564));
#25634=CARTESIAN_POINT('Ctrl Pts',(-1.9827665876182,1.,-0.493843476541492));
#25635=CARTESIAN_POINT('Ctrl Pts',(-1.97783973019229,1.,-0.490150627860955));
#25636=CARTESIAN_POINT('Ctrl Pts',(-1.97289186263272,1.,-0.486502692907661));
#25637=CARTESIAN_POINT('Ctrl Pts',(-1.96792703422358,1.,-0.482901662120686));
#25638=CARTESIAN_POINT('Ctrl Pts',(-1.96294933055938,1.,-0.479349583074846));
#25639=CARTESIAN_POINT('Ctrl Pts',(-1.95796111148175,1.,-0.475848034683171));
#25640=CARTESIAN_POINT('Ctrl Pts',(-1.95296148278136,1.,-0.472397672264079));
#25641=CARTESIAN_POINT('Ctrl Pts',(-1.94794381136524,1.,-0.468997482913158));
#25642=CARTESIAN_POINT('Ctrl Pts',(-1.94289794196205,1.,-0.465645462026064));
#25643=CARTESIAN_POINT('Ctrl Pts',(-1.93781486640834,1.,-0.462340031009087));
#25644=CARTESIAN_POINT('Ctrl Pts',(-1.93269066517936,1.,-0.459081234547931));
#25645=CARTESIAN_POINT('Ctrl Pts',(-1.92753067150461,1.,-0.455872005174335));
#25646=CARTESIAN_POINT('Ctrl Pts',(-1.9223538064847,1.,-0.452719478359356));
#25647=CARTESIAN_POINT('Ctrl Pts',(-1.91718342555717,1.,-0.449632260106572));
#25648=CARTESIAN_POINT('Ctrl Pts',(-1.91203699981095,1.,-0.446617343485651));
#25649=CARTESIAN_POINT('Ctrl Pts',(-1.90691756144906,1.,-0.44367755684917));
#25650=CARTESIAN_POINT('Ctrl Pts',(-1.90180124389137,1.,-0.44080783370416));
#25651=CARTESIAN_POINT('Ctrl Pts',(-1.89663648956549,1.,-0.437995003948443));
#25652=CARTESIAN_POINT('Ctrl Pts',(-1.89136993975585,1.,-0.43522566096358));
#25653=CARTESIAN_POINT('Ctrl Pts',(-1.88596913666828,1.,-0.432493038548833));
#25654=CARTESIAN_POINT('Ctrl Pts',(-1.88044229001778,1.,-0.429803062482217));
#25655=CARTESIAN_POINT('Ctrl Pts',(-1.87486989291333,1.,-0.427183828518743));
#25656=CARTESIAN_POINT('Ctrl Pts',(-1.8693780394412,1.,-0.424678177290876));
#25657=CARTESIAN_POINT('Ctrl Pts',(-1.86408083333863,1.,-0.422327307417884));
#25658=CARTESIAN_POINT('Ctrl Pts',(-1.8590328109667,1.,-0.420157287975583));
#25659=CARTESIAN_POINT('Ctrl Pts',(-1.8541763285645,1.,-0.418164129144045));
#25660=CARTESIAN_POINT('Ctrl Pts',(-1.84929312930314,1.,-0.416300022039885));
#25661=CARTESIAN_POINT('Ctrl Pts',(-1.84405757074218,1.,-0.414487438255542));
#25662=CARTESIAN_POINT('Ctrl Pts',(-1.8380895347617,1.,-0.412633125322945));
#25663=CARTESIAN_POINT('Ctrl Pts',(-1.83100408895047,1.,-0.410641256301276));
#25664=CARTESIAN_POINT('Ctrl Pts',(-1.82247022677562,1.,-0.408428948106227));
#25665=CARTESIAN_POINT('Ctrl Pts',(-1.81223801812013,1.,-0.405933518407175));
#25666=CARTESIAN_POINT('Ctrl Pts',(-1.80012077173238,1.,-0.403107976163396));
#25667=CARTESIAN_POINT('Ctrl Pts',(-1.78598826343754,1.,-0.399919403774155));
#25668=CARTESIAN_POINT('Ctrl Pts',(-1.76975560043442,1.,-0.396346196110688));
#25669=CARTESIAN_POINT('Ctrl Pts',(-1.75137405310193,1.,-0.392375812285395));
#25670=CARTESIAN_POINT('Ctrl Pts',(-1.73493170972829,1.,-0.388877023502615));
#25671=CARTESIAN_POINT('Ctrl Pts',(-1.72162022244582,1.,-0.386070790323281));
#25672=CARTESIAN_POINT('Ctrl Pts',(-1.71231062891398,1.,-0.384119047314215));
#25673=CARTESIAN_POINT('Ctrl Pts',(-1.7075470150345,1.,-0.383122945602004));
#25674=CARTESIAN_POINT('',(-2.11275013067528,0.,-0.61342227326009));
#25675=CARTESIAN_POINT('Origin',(-2.0698113262342,0.,-0.745574324794401));
#25676=CARTESIAN_POINT('',(-2.0698113262342,1.,-0.745574324794401));
#25677=CARTESIAN_POINT('',(-2.11275013067528,1.,-0.61342227326009));
#25678=CARTESIAN_POINT('',(-2.0698113262342,0.,-0.745574324794401));
#25679=CARTESIAN_POINT('Ctrl Pts',(-1.60662857109684,-1.,-0.693717979106306));
#25680=CARTESIAN_POINT('Ctrl Pts',(-1.60662857109684,1.,-0.693717979106306));
#25681=CARTESIAN_POINT('Ctrl Pts',(-1.61106790958151,-1.,-0.695712097881194));
#25682=CARTESIAN_POINT('Ctrl Pts',(-1.61106790958151,1.,-0.695712097881194));
#25683=CARTESIAN_POINT('Ctrl Pts',(-1.61974673472612,-1.,-0.699605146405088));
#25684=CARTESIAN_POINT('Ctrl Pts',(-1.61974673472612,1.,-0.699605146405088));
#25685=CARTESIAN_POINT('Ctrl Pts',(-1.63216541664676,-1.,-0.705159151988319));
#25686=CARTESIAN_POINT('Ctrl Pts',(-1.63216541664676,1.,-0.705159151988319));
#25687=CARTESIAN_POINT('Ctrl Pts',(-1.64752408832016,-1.,-0.711993139355394));
#25688=CARTESIAN_POINT('Ctrl Pts',(-1.64752408832016,1.,-0.711993139355394));
#25689=CARTESIAN_POINT('Ctrl Pts',(-1.6647288055568,-1.,-0.719585433804282));
#25690=CARTESIAN_POINT('Ctrl Pts',(-1.6647288055568,1.,-0.719585433804282));
#25691=CARTESIAN_POINT('Ctrl Pts',(-1.67996158455503,-1.,-0.726235967997433));
#25692=CARTESIAN_POINT('Ctrl Pts',(-1.67996158455503,1.,-0.726235967997433));
#25693=CARTESIAN_POINT('Ctrl Pts',(-1.69326921975743,-1.,-0.731963238697195));
#25694=CARTESIAN_POINT('Ctrl Pts',(-1.69326921975743,1.,-0.731963238697195));
#25695=CARTESIAN_POINT('Ctrl Pts',(-1.70473309006121,-1.,-0.736799665724771));
#25696=CARTESIAN_POINT('Ctrl Pts',(-1.70473309006121,1.,-0.736799665724771));
#25697=CARTESIAN_POINT('Ctrl Pts',(-1.71447789751927,-1.,-0.740795162032087));
#25698=CARTESIAN_POINT('Ctrl Pts',(-1.71447789751927,1.,-0.740795162032087));
#25699=CARTESIAN_POINT('Ctrl Pts',(-1.7226822991693,-1.,-0.744021445433764));
#25700=CARTESIAN_POINT('Ctrl Pts',(-1.7226822991693,1.,-0.744021445433764));
#25701=CARTESIAN_POINT('Ctrl Pts',(-1.72958533647399,-1.,-0.746574710096436));
#25702=CARTESIAN_POINT('Ctrl Pts',(-1.72958533647399,1.,-0.746574710096436));
#25703=CARTESIAN_POINT('Ctrl Pts',(-1.73550351679848,-1.,-0.748582462954854));
#25704=CARTESIAN_POINT('Ctrl Pts',(-1.73550351679848,1.,-0.748582462954854));
#25705=CARTESIAN_POINT('Ctrl Pts',(-1.74080458266705,-1.,-0.75019343597954));
#25706=CARTESIAN_POINT('Ctrl Pts',(-1.74080458266705,1.,-0.75019343597954));
#25707=CARTESIAN_POINT('Ctrl Pts',(-1.74585086852298,-1.,-0.751555614163629));
#25708=CARTESIAN_POINT('Ctrl Pts',(-1.74585086852298,1.,-0.751555614163629));
#25709=CARTESIAN_POINT('Ctrl Pts',(-1.75095139468809,-1.,-0.752797683531377));
#25710=CARTESIAN_POINT('Ctrl Pts',(-1.75095139468809,1.,-0.752797683531377));
#25711=CARTESIAN_POINT('Ctrl Pts',(-1.75631083600175,-1.,-0.75400925402848));
#25712=CARTESIAN_POINT('Ctrl Pts',(-1.75631083600175,1.,-0.75400925402848));
#25713=CARTESIAN_POINT('Ctrl Pts',(-1.7619781724032,-1.,-0.755220979975262));
#25714=CARTESIAN_POINT('Ctrl Pts',(-1.7619781724032,1.,-0.755220979975262));
#25715=CARTESIAN_POINT('Ctrl Pts',(-1.76789396003141,-1.,-0.756421896028403));
#25716=CARTESIAN_POINT('Ctrl Pts',(-1.76789396003141,1.,-0.756421896028403));
#25717=CARTESIAN_POINT('Ctrl Pts',(-1.77394167108342,-1.,-0.757578264077238));
#25718=CARTESIAN_POINT('Ctrl Pts',(-1.77394167108342,1.,-0.757578264077238));
#25719=CARTESIAN_POINT('Ctrl Pts',(-1.77999411220912,-1.,-0.75865062667738));
#25720=CARTESIAN_POINT('Ctrl Pts',(-1.77999411220912,1.,-0.75865062667738));
#25721=CARTESIAN_POINT('Ctrl Pts',(-1.78596964884526,-1.,-0.759614401109868));
#25722=CARTESIAN_POINT('Ctrl Pts',(-1.78596964884526,1.,-0.759614401109868));
#25723=CARTESIAN_POINT('Ctrl Pts',(-1.79185815610802,-1.,-0.760469555880425));
#25724=CARTESIAN_POINT('Ctrl Pts',(-1.79185815610802,1.,-0.760469555880425));
#25725=CARTESIAN_POINT('Ctrl Pts',(-1.79768986997735,-1.,-0.761229695230359));
#25726=CARTESIAN_POINT('Ctrl Pts',(-1.79768986997735,1.,-0.761229695230359));
#25727=CARTESIAN_POINT('Ctrl Pts',(-1.80351583877334,-1.,-0.761915336443515));
#25728=CARTESIAN_POINT('Ctrl Pts',(-1.80351583877334,1.,-0.761915336443515));
#25729=CARTESIAN_POINT('Ctrl Pts',(-1.80938551463989,-1.,-0.762546129464036));
#25730=CARTESIAN_POINT('Ctrl Pts',(-1.80938551463989,1.,-0.762546129464036));
#25731=CARTESIAN_POINT('Ctrl Pts',(-1.81532118405566,-1.,-0.763132003836783));
#25732=CARTESIAN_POINT('Ctrl Pts',(-1.81532118405566,1.,-0.763132003836783));
#25733=CARTESIAN_POINT('Ctrl Pts',(-1.82131873145297,-1.,-0.763673465462854));
#25734=CARTESIAN_POINT('Ctrl Pts',(-1.82131873145297,1.,-0.763673465462854));
#25735=CARTESIAN_POINT('Ctrl Pts',(-1.8273599120008,-1.,-0.764165902606055));
#25736=CARTESIAN_POINT('Ctrl Pts',(-1.8273599120008,1.,-0.764165902606055));
#25737=CARTESIAN_POINT('Ctrl Pts',(-1.8334207722714,-1.,-0.764602549687845));
#25738=CARTESIAN_POINT('Ctrl Pts',(-1.8334207722714,1.,-0.764602549687845));
#25739=CARTESIAN_POINT('Ctrl Pts',(-1.83948181064823,-1.,-0.764978057881687));
#25740=CARTESIAN_POINT('Ctrl Pts',(-1.83948181064823,1.,-0.764978057881687));
#25741=CARTESIAN_POINT('Ctrl Pts',(-1.8455369887591,-1.,-0.765291664861971));
#25742=CARTESIAN_POINT('Ctrl Pts',(-1.8455369887591,1.,-0.765291664861971));
#25743=CARTESIAN_POINT('Ctrl Pts',(-1.85158945130054,-1.,-0.765545710619023));
#25744=CARTESIAN_POINT('Ctrl Pts',(-1.85158945130054,1.,-0.765545710619023));
#25745=CARTESIAN_POINT('Ctrl Pts',(-1.85764741390391,-1.,-0.765744212909305));
#25746=CARTESIAN_POINT('Ctrl Pts',(-1.85764741390391,1.,-0.765744212909305));
#25747=CARTESIAN_POINT('Ctrl Pts',(-1.86372027063314,-1.,-0.765891519092557));
#25748=CARTESIAN_POINT('Ctrl Pts',(-1.86372027063314,1.,-0.765891519092557));
#25749=CARTESIAN_POINT('Ctrl Pts',(-1.86981398314345,-1.,-0.765990708546111));
#25750=CARTESIAN_POINT('Ctrl Pts',(-1.86981398314345,1.,-0.765990708546111));
#25751=CARTESIAN_POINT('Ctrl Pts',(-1.87592888967886,-1.,-0.766042837036759));
#25752=CARTESIAN_POINT('Ctrl Pts',(-1.87592888967886,1.,-0.766042837036759));
#25753=CARTESIAN_POINT('Ctrl Pts',(-1.88206215302561,-1.,-0.766047794851868));
#25754=CARTESIAN_POINT('Ctrl Pts',(-1.88206215302561,1.,-0.766047794851868));
#25755=CARTESIAN_POINT('Ctrl Pts',(-1.88820926433409,-1.,-0.76600483706209));
#25756=CARTESIAN_POINT('Ctrl Pts',(-1.88820926433409,1.,-0.76600483706209));
#25757=CARTESIAN_POINT('Ctrl Pts',(-1.89436577771389,-1.,-0.765913193856979));
#25758=CARTESIAN_POINT('Ctrl Pts',(-1.89436577771389,1.,-0.765913193856979));
#25759=CARTESIAN_POINT('Ctrl Pts',(-1.90052930393599,-1.,-0.765772772593395));
#25760=CARTESIAN_POINT('Ctrl Pts',(-1.90052930393599,1.,-0.765772772593395));
#25761=CARTESIAN_POINT('Ctrl Pts',(-1.90669961402362,-1.,-0.765584196937936));
#25762=CARTESIAN_POINT('Ctrl Pts',(-1.90669961402362,1.,-0.765584196937936));
#25763=CARTESIAN_POINT('Ctrl Pts',(-1.91287765805174,-1.,-0.765348465884739));
#25764=CARTESIAN_POINT('Ctrl Pts',(-1.91287765805174,1.,-0.765348465884739));
#25765=CARTESIAN_POINT('Ctrl Pts',(-1.91906491634197,-1.,-0.765066729667095));
#25766=CARTESIAN_POINT('Ctrl Pts',(-1.91906491634197,1.,-0.765066729667095));
#25767=CARTESIAN_POINT('Ctrl Pts',(-1.92526263537041,-1.,-0.764740025488189));
#25768=CARTESIAN_POINT('Ctrl Pts',(-1.92526263537041,1.,-0.764740025488189));
#25769=CARTESIAN_POINT('Ctrl Pts',(-1.93147105496367,-1.,-0.764369010673889));
#25770=CARTESIAN_POINT('Ctrl Pts',(-1.93147105496367,1.,-0.764369010673889));
#25771=CARTESIAN_POINT('Ctrl Pts',(-1.93768964875867,-1.,-0.763954049121393));
#25772=CARTESIAN_POINT('Ctrl Pts',(-1.93768964875867,1.,-0.763954049121393));
#25773=CARTESIAN_POINT('Ctrl Pts',(-1.94391746617626,-1.,-0.76349533353858));
#25774=CARTESIAN_POINT('Ctrl Pts',(-1.94391746617626,1.,-0.76349533353858));
#25775=CARTESIAN_POINT('Ctrl Pts',(-1.95015342590025,-1.,-0.762992990878774));
#25776=CARTESIAN_POINT('Ctrl Pts',(-1.95015342590025,1.,-0.762992990878774));
#25777=CARTESIAN_POINT('Ctrl Pts',(-1.95639665309893,-1.,-0.762447203806263));
#25778=CARTESIAN_POINT('Ctrl Pts',(-1.95639665309893,1.,-0.762447203806263));
#25779=CARTESIAN_POINT('Ctrl Pts',(-1.96264672744229,-1.,-0.761858300014575));
#25780=CARTESIAN_POINT('Ctrl Pts',(-1.96264672744229,1.,-0.761858300014575));
#25781=CARTESIAN_POINT('Ctrl Pts',(-1.96890351582545,-1.,-0.761226690483986));
#25782=CARTESIAN_POINT('Ctrl Pts',(-1.96890351582545,1.,-0.761226690483986));
#25783=CARTESIAN_POINT('Ctrl Pts',(-1.97516705321521,-1.,-0.760552825409855));
#25784=CARTESIAN_POINT('Ctrl Pts',(-1.97516705321521,1.,-0.760552825409855));
#25785=CARTESIAN_POINT('Ctrl Pts',(-1.98143741418156,-1.,-0.759837147452135));
#25786=CARTESIAN_POINT('Ctrl Pts',(-1.98143741418156,1.,-0.759837147452135));
#25787=CARTESIAN_POINT('Ctrl Pts',(-1.98771456680806,-1.,-0.759080037802242));
#25788=CARTESIAN_POINT('Ctrl Pts',(-1.98771456680806,1.,-0.759080037802242));
#25789=CARTESIAN_POINT('Ctrl Pts',(-1.9939983109871,-1.,-0.758281796766377));
#25790=CARTESIAN_POINT('Ctrl Pts',(-1.9939983109871,1.,-0.758281796766377));
#25791=CARTESIAN_POINT('Ctrl Pts',(-2.00028834739072,-1.,-0.757442676862341));
#25792=CARTESIAN_POINT('Ctrl Pts',(-2.00028834739072,1.,-0.757442676862341));
#25793=CARTESIAN_POINT('Ctrl Pts',(-2.00658431587682,-1.,-0.756562904646496));
#25794=CARTESIAN_POINT('Ctrl Pts',(-2.00658431587682,1.,-0.756562904646496));
#25795=CARTESIAN_POINT('Ctrl Pts',(-2.01288584328149,-1.,-0.7556427049581));
#25796=CARTESIAN_POINT('Ctrl Pts',(-2.01288584328149,1.,-0.7556427049581));
#25797=CARTESIAN_POINT('Ctrl Pts',(-2.01919259406003,-1.,-0.75468233072352));
#25798=CARTESIAN_POINT('Ctrl Pts',(-2.01919259406003,1.,-0.75468233072352));
#25799=CARTESIAN_POINT('Ctrl Pts',(-2.02550428623587,-1.,-0.753682061113765));
#25800=CARTESIAN_POINT('Ctrl Pts',(-2.02550428623587,1.,-0.753682061113765));
#25801=CARTESIAN_POINT('Ctrl Pts',(-2.03182068456467,-1.,-0.752642180488104));
#25802=CARTESIAN_POINT('Ctrl Pts',(-2.03182068456467,1.,-0.752642180488104));
#25803=CARTESIAN_POINT('Ctrl Pts',(-2.03814160092173,-1.,-0.751562963361383));
#25804=CARTESIAN_POINT('Ctrl Pts',(-2.03814160092173,1.,-0.751562963361383));
#25805=CARTESIAN_POINT('Ctrl Pts',(-2.04446689147754,-1.,-0.750444657874758));
#25806=CARTESIAN_POINT('Ctrl Pts',(-2.04446689147754,1.,-0.750444657874758));
#25807=CARTESIAN_POINT('Ctrl Pts',(-2.05079645591606,-1.,-0.749287468663053));
#25808=CARTESIAN_POINT('Ctrl Pts',(-2.05079645591606,1.,-0.749287468663053));
#25809=CARTESIAN_POINT('Ctrl Pts',(-2.05713023030263,-1.,-0.748091554181101));
#25810=CARTESIAN_POINT('Ctrl Pts',(-2.05713023030263,1.,-0.748091554181101));
#25811=CARTESIAN_POINT('Ctrl Pts',(-2.06220058927162,-1.,-0.747103932785504));
#25812=CARTESIAN_POINT('Ctrl Pts',(-2.06220058927162,1.,-0.747103932785504));
#25813=CARTESIAN_POINT('Ctrl Pts',(-2.06600523016401,-1.,-0.746345871542695));
#25814=CARTESIAN_POINT('Ctrl Pts',(-2.06600523016401,1.,-0.746345871542695));
#25815=CARTESIAN_POINT('Ctrl Pts',(-2.06854248895575,-1.,-0.74583279137781));
#25816=CARTESIAN_POINT('Ctrl Pts',(-2.06854248895575,1.,-0.74583279137781));
#25817=CARTESIAN_POINT('Ctrl Pts',(-2.0698113262342,-1.,-0.745574324794401));
#25818=CARTESIAN_POINT('Ctrl Pts',(-2.0698113262342,1.,-0.745574324794401));
#25819=CARTESIAN_POINT('',(-1.60662857109684,1.,-0.693717979106306));
#25820=CARTESIAN_POINT('Ctrl Pts',(-1.60662857109684,1.,-0.693717979106306));
#25821=CARTESIAN_POINT('Ctrl Pts',(-1.61106790958151,1.,-0.695712097881194));
#25822=CARTESIAN_POINT('Ctrl Pts',(-1.61974673472612,1.,-0.699605146405088));
#25823=CARTESIAN_POINT('Ctrl Pts',(-1.63216541664676,1.,-0.705159151988319));
#25824=CARTESIAN_POINT('Ctrl Pts',(-1.64752408832016,1.,-0.711993139355394));
#25825=CARTESIAN_POINT('Ctrl Pts',(-1.6647288055568,1.,-0.719585433804282));
#25826=CARTESIAN_POINT('Ctrl Pts',(-1.67996158455503,1.,-0.726235967997433));
#25827=CARTESIAN_POINT('Ctrl Pts',(-1.69326921975743,1.,-0.731963238697195));
#25828=CARTESIAN_POINT('Ctrl Pts',(-1.70473309006121,1.,-0.736799665724771));
#25829=CARTESIAN_POINT('Ctrl Pts',(-1.71447789751927,1.,-0.740795162032087));
#25830=CARTESIAN_POINT('Ctrl Pts',(-1.7226822991693,1.,-0.744021445433764));
#25831=CARTESIAN_POINT('Ctrl Pts',(-1.72958533647399,1.,-0.746574710096436));
#25832=CARTESIAN_POINT('Ctrl Pts',(-1.73550351679848,1.,-0.748582462954854));
#25833=CARTESIAN_POINT('Ctrl Pts',(-1.74080458266705,1.,-0.75019343597954));
#25834=CARTESIAN_POINT('Ctrl Pts',(-1.74585086852298,1.,-0.751555614163629));
#25835=CARTESIAN_POINT('Ctrl Pts',(-1.75095139468809,1.,-0.752797683531377));
#25836=CARTESIAN_POINT('Ctrl Pts',(-1.75631083600175,1.,-0.75400925402848));
#25837=CARTESIAN_POINT('Ctrl Pts',(-1.7619781724032,1.,-0.755220979975262));
#25838=CARTESIAN_POINT('Ctrl Pts',(-1.76789396003141,1.,-0.756421896028403));
#25839=CARTESIAN_POINT('Ctrl Pts',(-1.77394167108342,1.,-0.757578264077238));
#25840=CARTESIAN_POINT('Ctrl Pts',(-1.77999411220912,1.,-0.75865062667738));
#25841=CARTESIAN_POINT('Ctrl Pts',(-1.78596964884526,1.,-0.759614401109868));
#25842=CARTESIAN_POINT('Ctrl Pts',(-1.79185815610802,1.,-0.760469555880425));
#25843=CARTESIAN_POINT('Ctrl Pts',(-1.79768986997735,1.,-0.761229695230359));
#25844=CARTESIAN_POINT('Ctrl Pts',(-1.80351583877334,1.,-0.761915336443515));
#25845=CARTESIAN_POINT('Ctrl Pts',(-1.80938551463989,1.,-0.762546129464036));
#25846=CARTESIAN_POINT('Ctrl Pts',(-1.81532118405566,1.,-0.763132003836783));
#25847=CARTESIAN_POINT('Ctrl Pts',(-1.82131873145297,1.,-0.763673465462854));
#25848=CARTESIAN_POINT('Ctrl Pts',(-1.8273599120008,1.,-0.764165902606055));
#25849=CARTESIAN_POINT('Ctrl Pts',(-1.8334207722714,1.,-0.764602549687845));
#25850=CARTESIAN_POINT('Ctrl Pts',(-1.83948181064823,1.,-0.764978057881687));
#25851=CARTESIAN_POINT('Ctrl Pts',(-1.8455369887591,1.,-0.765291664861971));
#25852=CARTESIAN_POINT('Ctrl Pts',(-1.85158945130054,1.,-0.765545710619023));
#25853=CARTESIAN_POINT('Ctrl Pts',(-1.85764741390391,1.,-0.765744212909305));
#25854=CARTESIAN_POINT('Ctrl Pts',(-1.86372027063314,1.,-0.765891519092557));
#25855=CARTESIAN_POINT('Ctrl Pts',(-1.86981398314345,1.,-0.765990708546111));
#25856=CARTESIAN_POINT('Ctrl Pts',(-1.87592888967886,1.,-0.766042837036759));
#25857=CARTESIAN_POINT('Ctrl Pts',(-1.88206215302561,1.,-0.766047794851868));
#25858=CARTESIAN_POINT('Ctrl Pts',(-1.88820926433409,1.,-0.76600483706209));
#25859=CARTESIAN_POINT('Ctrl Pts',(-1.89436577771389,1.,-0.765913193856979));
#25860=CARTESIAN_POINT('Ctrl Pts',(-1.90052930393599,1.,-0.765772772593395));
#25861=CARTESIAN_POINT('Ctrl Pts',(-1.90669961402362,1.,-0.765584196937936));
#25862=CARTESIAN_POINT('Ctrl Pts',(-1.91287765805174,1.,-0.765348465884739));
#25863=CARTESIAN_POINT('Ctrl Pts',(-1.91906491634197,1.,-0.765066729667095));
#25864=CARTESIAN_POINT('Ctrl Pts',(-1.92526263537041,1.,-0.764740025488189));
#25865=CARTESIAN_POINT('Ctrl Pts',(-1.93147105496367,1.,-0.764369010673889));
#25866=CARTESIAN_POINT('Ctrl Pts',(-1.93768964875867,1.,-0.763954049121393));
#25867=CARTESIAN_POINT('Ctrl Pts',(-1.94391746617626,1.,-0.76349533353858));
#25868=CARTESIAN_POINT('Ctrl Pts',(-1.95015342590025,1.,-0.762992990878774));
#25869=CARTESIAN_POINT('Ctrl Pts',(-1.95639665309893,1.,-0.762447203806263));
#25870=CARTESIAN_POINT('Ctrl Pts',(-1.96264672744229,1.,-0.761858300014575));
#25871=CARTESIAN_POINT('Ctrl Pts',(-1.96890351582545,1.,-0.761226690483986));
#25872=CARTESIAN_POINT('Ctrl Pts',(-1.97516705321521,1.,-0.760552825409855));
#25873=CARTESIAN_POINT('Ctrl Pts',(-1.98143741418156,1.,-0.759837147452135));
#25874=CARTESIAN_POINT('Ctrl Pts',(-1.98771456680806,1.,-0.759080037802242));
#25875=CARTESIAN_POINT('Ctrl Pts',(-1.9939983109871,1.,-0.758281796766377));
#25876=CARTESIAN_POINT('Ctrl Pts',(-2.00028834739072,1.,-0.757442676862341));
#25877=CARTESIAN_POINT('Ctrl Pts',(-2.00658431587682,1.,-0.756562904646496));
#25878=CARTESIAN_POINT('Ctrl Pts',(-2.01288584328149,1.,-0.7556427049581));
#25879=CARTESIAN_POINT('Ctrl Pts',(-2.01919259406003,1.,-0.75468233072352));
#25880=CARTESIAN_POINT('Ctrl Pts',(-2.02550428623587,1.,-0.753682061113765));
#25881=CARTESIAN_POINT('Ctrl Pts',(-2.03182068456467,1.,-0.752642180488104));
#25882=CARTESIAN_POINT('Ctrl Pts',(-2.03814160092173,1.,-0.751562963361383));
#25883=CARTESIAN_POINT('Ctrl Pts',(-2.04446689147754,1.,-0.750444657874758));
#25884=CARTESIAN_POINT('Ctrl Pts',(-2.05079645591606,1.,-0.749287468663053));
#25885=CARTESIAN_POINT('Ctrl Pts',(-2.05713023030263,1.,-0.748091554181101));
#25886=CARTESIAN_POINT('Ctrl Pts',(-2.06220058927162,1.,-0.747103932785504));
#25887=CARTESIAN_POINT('Ctrl Pts',(-2.06600523016401,1.,-0.746345871542695));
#25888=CARTESIAN_POINT('Ctrl Pts',(-2.06854248895575,1.,-0.74583279137781));
#25889=CARTESIAN_POINT('Ctrl Pts',(-2.0698113262342,1.,-0.745574324794401));
#25890=CARTESIAN_POINT('',(-1.60662857109684,0.,-0.693717979106306));
#25891=CARTESIAN_POINT('Origin',(0.,0.,0.));
#25892=CARTESIAN_POINT('',(-1.5055822144029,1.,-0.892032620296855));
#25893=CARTESIAN_POINT('Origin',(0.,1.,0.));
#25894=CARTESIAN_POINT('',(-1.5055822144029,0.,-0.892032620296855));
#25895=CARTESIAN_POINT('Ctrl Pts',(-1.81978687191668,-1.,-1.23627494547115));
#25896=CARTESIAN_POINT('Ctrl Pts',(-1.81978687191668,1.,-1.23627494547115));
#25897=CARTESIAN_POINT('Ctrl Pts',(-1.81925017193666,-1.,-1.23509651170476));
#25898=CARTESIAN_POINT('Ctrl Pts',(-1.81925017193666,1.,-1.23509651170476));
#25899=CARTESIAN_POINT('Ctrl Pts',(-1.81817389921279,-1.,-1.2327422452705));
#25900=CARTESIAN_POINT('Ctrl Pts',(-1.81817389921279,1.,-1.2327422452705));
#25901=CARTESIAN_POINT('Ctrl Pts',(-1.8165508718364,-1.,-1.2292186489137));
#25902=CARTESIAN_POINT('Ctrl Pts',(-1.8165508718364,1.,-1.2292186489137));
#25903=CARTESIAN_POINT('Ctrl Pts',(-1.81436959210434,-1.,-1.2245361330495));
#25904=CARTESIAN_POINT('Ctrl Pts',(-1.81436959210434,1.,-1.2245361330495));
#25905=CARTESIAN_POINT('Ctrl Pts',(-1.81161420806656,-1.,-1.21870906103557));
#25906=CARTESIAN_POINT('Ctrl Pts',(-1.81161420806656,1.,-1.21870906103557));
#25907=CARTESIAN_POINT('Ctrl Pts',(-1.80882996917129,-1.,-1.21290815708314));
#25908=CARTESIAN_POINT('Ctrl Pts',(-1.80882996917129,1.,-1.21290815708314));
#25909=CARTESIAN_POINT('Ctrl Pts',(-1.80601678480707,-1.,-1.20713356605475));
#25910=CARTESIAN_POINT('Ctrl Pts',(-1.80601678480707,1.,-1.20713356605475));
#25911=CARTESIAN_POINT('Ctrl Pts',(-1.80317454838603,-1.,-1.20138548938974));
#25912=CARTESIAN_POINT('Ctrl Pts',(-1.80317454838603,1.,-1.20138548938974));
#25913=CARTESIAN_POINT('Ctrl Pts',(-1.80030314369879,-1.,-1.19566418930242));
#25914=CARTESIAN_POINT('Ctrl Pts',(-1.80030314369879,1.,-1.19566418930242));
#25915=CARTESIAN_POINT('Ctrl Pts',(-1.79740245923478,-1.,-1.18996997934445));
#25916=CARTESIAN_POINT('Ctrl Pts',(-1.79740245923478,1.,-1.18996997934445));
#25917=CARTESIAN_POINT('Ctrl Pts',(-1.79447240321515,-1.,-1.18430321697432));
#25918=CARTESIAN_POINT('Ctrl Pts',(-1.79447240321515,1.,-1.18430321697432));
#25919=CARTESIAN_POINT('Ctrl Pts',(-1.79151291552689,-1.,-1.17866429440809));
#25920=CARTESIAN_POINT('Ctrl Pts',(-1.79151291552689,1.,-1.17866429440809));
#25921=CARTESIAN_POINT('Ctrl Pts',(-1.78852398877616,-1.,-1.17305363177328));
#25922=CARTESIAN_POINT('Ctrl Pts',(-1.78852398877616,1.,-1.17305363177328));
#25923=CARTESIAN_POINT('Ctrl Pts',(-1.78550566040443,-1.,-1.16747166312303));
#25924=CARTESIAN_POINT('Ctrl Pts',(-1.78550566040443,1.,-1.16747166312303));
#25925=CARTESIAN_POINT('Ctrl Pts',(-1.78245795881009,-1.,-1.16191881298499));
#25926=CARTESIAN_POINT('Ctrl Pts',(-1.78245795881009,1.,-1.16191881298499));
#25927=CARTESIAN_POINT('Ctrl Pts',(-1.77938085564275,-1.,-1.15639547194698));
#25928=CARTESIAN_POINT('Ctrl Pts',(-1.77938085564275,1.,-1.15639547194698));
#25929=CARTESIAN_POINT('Ctrl Pts',(-1.7762742255701,-1.,-1.15090197841515));
#25930=CARTESIAN_POINT('Ctrl Pts',(-1.7762742255701,1.,-1.15090197841515));
#25931=CARTESIAN_POINT('Ctrl Pts',(-1.77313777896194,-1.,-1.1454385822692));
#25932=CARTESIAN_POINT('Ctrl Pts',(-1.77313777896194,1.,-1.1454385822692));
#25933=CARTESIAN_POINT('Ctrl Pts',(-1.76997111386769,-1.,-1.14000548336975));
#25934=CARTESIAN_POINT('Ctrl Pts',(-1.76997111386769,1.,-1.14000548336975));
#25935=CARTESIAN_POINT('Ctrl Pts',(-1.76677384551862,-1.,-1.1346029180462));
#25936=CARTESIAN_POINT('Ctrl Pts',(-1.76677384551862,1.,-1.1346029180462));
#25937=CARTESIAN_POINT('Ctrl Pts',(-1.7635457196617,-1.,-1.12923123555075));
#25938=CARTESIAN_POINT('Ctrl Pts',(-1.7635457196617,1.,-1.12923123555075));
#25939=CARTESIAN_POINT('Ctrl Pts',(-1.76028671825096,-1.,-1.12389096855086));
#25940=CARTESIAN_POINT('Ctrl Pts',(-1.76028671825096,1.,-1.12389096855086));
#25941=CARTESIAN_POINT('Ctrl Pts',(-1.75699720772105,-1.,-1.11858293216763));
#25942=CARTESIAN_POINT('Ctrl Pts',(-1.75699720772105,1.,-1.11858293216763));
#25943=CARTESIAN_POINT('Ctrl Pts',(-1.7536777209463,-1.,-1.11330807582551));
#25944=CARTESIAN_POINT('Ctrl Pts',(-1.7536777209463,1.,-1.11330807582551));
#25945=CARTESIAN_POINT('Ctrl Pts',(-1.7503286607592,-1.,-1.10806728183007));
#25946=CARTESIAN_POINT('Ctrl Pts',(-1.7503286607592,1.,-1.10806728183007));
#25947=CARTESIAN_POINT('Ctrl Pts',(-1.74695004214923,-1.,-1.10286118991143));
#25948=CARTESIAN_POINT('Ctrl Pts',(-1.74695004214923,1.,-1.10286118991143));
#25949=CARTESIAN_POINT('Ctrl Pts',(-1.74354119236208,-1.,-1.09768999241225));
#25950=CARTESIAN_POINT('Ctrl Pts',(-1.74354119236208,1.,-1.09768999241225));
#25951=CARTESIAN_POINT('Ctrl Pts',(-1.74010053962247,-1.,-1.09255329056493));
#25952=CARTESIAN_POINT('Ctrl Pts',(-1.74010053962247,1.,-1.09255329056493));
#25953=CARTESIAN_POINT('Ctrl Pts',(-1.73662628326091,-1.,-1.08745056285427));
#25954=CARTESIAN_POINT('Ctrl Pts',(-1.73662628326091,1.,-1.08745056285427));
#25955=CARTESIAN_POINT('Ctrl Pts',(-1.73311705663407,-1.,-1.08238162784749));
#25956=CARTESIAN_POINT('Ctrl Pts',(-1.73311705663407,1.,-1.08238162784749));
#25957=CARTESIAN_POINT('Ctrl Pts',(-1.72957248977424,-1.,-1.0773470373727));
#25958=CARTESIAN_POINT('Ctrl Pts',(-1.72957248977424,1.,-1.0773470373727));
#25959=CARTESIAN_POINT('Ctrl Pts',(-1.72599406198488,-1.,-1.07234866990252));
#25960=CARTESIAN_POINT('Ctrl Pts',(-1.72599406198488,1.,-1.07234866990252));
#25961=CARTESIAN_POINT('Ctrl Pts',(-1.72238500928453,-1.,-1.06738966975462));
#25962=CARTESIAN_POINT('Ctrl Pts',(-1.72238500928453,1.,-1.06738966975462));
#25963=CARTESIAN_POINT('Ctrl Pts',(-1.71874858456904,-1.,-1.06247324680647));
#25964=CARTESIAN_POINT('Ctrl Pts',(-1.71874858456904,1.,-1.06247324680647));
#25965=CARTESIAN_POINT('Ctrl Pts',(-1.7150865442702,-1.,-1.05760163192479));
#25966=CARTESIAN_POINT('Ctrl Pts',(-1.7150865442702,1.,-1.05760163192479));
#25967=CARTESIAN_POINT('Ctrl Pts',(-1.71139783543989,-1.,-1.05277517202855));
#25968=CARTESIAN_POINT('Ctrl Pts',(-1.71139783543989,1.,-1.05277517202855));
#25969=CARTESIAN_POINT('Ctrl Pts',(-1.70767646263649,-1.,-1.04799085404995));
#25970=CARTESIAN_POINT('Ctrl Pts',(-1.70767646263649,1.,-1.04799085404995));
#25971=CARTESIAN_POINT('Ctrl Pts',(-1.70391338707982,-1.,-1.04324363334554));
#25972=CARTESIAN_POINT('Ctrl Pts',(-1.70391338707982,1.,-1.04324363334554));
#25973=CARTESIAN_POINT('Ctrl Pts',(-1.70010052930962,-1.,-1.03852922490789));
#25974=CARTESIAN_POINT('Ctrl Pts',(-1.70010052930962,1.,-1.03852922490789));
#25975=CARTESIAN_POINT('Ctrl Pts',(-1.69623414782771,-1.,-1.03384646003588));
#25976=CARTESIAN_POINT('Ctrl Pts',(-1.69623414782771,1.,-1.03384646003588));
#25977=CARTESIAN_POINT('Ctrl Pts',(-1.69231840863458,-1.,-1.02919977579147));
#25978=CARTESIAN_POINT('Ctrl Pts',(-1.69231840863458,1.,-1.02919977579147));
#25979=CARTESIAN_POINT('Ctrl Pts',(-1.68836910178447,-1.,-1.02460180535255));
#25980=CARTESIAN_POINT('Ctrl Pts',(-1.68836910178447,1.,-1.02460180535255));
#25981=CARTESIAN_POINT('Ctrl Pts',(-1.68440578021706,-1.,-1.02006795074201));
#25982=CARTESIAN_POINT('Ctrl Pts',(-1.68440578021706,1.,-1.02006795074201));
#25983=CARTESIAN_POINT('Ctrl Pts',(-1.68044289894798,-1.,-1.01561026162773));
#25984=CARTESIAN_POINT('Ctrl Pts',(-1.68044289894798,1.,-1.01561026162773));
#25985=CARTESIAN_POINT('Ctrl Pts',(-1.67648246776464,-1.,-1.01123236493511));
#25986=CARTESIAN_POINT('Ctrl Pts',(-1.67648246776464,1.,-1.01123236493511));
#25987=CARTESIAN_POINT('Ctrl Pts',(-1.67250335383293,-1.,-1.00692206696414));
#25988=CARTESIAN_POINT('Ctrl Pts',(-1.67250335383293,1.,-1.00692206696414));
#25989=CARTESIAN_POINT('Ctrl Pts',(-1.66846059277303,-1.,-1.00265091003727));
#25990=CARTESIAN_POINT('Ctrl Pts',(-1.66846059277303,1.,-1.00265091003727));
#25991=CARTESIAN_POINT('Ctrl Pts',(-1.66430758030376,-1.,-0.998389654952758));
#25992=CARTESIAN_POINT('Ctrl Pts',(-1.66430758030376,1.,-0.998389654952758));
#25993=CARTESIAN_POINT('Ctrl Pts',(-1.66001553809947,-1.,-0.994121836661306));
#25994=CARTESIAN_POINT('Ctrl Pts',(-1.66001553809947,1.,-0.994121836661306));
#25995=CARTESIAN_POINT('Ctrl Pts',(-1.65559044289699,-1.,-0.989855627854165));
#25996=CARTESIAN_POINT('Ctrl Pts',(-1.65559044289699,1.,-0.989855627854165));
#25997=CARTESIAN_POINT('Ctrl Pts',(-1.65110016612638,-1.,-0.985642622920821));
#25998=CARTESIAN_POINT('Ctrl Pts',(-1.65110016612638,1.,-0.985642622920821));
#25999=CARTESIAN_POINT('Ctrl Pts',(-1.64665139190656,-1.,-0.981562530939489));
#26000=CARTESIAN_POINT('Ctrl Pts',(-1.64665139190656,1.,-0.981562530939489));
#26001=CARTESIAN_POINT('Ctrl Pts',(-1.64233990826687,-1.,-0.977689794119416));
#26002=CARTESIAN_POINT('Ctrl Pts',(-1.64233990826687,1.,-0.977689794119416));
#26003=CARTESIAN_POINT('Ctrl Pts',(-1.63820952658144,-1.,-0.974066058287418));
#26004=CARTESIAN_POINT('Ctrl Pts',(-1.63820952658144,1.,-0.974066058287418));
#26005=CARTESIAN_POINT('Ctrl Pts',(-1.63420665729798,-1.,-0.970669715997509));
#26006=CARTESIAN_POINT('Ctrl Pts',(-1.63420665729798,1.,-0.970669715997509));
#26007=CARTESIAN_POINT('Ctrl Pts',(-1.63013849959461,-1.,-0.967387853230345));
#26008=CARTESIAN_POINT('Ctrl Pts',(-1.63013849959461,1.,-0.967387853230345));
#26009=CARTESIAN_POINT('Ctrl Pts',(-1.62571930670187,-1.,-0.964046107040536));
#26010=CARTESIAN_POINT('Ctrl Pts',(-1.62571930670187,1.,-0.964046107040536));
#26011=CARTESIAN_POINT('Ctrl Pts',(-1.62061638140221,-1.,-0.960438326101729));
#26012=CARTESIAN_POINT('Ctrl Pts',(-1.62061638140221,1.,-0.960438326101729));
#26013=CARTESIAN_POINT('Ctrl Pts',(-1.61449324337085,-1.,-0.956354422920671));
#26014=CARTESIAN_POINT('Ctrl Pts',(-1.61449324337085,1.,-0.956354422920671));
#26015=CARTESIAN_POINT('Ctrl Pts',(-1.60706069896936,-1.,-0.951613284356035));
#26016=CARTESIAN_POINT('Ctrl Pts',(-1.60706069896936,1.,-0.951613284356035));
#26017=CARTESIAN_POINT('Ctrl Pts',(-1.59810042043673,-1.,-0.946078063315257));
#26018=CARTESIAN_POINT('Ctrl Pts',(-1.59810042043673,1.,-0.946078063315257));
#26019=CARTESIAN_POINT('Ctrl Pts',(-1.58744937487176,-1.,-0.939646377893399));
#26020=CARTESIAN_POINT('Ctrl Pts',(-1.58744937487176,1.,-0.939646377893399));
#26021=CARTESIAN_POINT('Ctrl Pts',(-1.57499388382243,-1.,-0.932246680108685));
#26022=CARTESIAN_POINT('Ctrl Pts',(-1.57499388382243,1.,-0.932246680108685));
#26023=CARTESIAN_POINT('Ctrl Pts',(-1.56065988578893,-1.,-0.923832188944341));
#26024=CARTESIAN_POINT('Ctrl Pts',(-1.56065988578893,1.,-0.923832188944341));
#26025=CARTESIAN_POINT('Ctrl Pts',(-1.54440491149498,-1.,-0.914375919026456));
#26026=CARTESIAN_POINT('Ctrl Pts',(-1.54440491149498,1.,-0.914375919026456));
#26027=CARTESIAN_POINT('Ctrl Pts',(-1.52984849887993,-1.,-0.905967409625651));
#26028=CARTESIAN_POINT('Ctrl Pts',(-1.52984849887993,1.,-0.905967409625651));
#26029=CARTESIAN_POINT('Ctrl Pts',(-1.51805569590094,-1.,-0.899185047483511));
#26030=CARTESIAN_POINT('Ctrl Pts',(-1.51805569590094,1.,-0.899185047483511));
#26031=CARTESIAN_POINT('Ctrl Pts',(-1.50980486806688,-1.,-0.894452006964543));
#26032=CARTESIAN_POINT('Ctrl Pts',(-1.50980486806688,1.,-0.894452006964543));
#26033=CARTESIAN_POINT('Ctrl Pts',(-1.5055822144029,-1.,-0.892032620296855));
#26034=CARTESIAN_POINT('Ctrl Pts',(-1.5055822144029,1.,-0.892032620296855));
#26035=CARTESIAN_POINT('',(-1.81978687191668,1.,-1.23627494547115));
#26036=CARTESIAN_POINT('Ctrl Pts',(-1.81978687191668,1.,-1.23627494547115));
#26037=CARTESIAN_POINT('Ctrl Pts',(-1.81925017193666,1.,-1.23509651170476));
#26038=CARTESIAN_POINT('Ctrl Pts',(-1.81817389921279,1.,-1.2327422452705));
#26039=CARTESIAN_POINT('Ctrl Pts',(-1.8165508718364,1.,-1.2292186489137));
#26040=CARTESIAN_POINT('Ctrl Pts',(-1.81436959210434,1.,-1.2245361330495));
#26041=CARTESIAN_POINT('Ctrl Pts',(-1.81161420806656,1.,-1.21870906103557));
#26042=CARTESIAN_POINT('Ctrl Pts',(-1.80882996917129,1.,-1.21290815708314));
#26043=CARTESIAN_POINT('Ctrl Pts',(-1.80601678480707,1.,-1.20713356605475));
#26044=CARTESIAN_POINT('Ctrl Pts',(-1.80317454838603,1.,-1.20138548938974));
#26045=CARTESIAN_POINT('Ctrl Pts',(-1.80030314369879,1.,-1.19566418930242));
#26046=CARTESIAN_POINT('Ctrl Pts',(-1.79740245923478,1.,-1.18996997934445));
#26047=CARTESIAN_POINT('Ctrl Pts',(-1.79447240321515,1.,-1.18430321697432));
#26048=CARTESIAN_POINT('Ctrl Pts',(-1.79151291552689,1.,-1.17866429440809));
#26049=CARTESIAN_POINT('Ctrl Pts',(-1.78852398877616,1.,-1.17305363177328));
#26050=CARTESIAN_POINT('Ctrl Pts',(-1.78550566040443,1.,-1.16747166312303));
#26051=CARTESIAN_POINT('Ctrl Pts',(-1.78245795881009,1.,-1.16191881298499));
#26052=CARTESIAN_POINT('Ctrl Pts',(-1.77938085564275,1.,-1.15639547194698));
#26053=CARTESIAN_POINT('Ctrl Pts',(-1.7762742255701,1.,-1.15090197841515));
#26054=CARTESIAN_POINT('Ctrl Pts',(-1.77313777896194,1.,-1.1454385822692));
#26055=CARTESIAN_POINT('Ctrl Pts',(-1.76997111386769,1.,-1.14000548336975));
#26056=CARTESIAN_POINT('Ctrl Pts',(-1.76677384551862,1.,-1.1346029180462));
#26057=CARTESIAN_POINT('Ctrl Pts',(-1.7635457196617,1.,-1.12923123555075));
#26058=CARTESIAN_POINT('Ctrl Pts',(-1.76028671825096,1.,-1.12389096855086));
#26059=CARTESIAN_POINT('Ctrl Pts',(-1.75699720772105,1.,-1.11858293216763));
#26060=CARTESIAN_POINT('Ctrl Pts',(-1.7536777209463,1.,-1.11330807582551));
#26061=CARTESIAN_POINT('Ctrl Pts',(-1.7503286607592,1.,-1.10806728183007));
#26062=CARTESIAN_POINT('Ctrl Pts',(-1.74695004214923,1.,-1.10286118991143));
#26063=CARTESIAN_POINT('Ctrl Pts',(-1.74354119236208,1.,-1.09768999241225));
#26064=CARTESIAN_POINT('Ctrl Pts',(-1.74010053962247,1.,-1.09255329056493));
#26065=CARTESIAN_POINT('Ctrl Pts',(-1.73662628326091,1.,-1.08745056285427));
#26066=CARTESIAN_POINT('Ctrl Pts',(-1.73311705663407,1.,-1.08238162784749));
#26067=CARTESIAN_POINT('Ctrl Pts',(-1.72957248977424,1.,-1.0773470373727));
#26068=CARTESIAN_POINT('Ctrl Pts',(-1.72599406198488,1.,-1.07234866990252));
#26069=CARTESIAN_POINT('Ctrl Pts',(-1.72238500928453,1.,-1.06738966975462));
#26070=CARTESIAN_POINT('Ctrl Pts',(-1.71874858456904,1.,-1.06247324680647));
#26071=CARTESIAN_POINT('Ctrl Pts',(-1.7150865442702,1.,-1.05760163192479));
#26072=CARTESIAN_POINT('Ctrl Pts',(-1.71139783543989,1.,-1.05277517202855));
#26073=CARTESIAN_POINT('Ctrl Pts',(-1.70767646263649,1.,-1.04799085404995));
#26074=CARTESIAN_POINT('Ctrl Pts',(-1.70391338707982,1.,-1.04324363334554));
#26075=CARTESIAN_POINT('Ctrl Pts',(-1.70010052930962,1.,-1.03852922490789));
#26076=CARTESIAN_POINT('Ctrl Pts',(-1.69623414782771,1.,-1.03384646003588));
#26077=CARTESIAN_POINT('Ctrl Pts',(-1.69231840863458,1.,-1.02919977579147));
#26078=CARTESIAN_POINT('Ctrl Pts',(-1.68836910178447,1.,-1.02460180535255));
#26079=CARTESIAN_POINT('Ctrl Pts',(-1.68440578021706,1.,-1.02006795074201));
#26080=CARTESIAN_POINT('Ctrl Pts',(-1.68044289894798,1.,-1.01561026162773));
#26081=CARTESIAN_POINT('Ctrl Pts',(-1.67648246776464,1.,-1.01123236493511));
#26082=CARTESIAN_POINT('Ctrl Pts',(-1.67250335383293,1.,-1.00692206696414));
#26083=CARTESIAN_POINT('Ctrl Pts',(-1.66846059277303,1.,-1.00265091003727));
#26084=CARTESIAN_POINT('Ctrl Pts',(-1.66430758030376,1.,-0.998389654952758));
#26085=CARTESIAN_POINT('Ctrl Pts',(-1.66001553809947,1.,-0.994121836661306));
#26086=CARTESIAN_POINT('Ctrl Pts',(-1.65559044289699,1.,-0.989855627854165));
#26087=CARTESIAN_POINT('Ctrl Pts',(-1.65110016612638,1.,-0.985642622920821));
#26088=CARTESIAN_POINT('Ctrl Pts',(-1.64665139190656,1.,-0.981562530939489));
#26089=CARTESIAN_POINT('Ctrl Pts',(-1.64233990826687,1.,-0.977689794119416));
#26090=CARTESIAN_POINT('Ctrl Pts',(-1.63820952658144,1.,-0.974066058287418));
#26091=CARTESIAN_POINT('Ctrl Pts',(-1.63420665729798,1.,-0.970669715997509));
#26092=CARTESIAN_POINT('Ctrl Pts',(-1.63013849959461,1.,-0.967387853230345));
#26093=CARTESIAN_POINT('Ctrl Pts',(-1.62571930670187,1.,-0.964046107040536));
#26094=CARTESIAN_POINT('Ctrl Pts',(-1.62061638140221,1.,-0.960438326101729));
#26095=CARTESIAN_POINT('Ctrl Pts',(-1.61449324337085,1.,-0.956354422920671));
#26096=CARTESIAN_POINT('Ctrl Pts',(-1.60706069896936,1.,-0.951613284356035));
#26097=CARTESIAN_POINT('Ctrl Pts',(-1.59810042043673,1.,-0.946078063315257));
#26098=CARTESIAN_POINT('Ctrl Pts',(-1.58744937487176,1.,-0.939646377893399));
#26099=CARTESIAN_POINT('Ctrl Pts',(-1.57499388382243,1.,-0.932246680108685));
#26100=CARTESIAN_POINT('Ctrl Pts',(-1.56065988578893,1.,-0.923832188944341));
#26101=CARTESIAN_POINT('Ctrl Pts',(-1.54440491149498,1.,-0.914375919026456));
#26102=CARTESIAN_POINT('Ctrl Pts',(-1.52984849887993,1.,-0.905967409625651));
#26103=CARTESIAN_POINT('Ctrl Pts',(-1.51805569590094,1.,-0.899185047483511));
#26104=CARTESIAN_POINT('Ctrl Pts',(-1.50980486806688,1.,-0.894452006964543));
#26105=CARTESIAN_POINT('Ctrl Pts',(-1.5055822144029,1.,-0.892032620296855));
#26106=CARTESIAN_POINT('',(-1.81978687191668,0.,-1.23627494547115));
#26107=CARTESIAN_POINT('Origin',(-1.73811241238545,0.,-1.34869019493419));
#26108=CARTESIAN_POINT('',(-1.73811241238545,1.,-1.34869019493419));
#26109=CARTESIAN_POINT('',(-1.81978687191668,1.,-1.23627494547115));
#26110=CARTESIAN_POINT('',(-1.73811241238545,0.,-1.34869019493419));
#26111=CARTESIAN_POINT('Ctrl Pts',(-1.31362392696032,-1.,-1.15624053661742));
#26112=CARTESIAN_POINT('Ctrl Pts',(-1.31362392696032,1.,-1.15624053661742));
#26113=CARTESIAN_POINT('Ctrl Pts',(-1.31722977216397,-1.,-1.15950888730809));
#26114=CARTESIAN_POINT('Ctrl Pts',(-1.31722977216397,1.,-1.15950888730809));
#26115=CARTESIAN_POINT('Ctrl Pts',(-1.32428080721772,-1.,-1.16589330093588));
#26116=CARTESIAN_POINT('Ctrl Pts',(-1.32428080721772,1.,-1.16589330093588));
#26117=CARTESIAN_POINT('Ctrl Pts',(-1.33437539347008,-1.,-1.17501305789857));
#26118=CARTESIAN_POINT('Ctrl Pts',(-1.33437539347008,1.,-1.17501305789857));
#26119=CARTESIAN_POINT('Ctrl Pts',(-1.34687054001093,-1.,-1.18625865667441));
#26120=CARTESIAN_POINT('Ctrl Pts',(-1.34687054001093,1.,-1.18625865667441));
#26121=CARTESIAN_POINT('Ctrl Pts',(-1.36088705043885,-1.,-1.1987959077932));
#26122=CARTESIAN_POINT('Ctrl Pts',(-1.36088705043885,1.,-1.1987959077932));
#26123=CARTESIAN_POINT('Ctrl Pts',(-1.37331915607905,-1.,-1.20982812925645));
#26124=CARTESIAN_POINT('Ctrl Pts',(-1.37331915607905,1.,-1.20982812925645));
#26125=CARTESIAN_POINT('Ctrl Pts',(-1.38420564527715,-1.,-1.21938737280852));
#26126=CARTESIAN_POINT('Ctrl Pts',(-1.38420564527715,1.,-1.21938737280852));
#26127=CARTESIAN_POINT('Ctrl Pts',(-1.39361389568796,-1.,-1.22752961899387));
#26128=CARTESIAN_POINT('Ctrl Pts',(-1.39361389568796,1.,-1.22752961899387));
#26129=CARTESIAN_POINT('Ctrl Pts',(-1.40164708206106,-1.,-1.23434087290423));
#26130=CARTESIAN_POINT('Ctrl Pts',(-1.40164708206106,1.,-1.23434087290423));
#26131=CARTESIAN_POINT('Ctrl Pts',(-1.40845295531283,-1.,-1.23994455029534));
#26132=CARTESIAN_POINT('Ctrl Pts',(-1.40845295531283,1.,-1.23994455029534));
#26133=CARTESIAN_POINT('Ctrl Pts',(-1.41422913175179,-1.,-1.24450600513056));
#26134=CARTESIAN_POINT('Ctrl Pts',(-1.41422913175179,1.,-1.24450600513056));
#26135=CARTESIAN_POINT('Ctrl Pts',(-1.41923722596025,-1.,-1.24824430986571));
#26136=CARTESIAN_POINT('Ctrl Pts',(-1.41923722596025,1.,-1.24824430986571));
#26137=CARTESIAN_POINT('Ctrl Pts',(-1.42378102115575,-1.,-1.2514145557001));
#26138=CARTESIAN_POINT('Ctrl Pts',(-1.42378102115575,1.,-1.2514145557001));
#26139=CARTESIAN_POINT('Ctrl Pts',(-1.42815938799387,-1.,-1.25426945222639));
#26140=CARTESIAN_POINT('Ctrl Pts',(-1.42815938799387,1.,-1.25426945222639));
#26141=CARTESIAN_POINT('Ctrl Pts',(-1.43262645609691,-1.,-1.25702687965755));
#26142=CARTESIAN_POINT('Ctrl Pts',(-1.43262645609691,1.,-1.25702687965755));
#26143=CARTESIAN_POINT('Ctrl Pts',(-1.43734919180848,-1.,-1.25983531012005));
#26144=CARTESIAN_POINT('Ctrl Pts',(-1.43734919180848,1.,-1.25983531012005));
#26145=CARTESIAN_POINT('Ctrl Pts',(-1.44236470511303,-1.,-1.26273903323859));
#26146=CARTESIAN_POINT('Ctrl Pts',(-1.44236470511303,1.,-1.26273903323859));
#26147=CARTESIAN_POINT('Ctrl Pts',(-1.44761985001662,-1.,-1.26570925118868));
#26148=CARTESIAN_POINT('Ctrl Pts',(-1.44761985001662,1.,-1.26570925118868));
#26149=CARTESIAN_POINT('Ctrl Pts',(-1.45301422764247,-1.,-1.2686778680489));
#26150=CARTESIAN_POINT('Ctrl Pts',(-1.45301422764247,1.,-1.2686778680489));
#26151=CARTESIAN_POINT('Ctrl Pts',(-1.45843906294697,-1.,-1.27156805265289));
#26152=CARTESIAN_POINT('Ctrl Pts',(-1.45843906294697,1.,-1.27156805265289));
#26153=CARTESIAN_POINT('Ctrl Pts',(-1.46382431332476,-1.,-1.27433119897822));
#26154=CARTESIAN_POINT('Ctrl Pts',(-1.46382431332476,1.,-1.27433119897822));
#26155=CARTESIAN_POINT('Ctrl Pts',(-1.46916035917133,-1.,-1.27696414831089));
#26156=CARTESIAN_POINT('Ctrl Pts',(-1.46916035917133,1.,-1.27696414831089));
#26157=CARTESIAN_POINT('Ctrl Pts',(-1.4744717526707,-1.,-1.2794891824849));
#26158=CARTESIAN_POINT('Ctrl Pts',(-1.4744717526707,1.,-1.2794891824849));
#26159=CARTESIAN_POINT('Ctrl Pts',(-1.47980070347095,-1.,-1.28194158939517));
#26160=CARTESIAN_POINT('Ctrl Pts',(-1.47980070347095,1.,-1.28194158939517));
#26161=CARTESIAN_POINT('Ctrl Pts',(-1.4851881711891,-1.,-1.28435533880201));
#26162=CARTESIAN_POINT('Ctrl Pts',(-1.4851881711891,1.,-1.28435533880201));
#26163=CARTESIAN_POINT('Ctrl Pts',(-1.4906522831278,-1.,-1.2867467611644));
#26164=CARTESIAN_POINT('Ctrl Pts',(-1.4906522831278,1.,-1.2867467611644));
#26165=CARTESIAN_POINT('Ctrl Pts',(-1.49618896881754,-1.,-1.28911506584254));
#26166=CARTESIAN_POINT('Ctrl Pts',(-1.49618896881754,1.,-1.28911506584254));
#26167=CARTESIAN_POINT('Ctrl Pts',(-1.50178230149776,-1.,-1.29145022885181));
#26168=CARTESIAN_POINT('Ctrl Pts',(-1.50178230149776,1.,-1.29145022885181));
#26169=CARTESIAN_POINT('Ctrl Pts',(-1.50741159078365,-1.,-1.29373841372842));
#26170=CARTESIAN_POINT('Ctrl Pts',(-1.50741159078365,1.,-1.29373841372842));
#26171=CARTESIAN_POINT('Ctrl Pts',(-1.51305994241402,-1.,-1.29596850710509));
#26172=CARTESIAN_POINT('Ctrl Pts',(-1.51305994241402,1.,-1.29596850710509));
#26173=CARTESIAN_POINT('Ctrl Pts',(-1.51872184912724,-1.,-1.29813791800747));
#26174=CARTESIAN_POINT('Ctrl Pts',(-1.51872184912724,1.,-1.29813791800747));
#26175=CARTESIAN_POINT('Ctrl Pts',(-1.52439957861062,-1.,-1.30024984366328));
#26176=CARTESIAN_POINT('Ctrl Pts',(-1.52439957861062,1.,-1.30024984366328));
#26177=CARTESIAN_POINT('Ctrl Pts',(-1.53009970283891,-1.,-1.30231064395568));
#26178=CARTESIAN_POINT('Ctrl Pts',(-1.53009970283891,1.,-1.30231064395568));
#26179=CARTESIAN_POINT('Ctrl Pts',(-1.53582981268977,-1.,-1.30432735639489));
#26180=CARTESIAN_POINT('Ctrl Pts',(-1.53582981268977,1.,-1.30432735639489));
#26181=CARTESIAN_POINT('Ctrl Pts',(-1.54159462645432,-1.,-1.30630475189556));
#26182=CARTESIAN_POINT('Ctrl Pts',(-1.54159462645432,1.,-1.30630475189556));
#26183=CARTESIAN_POINT('Ctrl Pts',(-1.54739413957185,-1.,-1.30824393907473));
#26184=CARTESIAN_POINT('Ctrl Pts',(-1.54739413957185,1.,-1.30824393907473));
#26185=CARTESIAN_POINT('Ctrl Pts',(-1.55322568759481,-1.,-1.31014393684222));
#26186=CARTESIAN_POINT('Ctrl Pts',(-1.55322568759481,1.,-1.31014393684222));
#26187=CARTESIAN_POINT('Ctrl Pts',(-1.55908521254821,-1.,-1.31200264341696));
#26188=CARTESIAN_POINT('Ctrl Pts',(-1.55908521254821,1.,-1.31200264341696));
#26189=CARTESIAN_POINT('Ctrl Pts',(-1.56496872402353,-1.,-1.31381795281002));
#26190=CARTESIAN_POINT('Ctrl Pts',(-1.56496872402353,1.,-1.31381795281002));
#26191=CARTESIAN_POINT('Ctrl Pts',(-1.57087397835723,-1.,-1.31558903860016));
#26192=CARTESIAN_POINT('Ctrl Pts',(-1.57087397835723,1.,-1.31558903860016));
#26193=CARTESIAN_POINT('Ctrl Pts',(-1.5768005650559,-1.,-1.31731642317187));
#26194=CARTESIAN_POINT('Ctrl Pts',(-1.5768005650559,1.,-1.31731642317187));
#26195=CARTESIAN_POINT('Ctrl Pts',(-1.58274907898834,-1.,-1.31900135021432));
#26196=CARTESIAN_POINT('Ctrl Pts',(-1.58274907898834,1.,-1.31900135021432));
#26197=CARTESIAN_POINT('Ctrl Pts',(-1.58872057258245,-1.,-1.32064537110892));
#26198=CARTESIAN_POINT('Ctrl Pts',(-1.58872057258245,1.,-1.32064537110892));
#26199=CARTESIAN_POINT('Ctrl Pts',(-1.59471591079403,-1.,-1.32224985747682));
#26200=CARTESIAN_POINT('Ctrl Pts',(-1.59471591079403,1.,-1.32224985747682));
#26201=CARTESIAN_POINT('Ctrl Pts',(-1.60073511858687,-1.,-1.32381550858256));
#26202=CARTESIAN_POINT('Ctrl Pts',(-1.60073511858687,1.,-1.32381550858256));
#26203=CARTESIAN_POINT('Ctrl Pts',(-1.60677758290954,-1.,-1.32534250785782));
#26204=CARTESIAN_POINT('Ctrl Pts',(-1.60677758290954,1.,-1.32534250785782));
#26205=CARTESIAN_POINT('Ctrl Pts',(-1.6128423401575,-1.,-1.32683074483356));
#26206=CARTESIAN_POINT('Ctrl Pts',(-1.6128423401575,1.,-1.32683074483356));
#26207=CARTESIAN_POINT('Ctrl Pts',(-1.61892832270724,-1.,-1.32828000610449));
#26208=CARTESIAN_POINT('Ctrl Pts',(-1.61892832270724,1.,-1.32828000610449));
#26209=CARTESIAN_POINT('Ctrl Pts',(-1.62503464209797,-1.,-1.3296901950568));
#26210=CARTESIAN_POINT('Ctrl Pts',(-1.62503464209797,1.,-1.3296901950568));
#26211=CARTESIAN_POINT('Ctrl Pts',(-1.63116079730923,-1.,-1.33106149345645));
#26212=CARTESIAN_POINT('Ctrl Pts',(-1.63116079730923,1.,-1.33106149345645));
#26213=CARTESIAN_POINT('Ctrl Pts',(-1.63730653475089,-1.,-1.33239425103724));
#26214=CARTESIAN_POINT('Ctrl Pts',(-1.63730653475089,1.,-1.33239425103724));
#26215=CARTESIAN_POINT('Ctrl Pts',(-1.6434717485603,-1.,-1.33368890676572));
#26216=CARTESIAN_POINT('Ctrl Pts',(-1.6434717485603,1.,-1.33368890676572));
#26217=CARTESIAN_POINT('Ctrl Pts',(-1.6496563728683,-1.,-1.33494590467993));
#26218=CARTESIAN_POINT('Ctrl Pts',(-1.6496563728683,1.,-1.33494590467993));
#26219=CARTESIAN_POINT('Ctrl Pts',(-1.65586025952593,-1.,-1.33616559745172));
#26220=CARTESIAN_POINT('Ctrl Pts',(-1.65586025952593,1.,-1.33616559745172));
#26221=CARTESIAN_POINT('Ctrl Pts',(-1.66208312541983,-1.,-1.33734820885262));
#26222=CARTESIAN_POINT('Ctrl Pts',(-1.66208312541983,1.,-1.33734820885262));
#26223=CARTESIAN_POINT('Ctrl Pts',(-1.66832460783989,-1.,-1.33849388654388));
#26224=CARTESIAN_POINT('Ctrl Pts',(-1.66832460783989,1.,-1.33849388654388));
#26225=CARTESIAN_POINT('Ctrl Pts',(-1.67458429426086,-1.,-1.3396027347034));
#26226=CARTESIAN_POINT('Ctrl Pts',(-1.67458429426086,1.,-1.3396027347034));
#26227=CARTESIAN_POINT('Ctrl Pts',(-1.68086176030362,-1.,-1.34067485185203));
#26228=CARTESIAN_POINT('Ctrl Pts',(-1.68086176030362,1.,-1.34067485185203));
#26229=CARTESIAN_POINT('Ctrl Pts',(-1.68715660868764,-1.,-1.341710374848));
#26230=CARTESIAN_POINT('Ctrl Pts',(-1.68715660868764,1.,-1.341710374848));
#26231=CARTESIAN_POINT('Ctrl Pts',(-1.6934684849687,-1.,-1.34270948206319));
#26232=CARTESIAN_POINT('Ctrl Pts',(-1.6934684849687,1.,-1.34270948206319));
#26233=CARTESIAN_POINT('Ctrl Pts',(-1.69979707754427,-1.,-1.34367237124483));
#26234=CARTESIAN_POINT('Ctrl Pts',(-1.69979707754427,1.,-1.34367237124483));
#26235=CARTESIAN_POINT('Ctrl Pts',(-1.70614212266738,-1.,-1.34459924533831));
#26236=CARTESIAN_POINT('Ctrl Pts',(-1.70614212266738,1.,-1.34459924533831));
#26237=CARTESIAN_POINT('Ctrl Pts',(-1.71250340686822,-1.,-1.34549029589416));
#26238=CARTESIAN_POINT('Ctrl Pts',(-1.71250340686822,1.,-1.34549029589416));
#26239=CARTESIAN_POINT('Ctrl Pts',(-1.7188807715049,-1.,-1.34634568653227));
#26240=CARTESIAN_POINT('Ctrl Pts',(-1.7188807715049,1.,-1.34634568653227));
#26241=CARTESIAN_POINT('Ctrl Pts',(-1.72527410680674,-1.,-1.34716554819527));
#26242=CARTESIAN_POINT('Ctrl Pts',(-1.72527410680674,1.,-1.34716554819527));
#26243=CARTESIAN_POINT('Ctrl Pts',(-1.7304014965394,-1.,-1.34779309152035));
#26244=CARTESIAN_POINT('Ctrl Pts',(-1.7304014965394,1.,-1.34779309152035));
#26245=CARTESIAN_POINT('Ctrl Pts',(-1.73425417885907,-1.,-1.34824783112887));
#26246=CARTESIAN_POINT('Ctrl Pts',(-1.73425417885907,1.,-1.34824783112887));
#26247=CARTESIAN_POINT('Ctrl Pts',(-1.73682580585691,-1.,-1.34854391898045));
#26248=CARTESIAN_POINT('Ctrl Pts',(-1.73682580585691,1.,-1.34854391898045));
#26249=CARTESIAN_POINT('Ctrl Pts',(-1.73811241238545,-1.,-1.34869019493419));
#26250=CARTESIAN_POINT('Ctrl Pts',(-1.73811241238545,1.,-1.34869019493419));
#26251=CARTESIAN_POINT('',(-1.31362392696032,1.,-1.15624053661742));
#26252=CARTESIAN_POINT('Ctrl Pts',(-1.31362392696032,1.,-1.15624053661742));
#26253=CARTESIAN_POINT('Ctrl Pts',(-1.31722977216397,1.,-1.15950888730809));
#26254=CARTESIAN_POINT('Ctrl Pts',(-1.32428080721772,1.,-1.16589330093588));
#26255=CARTESIAN_POINT('Ctrl Pts',(-1.33437539347008,1.,-1.17501305789857));
#26256=CARTESIAN_POINT('Ctrl Pts',(-1.34687054001093,1.,-1.18625865667441));
#26257=CARTESIAN_POINT('Ctrl Pts',(-1.36088705043885,1.,-1.1987959077932));
#26258=CARTESIAN_POINT('Ctrl Pts',(-1.37331915607905,1.,-1.20982812925645));
#26259=CARTESIAN_POINT('Ctrl Pts',(-1.38420564527715,1.,-1.21938737280852));
#26260=CARTESIAN_POINT('Ctrl Pts',(-1.39361389568796,1.,-1.22752961899387));
#26261=CARTESIAN_POINT('Ctrl Pts',(-1.40164708206106,1.,-1.23434087290423));
#26262=CARTESIAN_POINT('Ctrl Pts',(-1.40845295531283,1.,-1.23994455029534));
#26263=CARTESIAN_POINT('Ctrl Pts',(-1.41422913175179,1.,-1.24450600513056));
#26264=CARTESIAN_POINT('Ctrl Pts',(-1.41923722596025,1.,-1.24824430986571));
#26265=CARTESIAN_POINT('Ctrl Pts',(-1.42378102115575,1.,-1.2514145557001));
#26266=CARTESIAN_POINT('Ctrl Pts',(-1.42815938799387,1.,-1.25426945222639));
#26267=CARTESIAN_POINT('Ctrl Pts',(-1.43262645609691,1.,-1.25702687965755));
#26268=CARTESIAN_POINT('Ctrl Pts',(-1.43734919180848,1.,-1.25983531012005));
#26269=CARTESIAN_POINT('Ctrl Pts',(-1.44236470511303,1.,-1.26273903323859));
#26270=CARTESIAN_POINT('Ctrl Pts',(-1.44761985001662,1.,-1.26570925118868));
#26271=CARTESIAN_POINT('Ctrl Pts',(-1.45301422764247,1.,-1.2686778680489));
#26272=CARTESIAN_POINT('Ctrl Pts',(-1.45843906294697,1.,-1.27156805265289));
#26273=CARTESIAN_POINT('Ctrl Pts',(-1.46382431332476,1.,-1.27433119897822));
#26274=CARTESIAN_POINT('Ctrl Pts',(-1.46916035917133,1.,-1.27696414831089));
#26275=CARTESIAN_POINT('Ctrl Pts',(-1.4744717526707,1.,-1.2794891824849));
#26276=CARTESIAN_POINT('Ctrl Pts',(-1.47980070347095,1.,-1.28194158939517));
#26277=CARTESIAN_POINT('Ctrl Pts',(-1.4851881711891,1.,-1.28435533880201));
#26278=CARTESIAN_POINT('Ctrl Pts',(-1.4906522831278,1.,-1.2867467611644));
#26279=CARTESIAN_POINT('Ctrl Pts',(-1.49618896881754,1.,-1.28911506584254));
#26280=CARTESIAN_POINT('Ctrl Pts',(-1.50178230149776,1.,-1.29145022885181));
#26281=CARTESIAN_POINT('Ctrl Pts',(-1.50741159078365,1.,-1.29373841372842));
#26282=CARTESIAN_POINT('Ctrl Pts',(-1.51305994241402,1.,-1.29596850710509));
#26283=CARTESIAN_POINT('Ctrl Pts',(-1.51872184912724,1.,-1.29813791800747));
#26284=CARTESIAN_POINT('Ctrl Pts',(-1.52439957861062,1.,-1.30024984366328));
#26285=CARTESIAN_POINT('Ctrl Pts',(-1.53009970283891,1.,-1.30231064395568));
#26286=CARTESIAN_POINT('Ctrl Pts',(-1.53582981268977,1.,-1.30432735639489));
#26287=CARTESIAN_POINT('Ctrl Pts',(-1.54159462645432,1.,-1.30630475189556));
#26288=CARTESIAN_POINT('Ctrl Pts',(-1.54739413957185,1.,-1.30824393907473));
#26289=CARTESIAN_POINT('Ctrl Pts',(-1.55322568759481,1.,-1.31014393684222));
#26290=CARTESIAN_POINT('Ctrl Pts',(-1.55908521254821,1.,-1.31200264341696));
#26291=CARTESIAN_POINT('Ctrl Pts',(-1.56496872402353,1.,-1.31381795281002));
#26292=CARTESIAN_POINT('Ctrl Pts',(-1.57087397835723,1.,-1.31558903860016));
#26293=CARTESIAN_POINT('Ctrl Pts',(-1.5768005650559,1.,-1.31731642317187));
#26294=CARTESIAN_POINT('Ctrl Pts',(-1.58274907898834,1.,-1.31900135021432));
#26295=CARTESIAN_POINT('Ctrl Pts',(-1.58872057258245,1.,-1.32064537110892));
#26296=CARTESIAN_POINT('Ctrl Pts',(-1.59471591079403,1.,-1.32224985747682));
#26297=CARTESIAN_POINT('Ctrl Pts',(-1.60073511858687,1.,-1.32381550858256));
#26298=CARTESIAN_POINT('Ctrl Pts',(-1.60677758290954,1.,-1.32534250785782));
#26299=CARTESIAN_POINT('Ctrl Pts',(-1.6128423401575,1.,-1.32683074483356));
#26300=CARTESIAN_POINT('Ctrl Pts',(-1.61892832270724,1.,-1.32828000610449));
#26301=CARTESIAN_POINT('Ctrl Pts',(-1.62503464209797,1.,-1.3296901950568));
#26302=CARTESIAN_POINT('Ctrl Pts',(-1.63116079730923,1.,-1.33106149345645));
#26303=CARTESIAN_POINT('Ctrl Pts',(-1.63730653475089,1.,-1.33239425103724));
#26304=CARTESIAN_POINT('Ctrl Pts',(-1.6434717485603,1.,-1.33368890676572));
#26305=CARTESIAN_POINT('Ctrl Pts',(-1.6496563728683,1.,-1.33494590467993));
#26306=CARTESIAN_POINT('Ctrl Pts',(-1.65586025952593,1.,-1.33616559745172));
#26307=CARTESIAN_POINT('Ctrl Pts',(-1.66208312541983,1.,-1.33734820885262));
#26308=CARTESIAN_POINT('Ctrl Pts',(-1.66832460783989,1.,-1.33849388654388));
#26309=CARTESIAN_POINT('Ctrl Pts',(-1.67458429426086,1.,-1.3396027347034));
#26310=CARTESIAN_POINT('Ctrl Pts',(-1.68086176030362,1.,-1.34067485185203));
#26311=CARTESIAN_POINT('Ctrl Pts',(-1.68715660868764,1.,-1.341710374848));
#26312=CARTESIAN_POINT('Ctrl Pts',(-1.6934684849687,1.,-1.34270948206319));
#26313=CARTESIAN_POINT('Ctrl Pts',(-1.69979707754427,1.,-1.34367237124483));
#26314=CARTESIAN_POINT('Ctrl Pts',(-1.70614212266738,1.,-1.34459924533831));
#26315=CARTESIAN_POINT('Ctrl Pts',(-1.71250340686822,1.,-1.34549029589416));
#26316=CARTESIAN_POINT('Ctrl Pts',(-1.7188807715049,1.,-1.34634568653227));
#26317=CARTESIAN_POINT('Ctrl Pts',(-1.72527410680674,1.,-1.34716554819527));
#26318=CARTESIAN_POINT('Ctrl Pts',(-1.7304014965394,1.,-1.34779309152035));
#26319=CARTESIAN_POINT('Ctrl Pts',(-1.73425417885907,1.,-1.34824783112887));
#26320=CARTESIAN_POINT('Ctrl Pts',(-1.73682580585691,1.,-1.34854391898045));
#26321=CARTESIAN_POINT('Ctrl Pts',(-1.73811241238545,1.,-1.34869019493419));
#26322=CARTESIAN_POINT('',(-1.31362392696032,0.,-1.15624053661742));
#26323=CARTESIAN_POINT('Origin',(0.,0.,0.));
#26324=CARTESIAN_POINT('',(-1.15624053661742,1.,-1.31362392696033));
#26325=CARTESIAN_POINT('Origin',(0.,1.,0.));
#26326=CARTESIAN_POINT('',(-1.15624053661742,0.,-1.31362392696033));
#26327=CARTESIAN_POINT('Ctrl Pts',(-1.34869019493419,-1.,-1.73811241238545));
#26328=CARTESIAN_POINT('Ctrl Pts',(-1.34869019493419,1.,-1.73811241238545));
#26329=CARTESIAN_POINT('Ctrl Pts',(-1.34854391898145,-1.,-1.73682580585819));
#26330=CARTESIAN_POINT('Ctrl Pts',(-1.34854391898145,1.,-1.73682580585819));
#26331=CARTESIAN_POINT('Ctrl Pts',(-1.34824783113158,-1.,-1.73425417886255));
#26332=CARTESIAN_POINT('Ctrl Pts',(-1.34824783113158,1.,-1.73425417886255));
#26333=CARTESIAN_POINT('Ctrl Pts',(-1.3477930915247,-1.,-1.73040149654497));
#26334=CARTESIAN_POINT('Ctrl Pts',(-1.3477930915247,1.,-1.73040149654497));
#26335=CARTESIAN_POINT('Ctrl Pts',(-1.34716554820013,-1.,-1.72527410681298));
#26336=CARTESIAN_POINT('Ctrl Pts',(-1.34716554820013,1.,-1.72527410681298));
#26337=CARTESIAN_POINT('Ctrl Pts',(-1.34634568653586,-1.,-1.7188807715095));
#26338=CARTESIAN_POINT('Ctrl Pts',(-1.34634568653586,1.,-1.7188807715095));
#26339=CARTESIAN_POINT('Ctrl Pts',(-1.34549029589563,-1.,-1.71250340687011));
#26340=CARTESIAN_POINT('Ctrl Pts',(-1.34549029589563,1.,-1.71250340687011));
#26341=CARTESIAN_POINT('Ctrl Pts',(-1.34459924533783,-1.,-1.70614212266676));
#26342=CARTESIAN_POINT('Ctrl Pts',(-1.34459924533783,1.,-1.70614212266676));
#26343=CARTESIAN_POINT('Ctrl Pts',(-1.34367237124322,-1.,-1.69979707754221));
#26344=CARTESIAN_POINT('Ctrl Pts',(-1.34367237124322,1.,-1.69979707754221));
#26345=CARTESIAN_POINT('Ctrl Pts',(-1.34270948206139,-1.,-1.6934684849664));
#26346=CARTESIAN_POINT('Ctrl Pts',(-1.34270948206139,1.,-1.6934684849664));
#26347=CARTESIAN_POINT('Ctrl Pts',(-1.34171037484673,-1.,-1.68715660868602));
#26348=CARTESIAN_POINT('Ctrl Pts',(-1.34171037484673,1.,-1.68715660868602));
#26349=CARTESIAN_POINT('Ctrl Pts',(-1.3406748518516,-1.,-1.68086176030308));
#26350=CARTESIAN_POINT('Ctrl Pts',(-1.3406748518516,1.,-1.68086176030308));
#26351=CARTESIAN_POINT('Ctrl Pts',(-1.33960273470372,-1.,-1.67458429426126));
#26352=CARTESIAN_POINT('Ctrl Pts',(-1.33960273470372,1.,-1.67458429426126));
#26353=CARTESIAN_POINT('Ctrl Pts',(-1.33849388654458,-1.,-1.66832460784078));
#26354=CARTESIAN_POINT('Ctrl Pts',(-1.33849388654458,1.,-1.66832460784078));
#26355=CARTESIAN_POINT('Ctrl Pts',(-1.33734820885331,-1.,-1.66208312542073));
#26356=CARTESIAN_POINT('Ctrl Pts',(-1.33734820885331,1.,-1.66208312542073));
#26357=CARTESIAN_POINT('Ctrl Pts',(-1.33616559745217,-1.,-1.65586025952651));
#26358=CARTESIAN_POINT('Ctrl Pts',(-1.33616559745217,1.,-1.65586025952651));
#26359=CARTESIAN_POINT('Ctrl Pts',(-1.33494590468003,-1.,-1.64965637286843));
#26360=CARTESIAN_POINT('Ctrl Pts',(-1.33494590468003,1.,-1.64965637286843));
#26361=CARTESIAN_POINT('Ctrl Pts',(-1.33368890676554,-1.,-1.64347174856007));
#26362=CARTESIAN_POINT('Ctrl Pts',(-1.33368890676554,1.,-1.64347174856007));
#26363=CARTESIAN_POINT('Ctrl Pts',(-1.33239425103694,-1.,-1.6373065347505));
#26364=CARTESIAN_POINT('Ctrl Pts',(-1.33239425103694,1.,-1.6373065347505));
#26365=CARTESIAN_POINT('Ctrl Pts',(-1.33106149345618,-1.,-1.63116079730887));
#26366=CARTESIAN_POINT('Ctrl Pts',(-1.33106149345618,1.,-1.63116079730887));
#26367=CARTESIAN_POINT('Ctrl Pts',(-1.32969019505665,-1.,-1.62503464209777));
#26368=CARTESIAN_POINT('Ctrl Pts',(-1.32969019505665,1.,-1.62503464209777));
#26369=CARTESIAN_POINT('Ctrl Pts',(-1.32828000610448,-1.,-1.61892832270723));
#26370=CARTESIAN_POINT('Ctrl Pts',(-1.32828000610448,1.,-1.61892832270723));
#26371=CARTESIAN_POINT('Ctrl Pts',(-1.32683074483365,-1.,-1.61284234015762));
#26372=CARTESIAN_POINT('Ctrl Pts',(-1.32683074483365,1.,-1.61284234015762));
#26373=CARTESIAN_POINT('Ctrl Pts',(-1.32534250785794,-1.,-1.6067775829097));
#26374=CARTESIAN_POINT('Ctrl Pts',(-1.32534250785794,1.,-1.6067775829097));
#26375=CARTESIAN_POINT('Ctrl Pts',(-1.32381550858266,-1.,-1.600735118587));
#26376=CARTESIAN_POINT('Ctrl Pts',(-1.32381550858266,1.,-1.600735118587));
#26377=CARTESIAN_POINT('Ctrl Pts',(-1.32224985747686,-1.,-1.59471591079408));
#26378=CARTESIAN_POINT('Ctrl Pts',(-1.32224985747686,1.,-1.59471591079408));
#26379=CARTESIAN_POINT('Ctrl Pts',(-1.32064537110891,-1.,-1.58872057258244));
#26380=CARTESIAN_POINT('Ctrl Pts',(-1.32064537110891,1.,-1.58872057258244));
#26381=CARTESIAN_POINT('Ctrl Pts',(-1.31900135021428,-1.,-1.58274907898829));
#26382=CARTESIAN_POINT('Ctrl Pts',(-1.31900135021428,1.,-1.58274907898829));
#26383=CARTESIAN_POINT('Ctrl Pts',(-1.31731642317183,-1.,-1.57680056505585));
#26384=CARTESIAN_POINT('Ctrl Pts',(-1.31731642317183,1.,-1.57680056505585));
#26385=CARTESIAN_POINT('Ctrl Pts',(-1.31558903860015,-1.,-1.57087397835721));
#26386=CARTESIAN_POINT('Ctrl Pts',(-1.31558903860015,1.,-1.57087397835721));
#26387=CARTESIAN_POINT('Ctrl Pts',(-1.31381795281002,-1.,-1.56496872402352));
#26388=CARTESIAN_POINT('Ctrl Pts',(-1.31381795281002,1.,-1.56496872402352));
#26389=CARTESIAN_POINT('Ctrl Pts',(-1.31200264341696,-1.,-1.55908521254822));
#26390=CARTESIAN_POINT('Ctrl Pts',(-1.31200264341696,1.,-1.55908521254822));
#26391=CARTESIAN_POINT('Ctrl Pts',(-1.31014393684221,-1.,-1.55322568759481));
#26392=CARTESIAN_POINT('Ctrl Pts',(-1.31014393684221,1.,-1.55322568759481));
#26393=CARTESIAN_POINT('Ctrl Pts',(-1.30824393907471,-1.,-1.54739413957183));
#26394=CARTESIAN_POINT('Ctrl Pts',(-1.30824393907471,1.,-1.54739413957183));
#26395=CARTESIAN_POINT('Ctrl Pts',(-1.30630475189553,-1.,-1.54159462645428));
#26396=CARTESIAN_POINT('Ctrl Pts',(-1.30630475189553,1.,-1.54159462645428));
#26397=CARTESIAN_POINT('Ctrl Pts',(-1.30432735639487,-1.,-1.53582981268976));
#26398=CARTESIAN_POINT('Ctrl Pts',(-1.30432735639487,1.,-1.53582981268976));
#26399=CARTESIAN_POINT('Ctrl Pts',(-1.3023106439557,-1.,-1.53009970283893));
#26400=CARTESIAN_POINT('Ctrl Pts',(-1.3023106439557,1.,-1.53009970283893));
#26401=CARTESIAN_POINT('Ctrl Pts',(-1.30024984366334,-1.,-1.5243995786107));
#26402=CARTESIAN_POINT('Ctrl Pts',(-1.30024984366334,1.,-1.5243995786107));
#26403=CARTESIAN_POINT('Ctrl Pts',(-1.29813791800757,-1.,-1.51872184912735));
#26404=CARTESIAN_POINT('Ctrl Pts',(-1.29813791800757,1.,-1.51872184912735));
#26405=CARTESIAN_POINT('Ctrl Pts',(-1.29596850710518,-1.,-1.51305994241412));
#26406=CARTESIAN_POINT('Ctrl Pts',(-1.29596850710518,1.,-1.51305994241412));
#26407=CARTESIAN_POINT('Ctrl Pts',(-1.29373841372843,-1.,-1.50741159078367));
#26408=CARTESIAN_POINT('Ctrl Pts',(-1.29373841372843,1.,-1.50741159078367));
#26409=CARTESIAN_POINT('Ctrl Pts',(-1.29145022885171,-1.,-1.50178230149764));
#26410=CARTESIAN_POINT('Ctrl Pts',(-1.29145022885171,1.,-1.50178230149764));
#26411=CARTESIAN_POINT('Ctrl Pts',(-1.28911506584232,-1.,-1.49618896881729));
#26412=CARTESIAN_POINT('Ctrl Pts',(-1.28911506584232,1.,-1.49618896881729));
#26413=CARTESIAN_POINT('Ctrl Pts',(-1.28674676116415,-1.,-1.4906522831275));
#26414=CARTESIAN_POINT('Ctrl Pts',(-1.28674676116415,1.,-1.4906522831275));
#26415=CARTESIAN_POINT('Ctrl Pts',(-1.28435533880184,-1.,-1.48518817118891));
#26416=CARTESIAN_POINT('Ctrl Pts',(-1.28435533880184,1.,-1.48518817118891));
#26417=CARTESIAN_POINT('Ctrl Pts',(-1.28194158939522,-1.,-1.47980070347102));
#26418=CARTESIAN_POINT('Ctrl Pts',(-1.28194158939522,1.,-1.47980070347102));
#26419=CARTESIAN_POINT('Ctrl Pts',(-1.27948918248524,-1.,-1.4744717526711));
#26420=CARTESIAN_POINT('Ctrl Pts',(-1.27948918248524,1.,-1.4744717526711));
#26421=CARTESIAN_POINT('Ctrl Pts',(-1.27696414831144,-1.,-1.46916035917197));
#26422=CARTESIAN_POINT('Ctrl Pts',(-1.27696414831144,1.,-1.46916035917197));
#26423=CARTESIAN_POINT('Ctrl Pts',(-1.27433119897877,-1.,-1.4638243133254));
#26424=CARTESIAN_POINT('Ctrl Pts',(-1.27433119897877,1.,-1.4638243133254));
#26425=CARTESIAN_POINT('Ctrl Pts',(-1.27156805265312,-1.,-1.45843906294725));
#26426=CARTESIAN_POINT('Ctrl Pts',(-1.27156805265312,1.,-1.45843906294725));
#26427=CARTESIAN_POINT('Ctrl Pts',(-1.26867786804854,-1.,-1.45301422764205));
#26428=CARTESIAN_POINT('Ctrl Pts',(-1.26867786804854,1.,-1.45301422764205));
#26429=CARTESIAN_POINT('Ctrl Pts',(-1.26570925118767,-1.,-1.44761985001544));
#26430=CARTESIAN_POINT('Ctrl Pts',(-1.26570925118767,1.,-1.44761985001544));
#26431=CARTESIAN_POINT('Ctrl Pts',(-1.26273903323723,-1.,-1.44236470511145));
#26432=CARTESIAN_POINT('Ctrl Pts',(-1.26273903323723,1.,-1.44236470511145));
#26433=CARTESIAN_POINT('Ctrl Pts',(-1.25983531011894,-1.,-1.43734919180719));
#26434=CARTESIAN_POINT('Ctrl Pts',(-1.25983531011894,1.,-1.43734919180719));
#26435=CARTESIAN_POINT('Ctrl Pts',(-1.25702687965744,-1.,-1.43262645609679));
#26436=CARTESIAN_POINT('Ctrl Pts',(-1.25702687965744,1.,-1.43262645609679));
#26437=CARTESIAN_POINT('Ctrl Pts',(-1.25426945222783,-1.,-1.42815938799555));
#26438=CARTESIAN_POINT('Ctrl Pts',(-1.25426945222783,1.,-1.42815938799555));
#26439=CARTESIAN_POINT('Ctrl Pts',(-1.25141455570299,-1.,-1.42378102115911));
#26440=CARTESIAN_POINT('Ctrl Pts',(-1.25141455570299,1.,-1.42378102115911));
#26441=CARTESIAN_POINT('Ctrl Pts',(-1.24824430986911,-1.,-1.41923722596421));
#26442=CARTESIAN_POINT('Ctrl Pts',(-1.24824430986911,1.,-1.41923722596421));
#26443=CARTESIAN_POINT('Ctrl Pts',(-1.24450600513278,-1.,-1.41422913175437));
#26444=CARTESIAN_POINT('Ctrl Pts',(-1.24450600513278,1.,-1.41422913175437));
#26445=CARTESIAN_POINT('Ctrl Pts',(-1.23994455029421,-1.,-1.40845295531151));
#26446=CARTESIAN_POINT('Ctrl Pts',(-1.23994455029421,1.,-1.40845295531151));
#26447=CARTESIAN_POINT('Ctrl Pts',(-1.23434087289768,-1.,-1.40164708205345));
#26448=CARTESIAN_POINT('Ctrl Pts',(-1.23434087289768,1.,-1.40164708205345));
#26449=CARTESIAN_POINT('Ctrl Pts',(-1.22752961898063,-1.,-1.39361389567257));
#26450=CARTESIAN_POINT('Ctrl Pts',(-1.22752961898063,1.,-1.39361389567257));
#26451=CARTESIAN_POINT('Ctrl Pts',(-1.21938737278853,-1.,-1.38420564525391));
#26452=CARTESIAN_POINT('Ctrl Pts',(-1.21938737278853,1.,-1.38420564525391));
#26453=CARTESIAN_POINT('Ctrl Pts',(-1.20982812923113,-1.,-1.37331915604962));
#26454=CARTESIAN_POINT('Ctrl Pts',(-1.20982812923113,1.,-1.37331915604962));
#26455=CARTESIAN_POINT('Ctrl Pts',(-1.1987959077656,-1.,-1.36088705040677));
#26456=CARTESIAN_POINT('Ctrl Pts',(-1.1987959077656,1.,-1.36088705040677));
#26457=CARTESIAN_POINT('Ctrl Pts',(-1.18625865664915,-1.,-1.34687053998157));
#26458=CARTESIAN_POINT('Ctrl Pts',(-1.18625865664915,1.,-1.34687053998157));
#26459=CARTESIAN_POINT('Ctrl Pts',(-1.17501305787994,-1.,-1.33437539344842));
#26460=CARTESIAN_POINT('Ctrl Pts',(-1.17501305787994,1.,-1.33437539344842));
#26461=CARTESIAN_POINT('Ctrl Pts',(-1.16589330092532,-1.,-1.32428080720544));
#26462=CARTESIAN_POINT('Ctrl Pts',(-1.16589330092532,1.,-1.32428080720544));
#26463=CARTESIAN_POINT('Ctrl Pts',(-1.15950888730433,-1.,-1.3172297721596));
#26464=CARTESIAN_POINT('Ctrl Pts',(-1.15950888730433,1.,-1.3172297721596));
#26465=CARTESIAN_POINT('Ctrl Pts',(-1.15624053661742,-1.,-1.31362392696033));
#26466=CARTESIAN_POINT('Ctrl Pts',(-1.15624053661742,1.,-1.31362392696033));
#26467=CARTESIAN_POINT('',(-1.34869019493419,1.,-1.73811241238545));
#26468=CARTESIAN_POINT('Ctrl Pts',(-1.34869019493419,1.,-1.73811241238545));
#26469=CARTESIAN_POINT('Ctrl Pts',(-1.34854391898145,1.,-1.73682580585819));
#26470=CARTESIAN_POINT('Ctrl Pts',(-1.34824783113158,1.,-1.73425417886255));
#26471=CARTESIAN_POINT('Ctrl Pts',(-1.3477930915247,1.,-1.73040149654497));
#26472=CARTESIAN_POINT('Ctrl Pts',(-1.34716554820013,1.,-1.72527410681298));
#26473=CARTESIAN_POINT('Ctrl Pts',(-1.34634568653586,1.,-1.7188807715095));
#26474=CARTESIAN_POINT('Ctrl Pts',(-1.34549029589563,1.,-1.71250340687011));
#26475=CARTESIAN_POINT('Ctrl Pts',(-1.34459924533783,1.,-1.70614212266676));
#26476=CARTESIAN_POINT('Ctrl Pts',(-1.34367237124322,1.,-1.69979707754221));
#26477=CARTESIAN_POINT('Ctrl Pts',(-1.34270948206139,1.,-1.6934684849664));
#26478=CARTESIAN_POINT('Ctrl Pts',(-1.34171037484673,1.,-1.68715660868602));
#26479=CARTESIAN_POINT('Ctrl Pts',(-1.3406748518516,1.,-1.68086176030308));
#26480=CARTESIAN_POINT('Ctrl Pts',(-1.33960273470372,1.,-1.67458429426126));
#26481=CARTESIAN_POINT('Ctrl Pts',(-1.33849388654458,1.,-1.66832460784078));
#26482=CARTESIAN_POINT('Ctrl Pts',(-1.33734820885331,1.,-1.66208312542073));
#26483=CARTESIAN_POINT('Ctrl Pts',(-1.33616559745217,1.,-1.65586025952651));
#26484=CARTESIAN_POINT('Ctrl Pts',(-1.33494590468003,1.,-1.64965637286843));
#26485=CARTESIAN_POINT('Ctrl Pts',(-1.33368890676554,1.,-1.64347174856007));
#26486=CARTESIAN_POINT('Ctrl Pts',(-1.33239425103694,1.,-1.6373065347505));
#26487=CARTESIAN_POINT('Ctrl Pts',(-1.33106149345618,1.,-1.63116079730887));
#26488=CARTESIAN_POINT('Ctrl Pts',(-1.32969019505665,1.,-1.62503464209777));
#26489=CARTESIAN_POINT('Ctrl Pts',(-1.32828000610448,1.,-1.61892832270723));
#26490=CARTESIAN_POINT('Ctrl Pts',(-1.32683074483365,1.,-1.61284234015762));
#26491=CARTESIAN_POINT('Ctrl Pts',(-1.32534250785794,1.,-1.6067775829097));
#26492=CARTESIAN_POINT('Ctrl Pts',(-1.32381550858266,1.,-1.600735118587));
#26493=CARTESIAN_POINT('Ctrl Pts',(-1.32224985747686,1.,-1.59471591079408));
#26494=CARTESIAN_POINT('Ctrl Pts',(-1.32064537110891,1.,-1.58872057258244));
#26495=CARTESIAN_POINT('Ctrl Pts',(-1.31900135021428,1.,-1.58274907898829));
#26496=CARTESIAN_POINT('Ctrl Pts',(-1.31731642317183,1.,-1.57680056505585));
#26497=CARTESIAN_POINT('Ctrl Pts',(-1.31558903860015,1.,-1.57087397835721));
#26498=CARTESIAN_POINT('Ctrl Pts',(-1.31381795281002,1.,-1.56496872402352));
#26499=CARTESIAN_POINT('Ctrl Pts',(-1.31200264341696,1.,-1.55908521254822));
#26500=CARTESIAN_POINT('Ctrl Pts',(-1.31014393684221,1.,-1.55322568759481));
#26501=CARTESIAN_POINT('Ctrl Pts',(-1.30824393907471,1.,-1.54739413957183));
#26502=CARTESIAN_POINT('Ctrl Pts',(-1.30630475189553,1.,-1.54159462645428));
#26503=CARTESIAN_POINT('Ctrl Pts',(-1.30432735639487,1.,-1.53582981268976));
#26504=CARTESIAN_POINT('Ctrl Pts',(-1.3023106439557,1.,-1.53009970283893));
#26505=CARTESIAN_POINT('Ctrl Pts',(-1.30024984366334,1.,-1.5243995786107));
#26506=CARTESIAN_POINT('Ctrl Pts',(-1.29813791800757,1.,-1.51872184912735));
#26507=CARTESIAN_POINT('Ctrl Pts',(-1.29596850710518,1.,-1.51305994241412));
#26508=CARTESIAN_POINT('Ctrl Pts',(-1.29373841372843,1.,-1.50741159078367));
#26509=CARTESIAN_POINT('Ctrl Pts',(-1.29145022885171,1.,-1.50178230149764));
#26510=CARTESIAN_POINT('Ctrl Pts',(-1.28911506584232,1.,-1.49618896881729));
#26511=CARTESIAN_POINT('Ctrl Pts',(-1.28674676116415,1.,-1.4906522831275));
#26512=CARTESIAN_POINT('Ctrl Pts',(-1.28435533880184,1.,-1.48518817118891));
#26513=CARTESIAN_POINT('Ctrl Pts',(-1.28194158939522,1.,-1.47980070347102));
#26514=CARTESIAN_POINT('Ctrl Pts',(-1.27948918248524,1.,-1.4744717526711));
#26515=CARTESIAN_POINT('Ctrl Pts',(-1.27696414831144,1.,-1.46916035917197));
#26516=CARTESIAN_POINT('Ctrl Pts',(-1.27433119897877,1.,-1.4638243133254));
#26517=CARTESIAN_POINT('Ctrl Pts',(-1.27156805265312,1.,-1.45843906294725));
#26518=CARTESIAN_POINT('Ctrl Pts',(-1.26867786804854,1.,-1.45301422764205));
#26519=CARTESIAN_POINT('Ctrl Pts',(-1.26570925118767,1.,-1.44761985001544));
#26520=CARTESIAN_POINT('Ctrl Pts',(-1.26273903323723,1.,-1.44236470511145));
#26521=CARTESIAN_POINT('Ctrl Pts',(-1.25983531011894,1.,-1.43734919180719));
#26522=CARTESIAN_POINT('Ctrl Pts',(-1.25702687965744,1.,-1.43262645609679));
#26523=CARTESIAN_POINT('Ctrl Pts',(-1.25426945222783,1.,-1.42815938799555));
#26524=CARTESIAN_POINT('Ctrl Pts',(-1.25141455570299,1.,-1.42378102115911));
#26525=CARTESIAN_POINT('Ctrl Pts',(-1.24824430986911,1.,-1.41923722596421));
#26526=CARTESIAN_POINT('Ctrl Pts',(-1.24450600513278,1.,-1.41422913175437));
#26527=CARTESIAN_POINT('Ctrl Pts',(-1.23994455029421,1.,-1.40845295531151));
#26528=CARTESIAN_POINT('Ctrl Pts',(-1.23434087289768,1.,-1.40164708205345));
#26529=CARTESIAN_POINT('Ctrl Pts',(-1.22752961898063,1.,-1.39361389567257));
#26530=CARTESIAN_POINT('Ctrl Pts',(-1.21938737278853,1.,-1.38420564525391));
#26531=CARTESIAN_POINT('Ctrl Pts',(-1.20982812923113,1.,-1.37331915604962));
#26532=CARTESIAN_POINT('Ctrl Pts',(-1.1987959077656,1.,-1.36088705040677));
#26533=CARTESIAN_POINT('Ctrl Pts',(-1.18625865664915,1.,-1.34687053998157));
#26534=CARTESIAN_POINT('Ctrl Pts',(-1.17501305787994,1.,-1.33437539344842));
#26535=CARTESIAN_POINT('Ctrl Pts',(-1.16589330092532,1.,-1.32428080720544));
#26536=CARTESIAN_POINT('Ctrl Pts',(-1.15950888730433,1.,-1.3172297721596));
#26537=CARTESIAN_POINT('Ctrl Pts',(-1.15624053661742,1.,-1.31362392696033));
#26538=CARTESIAN_POINT('',(-1.34869019493419,0.,-1.73811241238545));
#26539=CARTESIAN_POINT('Origin',(-1.23627494547115,0.,-1.81978687191668));
#26540=CARTESIAN_POINT('',(-1.23627494547115,1.,-1.81978687191668));
#26541=CARTESIAN_POINT('',(-1.34869019493419,1.,-1.73811241238545));
#26542=CARTESIAN_POINT('',(-1.23627494547115,0.,-1.81978687191668));
#26543=CARTESIAN_POINT('Ctrl Pts',(-0.892032620296855,-1.,-1.5055822144029));
#26544=CARTESIAN_POINT('Ctrl Pts',(-0.892032620296855,1.,-1.5055822144029));
#26545=CARTESIAN_POINT('Ctrl Pts',(-0.894452006967538,-1.,-1.50980486807181));
#26546=CARTESIAN_POINT('Ctrl Pts',(-0.894452006967538,1.,-1.50980486807181));
#26547=CARTESIAN_POINT('Ctrl Pts',(-0.89918504749193,-1.,-1.51805569591479));
#26548=CARTESIAN_POINT('Ctrl Pts',(-0.89918504749193,1.,-1.51805569591479));
#26549=CARTESIAN_POINT('Ctrl Pts',(-0.905967409640499,-1.,-1.52984849890434));
#26550=CARTESIAN_POINT('Ctrl Pts',(-0.905967409640499,1.,-1.52984849890434));
#26551=CARTESIAN_POINT('Ctrl Pts',(-0.91437591904658,-1.,-1.54440491152808));
#26552=CARTESIAN_POINT('Ctrl Pts',(-0.91437591904658,1.,-1.54440491152808));
#26553=CARTESIAN_POINT('Ctrl Pts',(-0.923832188966322,-1.,-1.56065988582509));
#26554=CARTESIAN_POINT('Ctrl Pts',(-0.923832188966322,1.,-1.56065988582509));
#26555=CARTESIAN_POINT('Ctrl Pts',(-0.932246680128849,-1.,-1.57499388385561));
#26556=CARTESIAN_POINT('Ctrl Pts',(-0.932246680128849,1.,-1.57499388385561));
#26557=CARTESIAN_POINT('Ctrl Pts',(-0.939646377909319,-1.,-1.58744937489796));
#26558=CARTESIAN_POINT('Ctrl Pts',(-0.939646377909319,1.,-1.58744937489796));
#26559=CARTESIAN_POINT('Ctrl Pts',(-0.946078063325796,-1.,-1.59810042045408));
#26560=CARTESIAN_POINT('Ctrl Pts',(-0.946078063325796,1.,-1.59810042045408));
#26561=CARTESIAN_POINT('Ctrl Pts',(-0.951613284361248,-1.,-1.60706069897794));
#26562=CARTESIAN_POINT('Ctrl Pts',(-0.951613284361248,1.,-1.60706069897794));
#26563=CARTESIAN_POINT('Ctrl Pts',(-0.956354422921573,-1.,-1.61449324337233));
#26564=CARTESIAN_POINT('Ctrl Pts',(-0.956354422921573,1.,-1.61449324337233));
#26565=CARTESIAN_POINT('Ctrl Pts',(-0.960438326099958,-1.,-1.62061638139929));
#26566=CARTESIAN_POINT('Ctrl Pts',(-0.960438326099958,1.,-1.62061638139929));
#26567=CARTESIAN_POINT('Ctrl Pts',(-0.964046107037821,-1.,-1.6257193066974));
#26568=CARTESIAN_POINT('Ctrl Pts',(-0.964046107037821,1.,-1.6257193066974));
#26569=CARTESIAN_POINT('Ctrl Pts',(-0.967387853228041,-1.,-1.63013849959083));
#26570=CARTESIAN_POINT('Ctrl Pts',(-0.967387853228041,1.,-1.63013849959083));
#26571=CARTESIAN_POINT('Ctrl Pts',(-0.970669715996356,-1.,-1.63420665729609));
#26572=CARTESIAN_POINT('Ctrl Pts',(-0.970669715996356,1.,-1.63420665729609));
#26573=CARTESIAN_POINT('Ctrl Pts',(-0.974066058287501,-1.,-1.63820952658157));
#26574=CARTESIAN_POINT('Ctrl Pts',(-0.974066058287501,1.,-1.63820952658157));
#26575=CARTESIAN_POINT('Ctrl Pts',(-0.977689794120297,-1.,-1.64233990826831));
#26576=CARTESIAN_POINT('Ctrl Pts',(-0.977689794120297,1.,-1.64233990826831));
#26577=CARTESIAN_POINT('Ctrl Pts',(-0.981562530940574,-1.,-1.64665139190834));
#26578=CARTESIAN_POINT('Ctrl Pts',(-0.981562530940574,1.,-1.64665139190834));
#26579=CARTESIAN_POINT('Ctrl Pts',(-0.985642622921626,-1.,-1.6511001661277));
#26580=CARTESIAN_POINT('Ctrl Pts',(-0.985642622921626,1.,-1.6511001661277));
#26581=CARTESIAN_POINT('Ctrl Pts',(-0.98985562785445,-1.,-1.65559044289746));
#26582=CARTESIAN_POINT('Ctrl Pts',(-0.98985562785445,1.,-1.65559044289746));
#26583=CARTESIAN_POINT('Ctrl Pts',(-0.994121836661116,-1.,-1.66001553809916));
#26584=CARTESIAN_POINT('Ctrl Pts',(-0.994121836661116,1.,-1.66001553809916));
#26585=CARTESIAN_POINT('Ctrl Pts',(-0.998389654952317,-1.,-1.66430758030304));
#26586=CARTESIAN_POINT('Ctrl Pts',(-0.998389654952317,1.,-1.66430758030304));
#26587=CARTESIAN_POINT('Ctrl Pts',(-1.00265091003682,-1.,-1.66846059277231));
#26588=CARTESIAN_POINT('Ctrl Pts',(-1.00265091003682,1.,-1.66846059277231));
#26589=CARTESIAN_POINT('Ctrl Pts',(-1.00692206696387,-1.,-1.67250335383248));
#26590=CARTESIAN_POINT('Ctrl Pts',(-1.00692206696387,1.,-1.67250335383248));
#26591=CARTESIAN_POINT('Ctrl Pts',(-1.01123236493507,-1.,-1.67648246776457));
#26592=CARTESIAN_POINT('Ctrl Pts',(-1.01123236493507,1.,-1.67648246776457));
#26593=CARTESIAN_POINT('Ctrl Pts',(-1.01561026162787,-1.,-1.6804428989482));
#26594=CARTESIAN_POINT('Ctrl Pts',(-1.01561026162787,1.,-1.6804428989482));
#26595=CARTESIAN_POINT('Ctrl Pts',(-1.02006795074222,-1.,-1.68440578021739));
#26596=CARTESIAN_POINT('Ctrl Pts',(-1.02006795074222,1.,-1.68440578021739));
#26597=CARTESIAN_POINT('Ctrl Pts',(-1.02460180535272,-1.,-1.68836910178475));
#26598=CARTESIAN_POINT('Ctrl Pts',(-1.02460180535272,1.,-1.68836910178475));
#26599=CARTESIAN_POINT('Ctrl Pts',(-1.02919977579155,-1.,-1.69231840863471));
#26600=CARTESIAN_POINT('Ctrl Pts',(-1.02919977579155,1.,-1.69231840863471));
#26601=CARTESIAN_POINT('Ctrl Pts',(-1.03384646003587,-1.,-1.69623414782769));
#26602=CARTESIAN_POINT('Ctrl Pts',(-1.03384646003587,1.,-1.69623414782769));
#26603=CARTESIAN_POINT('Ctrl Pts',(-1.03852922490782,-1.,-1.70010052930951));
#26604=CARTESIAN_POINT('Ctrl Pts',(-1.03852922490782,1.,-1.70010052930951));
#26605=CARTESIAN_POINT('Ctrl Pts',(-1.04324363334546,-1.,-1.70391338707969));
#26606=CARTESIAN_POINT('Ctrl Pts',(-1.04324363334546,1.,-1.70391338707969));
#26607=CARTESIAN_POINT('Ctrl Pts',(-1.0479908540499,-1.,-1.70767646263641));
#26608=CARTESIAN_POINT('Ctrl Pts',(-1.0479908540499,1.,-1.70767646263641));
#26609=CARTESIAN_POINT('Ctrl Pts',(-1.05277517202854,-1.,-1.71139783543986));
#26610=CARTESIAN_POINT('Ctrl Pts',(-1.05277517202854,1.,-1.71139783543986));
#26611=CARTESIAN_POINT('Ctrl Pts',(-1.05760163192481,-1.,-1.71508654427022));
#26612=CARTESIAN_POINT('Ctrl Pts',(-1.05760163192481,1.,-1.71508654427022));
#26613=CARTESIAN_POINT('Ctrl Pts',(-1.0624732468065,-1.,-1.71874858456908));
#26614=CARTESIAN_POINT('Ctrl Pts',(-1.0624732468065,1.,-1.71874858456908));
#26615=CARTESIAN_POINT('Ctrl Pts',(-1.06738966975463,-1.,-1.72238500928456));
#26616=CARTESIAN_POINT('Ctrl Pts',(-1.06738966975463,1.,-1.72238500928456));
#26617=CARTESIAN_POINT('Ctrl Pts',(-1.07234866990252,-1.,-1.72599406198489));
#26618=CARTESIAN_POINT('Ctrl Pts',(-1.07234866990252,1.,-1.72599406198489));
#26619=CARTESIAN_POINT('Ctrl Pts',(-1.0773470373727,-1.,-1.72957248977424));
#26620=CARTESIAN_POINT('Ctrl Pts',(-1.0773470373727,1.,-1.72957248977424));
#26621=CARTESIAN_POINT('Ctrl Pts',(-1.08238162784749,-1.,-1.73311705663407));
#26622=CARTESIAN_POINT('Ctrl Pts',(-1.08238162784749,1.,-1.73311705663407));
#26623=CARTESIAN_POINT('Ctrl Pts',(-1.08745056285429,-1.,-1.73662628326093));
#26624=CARTESIAN_POINT('Ctrl Pts',(-1.08745056285429,1.,-1.73662628326093));
#26625=CARTESIAN_POINT('Ctrl Pts',(-1.09255329056496,-1.,-1.74010053962252));
#26626=CARTESIAN_POINT('Ctrl Pts',(-1.09255329056496,1.,-1.74010053962252));
#26627=CARTESIAN_POINT('Ctrl Pts',(-1.09768999241229,-1.,-1.74354119236212));
#26628=CARTESIAN_POINT('Ctrl Pts',(-1.09768999241229,1.,-1.74354119236212));
#26629=CARTESIAN_POINT('Ctrl Pts',(-1.10286118991144,-1.,-1.74695004214924));
#26630=CARTESIAN_POINT('Ctrl Pts',(-1.10286118991144,1.,-1.74695004214924));
#26631=CARTESIAN_POINT('Ctrl Pts',(-1.10806728183003,-1.,-1.75032866075914));
#26632=CARTESIAN_POINT('Ctrl Pts',(-1.10806728183003,1.,-1.75032866075914));
#26633=CARTESIAN_POINT('Ctrl Pts',(-1.11330807582542,-1.,-1.75367772094617));
#26634=CARTESIAN_POINT('Ctrl Pts',(-1.11330807582542,1.,-1.75367772094617));
#26635=CARTESIAN_POINT('Ctrl Pts',(-1.11858293216752,-1.,-1.75699720772089));
#26636=CARTESIAN_POINT('Ctrl Pts',(-1.11858293216752,1.,-1.75699720772089));
#26637=CARTESIAN_POINT('Ctrl Pts',(-1.12389096855078,-1.,-1.76028671825084));
#26638=CARTESIAN_POINT('Ctrl Pts',(-1.12389096855078,1.,-1.76028671825084));
#26639=CARTESIAN_POINT('Ctrl Pts',(-1.12923123555076,-1.,-1.76354571966171));
#26640=CARTESIAN_POINT('Ctrl Pts',(-1.12923123555076,1.,-1.76354571966171));
#26641=CARTESIAN_POINT('Ctrl Pts',(-1.13460291804635,-1.,-1.76677384551883));
#26642=CARTESIAN_POINT('Ctrl Pts',(-1.13460291804635,1.,-1.76677384551883));
#26643=CARTESIAN_POINT('Ctrl Pts',(-1.14000548337,-1.,-1.76997111386806));
#26644=CARTESIAN_POINT('Ctrl Pts',(-1.14000548337,1.,-1.76997111386806));
#26645=CARTESIAN_POINT('Ctrl Pts',(-1.14543858226948,-1.,-1.77313777896234));
#26646=CARTESIAN_POINT('Ctrl Pts',(-1.14543858226948,1.,-1.77313777896234));
#26647=CARTESIAN_POINT('Ctrl Pts',(-1.15090197841531,-1.,-1.77627422557034));
#26648=CARTESIAN_POINT('Ctrl Pts',(-1.15090197841531,1.,-1.77627422557034));
#26649=CARTESIAN_POINT('Ctrl Pts',(-1.15639547194689,-1.,-1.77938085564261));
#26650=CARTESIAN_POINT('Ctrl Pts',(-1.15639547194689,1.,-1.77938085564261));
#26651=CARTESIAN_POINT('Ctrl Pts',(-1.16191881298458,-1.,-1.78245795880949));
#26652=CARTESIAN_POINT('Ctrl Pts',(-1.16191881298458,1.,-1.78245795880949));
#26653=CARTESIAN_POINT('Ctrl Pts',(-1.16747166312239,-1.,-1.78550566040349));
#26654=CARTESIAN_POINT('Ctrl Pts',(-1.16747166312239,1.,-1.78550566040349));
#26655=CARTESIAN_POINT('Ctrl Pts',(-1.17305363177265,-1.,-1.78852398877523));
#26656=CARTESIAN_POINT('Ctrl Pts',(-1.17305363177265,1.,-1.78852398877523));
#26657=CARTESIAN_POINT('Ctrl Pts',(-1.17866429440781,-1.,-1.79151291552646));
#26658=CARTESIAN_POINT('Ctrl Pts',(-1.17866429440781,1.,-1.79151291552646));
#26659=CARTESIAN_POINT('Ctrl Pts',(-1.18430321697471,-1.,-1.79447240321572));
#26660=CARTESIAN_POINT('Ctrl Pts',(-1.18430321697471,1.,-1.79447240321572));
#26661=CARTESIAN_POINT('Ctrl Pts',(-1.1899699793456,-1.,-1.79740245923649));
#26662=CARTESIAN_POINT('Ctrl Pts',(-1.1899699793456,1.,-1.79740245923649));
#26663=CARTESIAN_POINT('Ctrl Pts',(-1.19566418930405,-1.,-1.80030314370121));
#26664=CARTESIAN_POINT('Ctrl Pts',(-1.19566418930405,1.,-1.80030314370121));
#26665=CARTESIAN_POINT('Ctrl Pts',(-1.2013854893912,-1.,-1.8031745483882));
#26666=CARTESIAN_POINT('Ctrl Pts',(-1.2013854893912,1.,-1.8031745483882));
#26667=CARTESIAN_POINT('Ctrl Pts',(-1.20713356605519,-1.,-1.80601678480772));
#26668=CARTESIAN_POINT('Ctrl Pts',(-1.20713356605519,1.,-1.80601678480772));
#26669=CARTESIAN_POINT('Ctrl Pts',(-1.2129081570818,-1.,-1.80882996916931));
#26670=CARTESIAN_POINT('Ctrl Pts',(-1.2129081570818,1.,-1.80882996916931));
#26671=CARTESIAN_POINT('Ctrl Pts',(-1.2187090610323,-1.,-1.81161420806172));
#26672=CARTESIAN_POINT('Ctrl Pts',(-1.2187090610323,1.,-1.81161420806172));
#26673=CARTESIAN_POINT('Ctrl Pts',(-1.22453613304507,-1.,-1.81436959209778));
#26674=CARTESIAN_POINT('Ctrl Pts',(-1.22453613304507,1.,-1.81436959209778));
#26675=CARTESIAN_POINT('Ctrl Pts',(-1.22921864890975,-1.,-1.81655087183054));
#26676=CARTESIAN_POINT('Ctrl Pts',(-1.22921864890975,1.,-1.81655087183054));
#26677=CARTESIAN_POINT('Ctrl Pts',(-1.23274224526804,-1.,-1.81817389920914));
#26678=CARTESIAN_POINT('Ctrl Pts',(-1.23274224526804,1.,-1.81817389920914));
#26679=CARTESIAN_POINT('Ctrl Pts',(-1.23509651170384,-1.,-1.81925017193531));
#26680=CARTESIAN_POINT('Ctrl Pts',(-1.23509651170384,1.,-1.81925017193531));
#26681=CARTESIAN_POINT('Ctrl Pts',(-1.23627494547115,-1.,-1.81978687191668));
#26682=CARTESIAN_POINT('Ctrl Pts',(-1.23627494547115,1.,-1.81978687191668));
#26683=CARTESIAN_POINT('',(-0.892032620296855,1.,-1.5055822144029));
#26684=CARTESIAN_POINT('Ctrl Pts',(-0.892032620296855,1.,-1.5055822144029));
#26685=CARTESIAN_POINT('Ctrl Pts',(-0.894452006967538,1.,-1.50980486807181));
#26686=CARTESIAN_POINT('Ctrl Pts',(-0.89918504749193,1.,-1.51805569591479));
#26687=CARTESIAN_POINT('Ctrl Pts',(-0.905967409640499,1.,-1.52984849890434));
#26688=CARTESIAN_POINT('Ctrl Pts',(-0.91437591904658,1.,-1.54440491152808));
#26689=CARTESIAN_POINT('Ctrl Pts',(-0.923832188966322,1.,-1.56065988582509));
#26690=CARTESIAN_POINT('Ctrl Pts',(-0.932246680128849,1.,-1.57499388385561));
#26691=CARTESIAN_POINT('Ctrl Pts',(-0.939646377909319,1.,-1.58744937489796));
#26692=CARTESIAN_POINT('Ctrl Pts',(-0.946078063325796,1.,-1.59810042045408));
#26693=CARTESIAN_POINT('Ctrl Pts',(-0.951613284361248,1.,-1.60706069897794));
#26694=CARTESIAN_POINT('Ctrl Pts',(-0.956354422921573,1.,-1.61449324337233));
#26695=CARTESIAN_POINT('Ctrl Pts',(-0.960438326099958,1.,-1.62061638139929));
#26696=CARTESIAN_POINT('Ctrl Pts',(-0.964046107037821,1.,-1.6257193066974));
#26697=CARTESIAN_POINT('Ctrl Pts',(-0.967387853228041,1.,-1.63013849959083));
#26698=CARTESIAN_POINT('Ctrl Pts',(-0.970669715996356,1.,-1.63420665729609));
#26699=CARTESIAN_POINT('Ctrl Pts',(-0.974066058287501,1.,-1.63820952658157));
#26700=CARTESIAN_POINT('Ctrl Pts',(-0.977689794120297,1.,-1.64233990826831));
#26701=CARTESIAN_POINT('Ctrl Pts',(-0.981562530940574,1.,-1.64665139190834));
#26702=CARTESIAN_POINT('Ctrl Pts',(-0.985642622921626,1.,-1.6511001661277));
#26703=CARTESIAN_POINT('Ctrl Pts',(-0.98985562785445,1.,-1.65559044289746));
#26704=CARTESIAN_POINT('Ctrl Pts',(-0.994121836661116,1.,-1.66001553809916));
#26705=CARTESIAN_POINT('Ctrl Pts',(-0.998389654952317,1.,-1.66430758030304));
#26706=CARTESIAN_POINT('Ctrl Pts',(-1.00265091003682,1.,-1.66846059277231));
#26707=CARTESIAN_POINT('Ctrl Pts',(-1.00692206696387,1.,-1.67250335383248));
#26708=CARTESIAN_POINT('Ctrl Pts',(-1.01123236493507,1.,-1.67648246776457));
#26709=CARTESIAN_POINT('Ctrl Pts',(-1.01561026162787,1.,-1.6804428989482));
#26710=CARTESIAN_POINT('Ctrl Pts',(-1.02006795074222,1.,-1.68440578021739));
#26711=CARTESIAN_POINT('Ctrl Pts',(-1.02460180535272,1.,-1.68836910178475));
#26712=CARTESIAN_POINT('Ctrl Pts',(-1.02919977579155,1.,-1.69231840863471));
#26713=CARTESIAN_POINT('Ctrl Pts',(-1.03384646003587,1.,-1.69623414782769));
#26714=CARTESIAN_POINT('Ctrl Pts',(-1.03852922490782,1.,-1.70010052930951));
#26715=CARTESIAN_POINT('Ctrl Pts',(-1.04324363334546,1.,-1.70391338707969));
#26716=CARTESIAN_POINT('Ctrl Pts',(-1.0479908540499,1.,-1.70767646263641));
#26717=CARTESIAN_POINT('Ctrl Pts',(-1.05277517202854,1.,-1.71139783543986));
#26718=CARTESIAN_POINT('Ctrl Pts',(-1.05760163192481,1.,-1.71508654427022));
#26719=CARTESIAN_POINT('Ctrl Pts',(-1.0624732468065,1.,-1.71874858456908));
#26720=CARTESIAN_POINT('Ctrl Pts',(-1.06738966975463,1.,-1.72238500928456));
#26721=CARTESIAN_POINT('Ctrl Pts',(-1.07234866990252,1.,-1.72599406198489));
#26722=CARTESIAN_POINT('Ctrl Pts',(-1.0773470373727,1.,-1.72957248977424));
#26723=CARTESIAN_POINT('Ctrl Pts',(-1.08238162784749,1.,-1.73311705663407));
#26724=CARTESIAN_POINT('Ctrl Pts',(-1.08745056285429,1.,-1.73662628326093));
#26725=CARTESIAN_POINT('Ctrl Pts',(-1.09255329056496,1.,-1.74010053962252));
#26726=CARTESIAN_POINT('Ctrl Pts',(-1.09768999241229,1.,-1.74354119236212));
#26727=CARTESIAN_POINT('Ctrl Pts',(-1.10286118991144,1.,-1.74695004214924));
#26728=CARTESIAN_POINT('Ctrl Pts',(-1.10806728183003,1.,-1.75032866075914));
#26729=CARTESIAN_POINT('Ctrl Pts',(-1.11330807582542,1.,-1.75367772094617));
#26730=CARTESIAN_POINT('Ctrl Pts',(-1.11858293216752,1.,-1.75699720772089));
#26731=CARTESIAN_POINT('Ctrl Pts',(-1.12389096855078,1.,-1.76028671825084));
#26732=CARTESIAN_POINT('Ctrl Pts',(-1.12923123555076,1.,-1.76354571966171));
#26733=CARTESIAN_POINT('Ctrl Pts',(-1.13460291804635,1.,-1.76677384551883));
#26734=CARTESIAN_POINT('Ctrl Pts',(-1.14000548337,1.,-1.76997111386806));
#26735=CARTESIAN_POINT('Ctrl Pts',(-1.14543858226948,1.,-1.77313777896234));
#26736=CARTESIAN_POINT('Ctrl Pts',(-1.15090197841531,1.,-1.77627422557034));
#26737=CARTESIAN_POINT('Ctrl Pts',(-1.15639547194689,1.,-1.77938085564261));
#26738=CARTESIAN_POINT('Ctrl Pts',(-1.16191881298458,1.,-1.78245795880949));
#26739=CARTESIAN_POINT('Ctrl Pts',(-1.16747166312239,1.,-1.78550566040349));
#26740=CARTESIAN_POINT('Ctrl Pts',(-1.17305363177265,1.,-1.78852398877523));
#26741=CARTESIAN_POINT('Ctrl Pts',(-1.17866429440781,1.,-1.79151291552646));
#26742=CARTESIAN_POINT('Ctrl Pts',(-1.18430321697471,1.,-1.79447240321572));
#26743=CARTESIAN_POINT('Ctrl Pts',(-1.1899699793456,1.,-1.79740245923649));
#26744=CARTESIAN_POINT('Ctrl Pts',(-1.19566418930405,1.,-1.80030314370121));
#26745=CARTESIAN_POINT('Ctrl Pts',(-1.2013854893912,1.,-1.8031745483882));
#26746=CARTESIAN_POINT('Ctrl Pts',(-1.20713356605519,1.,-1.80601678480772));
#26747=CARTESIAN_POINT('Ctrl Pts',(-1.2129081570818,1.,-1.80882996916931));
#26748=CARTESIAN_POINT('Ctrl Pts',(-1.2187090610323,1.,-1.81161420806172));
#26749=CARTESIAN_POINT('Ctrl Pts',(-1.22453613304507,1.,-1.81436959209778));
#26750=CARTESIAN_POINT('Ctrl Pts',(-1.22921864890975,1.,-1.81655087183054));
#26751=CARTESIAN_POINT('Ctrl Pts',(-1.23274224526804,1.,-1.81817389920914));
#26752=CARTESIAN_POINT('Ctrl Pts',(-1.23509651170384,1.,-1.81925017193531));
#26753=CARTESIAN_POINT('Ctrl Pts',(-1.23627494547115,1.,-1.81978687191668));
#26754=CARTESIAN_POINT('',(-0.892032620296856,0.,-1.5055822144029));
#26755=CARTESIAN_POINT('Origin',(0.,0.,0.));
#26756=CARTESIAN_POINT('',(-0.693717979106305,1.,-1.60662857109684));
#26757=CARTESIAN_POINT('Origin',(0.,1.,0.));
#26758=CARTESIAN_POINT('',(-0.693717979106306,0.,-1.60662857109684));
#26759=CARTESIAN_POINT('Ctrl Pts',(-0.745574324794401,-1.,-2.0698113262342));
#26760=CARTESIAN_POINT('Ctrl Pts',(-0.745574324794401,1.,-2.0698113262342));
#26761=CARTESIAN_POINT('Ctrl Pts',(-0.745832791378367,-1.,-2.06854248895728));
#26762=CARTESIAN_POINT('Ctrl Pts',(-0.745832791378367,1.,-2.06854248895728));
#26763=CARTESIAN_POINT('Ctrl Pts',(-0.7463458715442,-1.,-2.06600523016815));
#26764=CARTESIAN_POINT('Ctrl Pts',(-0.7463458715442,1.,-2.06600523016815));
#26765=CARTESIAN_POINT('Ctrl Pts',(-0.747103932787919,-1.,-2.06220058927826));
#26766=CARTESIAN_POINT('Ctrl Pts',(-0.747103932787919,1.,-2.06220058927826));
#26767=CARTESIAN_POINT('Ctrl Pts',(-0.748091554183802,-1.,-2.05713023031006));
#26768=CARTESIAN_POINT('Ctrl Pts',(-0.748091554183802,1.,-2.05713023031006));
#26769=CARTESIAN_POINT('Ctrl Pts',(-0.749287468665046,-1.,-2.05079645592154));
#26770=CARTESIAN_POINT('Ctrl Pts',(-0.749287468665046,1.,-2.05079645592154));
#26771=CARTESIAN_POINT('Ctrl Pts',(-0.750444657875576,-1.,-2.04446689147979));
#26772=CARTESIAN_POINT('Ctrl Pts',(-0.750444657875576,1.,-2.04446689147979));
#26773=CARTESIAN_POINT('Ctrl Pts',(-0.751562963361115,-1.,-2.03814160092099));
#26774=CARTESIAN_POINT('Ctrl Pts',(-0.751562963361115,1.,-2.03814160092099));
#26775=CARTESIAN_POINT('Ctrl Pts',(-0.752642180487211,-1.,-2.03182068456221));
#26776=CARTESIAN_POINT('Ctrl Pts',(-0.752642180487211,1.,-2.03182068456221));
#26777=CARTESIAN_POINT('Ctrl Pts',(-0.753682061112768,-1.,-2.02550428623313));
#26778=CARTESIAN_POINT('Ctrl Pts',(-0.753682061112768,1.,-2.02550428623313));
#26779=CARTESIAN_POINT('Ctrl Pts',(-0.754682330722816,-1.,-2.01919259405809));
#26780=CARTESIAN_POINT('Ctrl Pts',(-0.754682330722816,1.,-2.01919259405809));
#26781=CARTESIAN_POINT('Ctrl Pts',(-0.755642704957865,-1.,-2.01288584328084));
#26782=CARTESIAN_POINT('Ctrl Pts',(-0.755642704957865,1.,-2.01288584328084));
#26783=CARTESIAN_POINT('Ctrl Pts',(-0.75656290464667,-1.,-2.0065843158773));
#26784=CARTESIAN_POINT('Ctrl Pts',(-0.75656290464667,1.,-2.0065843158773));
#26785=CARTESIAN_POINT('Ctrl Pts',(-0.757442676862724,-1.,-2.00028834739178));
#26786=CARTESIAN_POINT('Ctrl Pts',(-0.757442676862724,1.,-2.00028834739178));
#26787=CARTESIAN_POINT('Ctrl Pts',(-0.758281796766761,-1.,-1.99399831098817));
#26788=CARTESIAN_POINT('Ctrl Pts',(-0.758281796766761,1.,-1.99399831098817));
#26789=CARTESIAN_POINT('Ctrl Pts',(-0.759080037802488,-1.,-1.98771456680874));
#26790=CARTESIAN_POINT('Ctrl Pts',(-0.759080037802488,1.,-1.98771456680874));
#26791=CARTESIAN_POINT('Ctrl Pts',(-0.75983714745219,-1.,-1.98143741418172));
#26792=CARTESIAN_POINT('Ctrl Pts',(-0.75983714745219,1.,-1.98143741418172));
#26793=CARTESIAN_POINT('Ctrl Pts',(-0.760552825409757,-1.,-1.97516705321494));
#26794=CARTESIAN_POINT('Ctrl Pts',(-0.760552825409757,1.,-1.97516705321494));
#26795=CARTESIAN_POINT('Ctrl Pts',(-0.76122669048382,-1.,-1.96890351582499));
#26796=CARTESIAN_POINT('Ctrl Pts',(-0.76122669048382,1.,-1.96890351582499));
#26797=CARTESIAN_POINT('Ctrl Pts',(-0.761858300014423,-1.,-1.96264672744186));
#26798=CARTESIAN_POINT('Ctrl Pts',(-0.761858300014423,1.,-1.96264672744186));
#26799=CARTESIAN_POINT('Ctrl Pts',(-0.762447203806179,-1.,-1.95639665309869));
#26800=CARTESIAN_POINT('Ctrl Pts',(-0.762447203806179,1.,-1.95639665309869));
#26801=CARTESIAN_POINT('Ctrl Pts',(-0.762992990878769,-1.,-1.95015342590024));
#26802=CARTESIAN_POINT('Ctrl Pts',(-0.762992990878769,1.,-1.95015342590024));
#26803=CARTESIAN_POINT('Ctrl Pts',(-0.763495333538629,-1.,-1.9439174661764));
#26804=CARTESIAN_POINT('Ctrl Pts',(-0.763495333538629,1.,-1.9439174661764));
#26805=CARTESIAN_POINT('Ctrl Pts',(-0.763954049121458,-1.,-1.93768964875886));
#26806=CARTESIAN_POINT('Ctrl Pts',(-0.763954049121458,1.,-1.93768964875886));
#26807=CARTESIAN_POINT('Ctrl Pts',(-0.764369010673941,-1.,-1.93147105496382));
#26808=CARTESIAN_POINT('Ctrl Pts',(-0.764369010673941,1.,-1.93147105496382));
#26809=CARTESIAN_POINT('Ctrl Pts',(-0.764740025488211,-1.,-1.92526263537048));
#26810=CARTESIAN_POINT('Ctrl Pts',(-0.764740025488211,1.,-1.92526263537048));
#26811=CARTESIAN_POINT('Ctrl Pts',(-0.765066729667088,-1.,-1.91906491634196));
#26812=CARTESIAN_POINT('Ctrl Pts',(-0.765066729667088,1.,-1.91906491634196));
#26813=CARTESIAN_POINT('Ctrl Pts',(-0.765348465884722,-1.,-1.91287765805169));
#26814=CARTESIAN_POINT('Ctrl Pts',(-0.765348465884722,1.,-1.91287765805169));
#26815=CARTESIAN_POINT('Ctrl Pts',(-0.765584196937919,-1.,-1.90669961402356));
#26816=CARTESIAN_POINT('Ctrl Pts',(-0.765584196937919,1.,-1.90669961402356));
#26817=CARTESIAN_POINT('Ctrl Pts',(-0.765772772593386,-1.,-1.90052930393596));
#26818=CARTESIAN_POINT('Ctrl Pts',(-0.765772772593386,1.,-1.90052930393596));
#26819=CARTESIAN_POINT('Ctrl Pts',(-0.765913193856978,-1.,-1.89436577771388));
#26820=CARTESIAN_POINT('Ctrl Pts',(-0.765913193856978,1.,-1.89436577771388));
#26821=CARTESIAN_POINT('Ctrl Pts',(-0.766004837062091,-1.,-1.88820926433409));
#26822=CARTESIAN_POINT('Ctrl Pts',(-0.766004837062091,1.,-1.88820926433409));
#26823=CARTESIAN_POINT('Ctrl Pts',(-0.766047794851865,-1.,-1.88206215302561));
#26824=CARTESIAN_POINT('Ctrl Pts',(-0.766047794851865,1.,-1.88206215302561));
#26825=CARTESIAN_POINT('Ctrl Pts',(-0.766042837036744,-1.,-1.87592888967883));
#26826=CARTESIAN_POINT('Ctrl Pts',(-0.766042837036744,1.,-1.87592888967883));
#26827=CARTESIAN_POINT('Ctrl Pts',(-0.765990708546091,-1.,-1.86981398314341));
#26828=CARTESIAN_POINT('Ctrl Pts',(-0.765990708546091,1.,-1.86981398314341));
#26829=CARTESIAN_POINT('Ctrl Pts',(-0.765891519092547,-1.,-1.86372027063312));
#26830=CARTESIAN_POINT('Ctrl Pts',(-0.765891519092547,1.,-1.86372027063312));
#26831=CARTESIAN_POINT('Ctrl Pts',(-0.765744212909318,-1.,-1.85764741390394));
#26832=CARTESIAN_POINT('Ctrl Pts',(-0.765744212909318,1.,-1.85764741390394));
#26833=CARTESIAN_POINT('Ctrl Pts',(-0.765545710619062,-1.,-1.85158945130063));
#26834=CARTESIAN_POINT('Ctrl Pts',(-0.765545710619062,1.,-1.85158945130063));
#26835=CARTESIAN_POINT('Ctrl Pts',(-0.765291664862029,-1.,-1.84553698875924));
#26836=CARTESIAN_POINT('Ctrl Pts',(-0.765291664862029,1.,-1.84553698875924));
#26837=CARTESIAN_POINT('Ctrl Pts',(-0.764978057881737,-1.,-1.83948181064835));
#26838=CARTESIAN_POINT('Ctrl Pts',(-0.764978057881737,1.,-1.83948181064835));
#26839=CARTESIAN_POINT('Ctrl Pts',(-0.764602549687853,-1.,-1.83342077227142));
#26840=CARTESIAN_POINT('Ctrl Pts',(-0.764602549687853,1.,-1.83342077227142));
#26841=CARTESIAN_POINT('Ctrl Pts',(-0.764165902605995,-1.,-1.82735991200065));
#26842=CARTESIAN_POINT('Ctrl Pts',(-0.764165902605995,1.,-1.82735991200065));
#26843=CARTESIAN_POINT('Ctrl Pts',(-0.763673465462726,-1.,-1.82131873145266));
#26844=CARTESIAN_POINT('Ctrl Pts',(-0.763673465462726,1.,-1.82131873145266));
#26845=CARTESIAN_POINT('Ctrl Pts',(-0.763132003836634,-1.,-1.8153211840553));
#26846=CARTESIAN_POINT('Ctrl Pts',(-0.763132003836634,1.,-1.8153211840553));
#26847=CARTESIAN_POINT('Ctrl Pts',(-0.762546129463938,-1.,-1.80938551463965));
#26848=CARTESIAN_POINT('Ctrl Pts',(-0.762546129463938,1.,-1.80938551463965));
#26849=CARTESIAN_POINT('Ctrl Pts',(-0.761915336443547,-1.,-1.80351583877342));
#26850=CARTESIAN_POINT('Ctrl Pts',(-0.761915336443547,1.,-1.80351583877342));
#26851=CARTESIAN_POINT('Ctrl Pts',(-0.761229695230558,-1.,-1.79768986997783));
#26852=CARTESIAN_POINT('Ctrl Pts',(-0.761229695230558,1.,-1.79768986997783));
#26853=CARTESIAN_POINT('Ctrl Pts',(-0.760469555880749,-1.,-1.7918581561088));
#26854=CARTESIAN_POINT('Ctrl Pts',(-0.760469555880749,1.,-1.7918581561088));
#26855=CARTESIAN_POINT('Ctrl Pts',(-0.759614401110189,-1.,-1.78596964884604));
#26856=CARTESIAN_POINT('Ctrl Pts',(-0.759614401110189,1.,-1.78596964884604));
#26857=CARTESIAN_POINT('Ctrl Pts',(-0.758650626677518,-1.,-1.77999411220945));
#26858=CARTESIAN_POINT('Ctrl Pts',(-0.758650626677518,1.,-1.77999411220945));
#26859=CARTESIAN_POINT('Ctrl Pts',(-0.757578264077029,-1.,-1.77394167108292));
#26860=CARTESIAN_POINT('Ctrl Pts',(-0.757578264077029,1.,-1.77394167108292));
#26861=CARTESIAN_POINT('Ctrl Pts',(-0.75642189602781,-1.,-1.76789396002998));
#26862=CARTESIAN_POINT('Ctrl Pts',(-0.75642189602781,1.,-1.76789396002998));
#26863=CARTESIAN_POINT('Ctrl Pts',(-0.755220979974461,-1.,-1.76197817240128));
#26864=CARTESIAN_POINT('Ctrl Pts',(-0.755220979974461,1.,-1.76197817240128));
#26865=CARTESIAN_POINT('Ctrl Pts',(-0.754009254027829,-1.,-1.75631083600019));
#26866=CARTESIAN_POINT('Ctrl Pts',(-0.754009254027829,1.,-1.75631083600019));
#26867=CARTESIAN_POINT('Ctrl Pts',(-0.752797683531314,-1.,-1.75095139468794));
#26868=CARTESIAN_POINT('Ctrl Pts',(-0.752797683531314,1.,-1.75095139468794));
#26869=CARTESIAN_POINT('Ctrl Pts',(-0.751555614164482,-1.,-1.74585086852502));
#26870=CARTESIAN_POINT('Ctrl Pts',(-0.751555614164482,1.,-1.74585086852502));
#26871=CARTESIAN_POINT('Ctrl Pts',(-0.750193435981249,-1.,-1.74080458267114));
#26872=CARTESIAN_POINT('Ctrl Pts',(-0.750193435981249,1.,-1.74080458267114));
#26873=CARTESIAN_POINT('Ctrl Pts',(-0.74858246295687,-1.,-1.7355035168033));
#26874=CARTESIAN_POINT('Ctrl Pts',(-0.74858246295687,1.,-1.7355035168033));
#26875=CARTESIAN_POINT('Ctrl Pts',(-0.746574710097752,-1.,-1.72958533647714));
#26876=CARTESIAN_POINT('Ctrl Pts',(-0.746574710097752,1.,-1.72958533647714));
#26877=CARTESIAN_POINT('Ctrl Pts',(-0.744021445433093,-1.,-1.72268229916769));
#26878=CARTESIAN_POINT('Ctrl Pts',(-0.744021445433093,1.,-1.72268229916769));
#26879=CARTESIAN_POINT('Ctrl Pts',(-0.74079516202821,-1.,-1.71447789751001));
#26880=CARTESIAN_POINT('Ctrl Pts',(-0.74079516202821,1.,-1.71447789751001));
#26881=CARTESIAN_POINT('Ctrl Pts',(-0.736799665716932,-1.,-1.70473309004249));
#26882=CARTESIAN_POINT('Ctrl Pts',(-0.736799665716932,1.,-1.70473309004249));
#26883=CARTESIAN_POINT('Ctrl Pts',(-0.731963238685357,-1.,-1.69326921972915));
#26884=CARTESIAN_POINT('Ctrl Pts',(-0.731963238685357,1.,-1.69326921972915));
#26885=CARTESIAN_POINT('Ctrl Pts',(-0.726235967982445,-1.,-1.67996158451922));
#26886=CARTESIAN_POINT('Ctrl Pts',(-0.726235967982445,1.,-1.67996158451922));
#26887=CARTESIAN_POINT('Ctrl Pts',(-0.71958543378795,-1.,-1.66472880551777));
#26888=CARTESIAN_POINT('Ctrl Pts',(-0.71958543378795,1.,-1.66472880551777));
#26889=CARTESIAN_POINT('Ctrl Pts',(-0.711993139340447,-1.,-1.64752408828442));
#26890=CARTESIAN_POINT('Ctrl Pts',(-0.711993139340447,1.,-1.64752408828442));
#26891=CARTESIAN_POINT('Ctrl Pts',(-0.705159151977294,-1.,-1.6321654166204));
#26892=CARTESIAN_POINT('Ctrl Pts',(-0.705159151977294,1.,-1.6321654166204));
#26893=CARTESIAN_POINT('Ctrl Pts',(-0.699605146398837,-1.,-1.61974673471117));
#26894=CARTESIAN_POINT('Ctrl Pts',(-0.699605146398837,1.,-1.61974673471117));
#26895=CARTESIAN_POINT('Ctrl Pts',(-0.69571209787897,-1.,-1.61106790957619));
#26896=CARTESIAN_POINT('Ctrl Pts',(-0.69571209787897,1.,-1.61106790957619));
#26897=CARTESIAN_POINT('Ctrl Pts',(-0.693717979106305,-1.,-1.60662857109684));
#26898=CARTESIAN_POINT('Ctrl Pts',(-0.693717979106305,1.,-1.60662857109684));
#26899=CARTESIAN_POINT('',(-0.745574324794401,1.,-2.0698113262342));
#26900=CARTESIAN_POINT('Ctrl Pts',(-0.745574324794401,1.,-2.0698113262342));
#26901=CARTESIAN_POINT('Ctrl Pts',(-0.745832791378367,1.,-2.06854248895728));
#26902=CARTESIAN_POINT('Ctrl Pts',(-0.7463458715442,1.,-2.06600523016815));
#26903=CARTESIAN_POINT('Ctrl Pts',(-0.747103932787919,1.,-2.06220058927826));
#26904=CARTESIAN_POINT('Ctrl Pts',(-0.748091554183802,1.,-2.05713023031006));
#26905=CARTESIAN_POINT('Ctrl Pts',(-0.749287468665046,1.,-2.05079645592154));
#26906=CARTESIAN_POINT('Ctrl Pts',(-0.750444657875576,1.,-2.04446689147979));
#26907=CARTESIAN_POINT('Ctrl Pts',(-0.751562963361115,1.,-2.03814160092099));
#26908=CARTESIAN_POINT('Ctrl Pts',(-0.752642180487211,1.,-2.03182068456221));
#26909=CARTESIAN_POINT('Ctrl Pts',(-0.753682061112768,1.,-2.02550428623313));
#26910=CARTESIAN_POINT('Ctrl Pts',(-0.754682330722816,1.,-2.01919259405809));
#26911=CARTESIAN_POINT('Ctrl Pts',(-0.755642704957865,1.,-2.01288584328084));
#26912=CARTESIAN_POINT('Ctrl Pts',(-0.75656290464667,1.,-2.0065843158773));
#26913=CARTESIAN_POINT('Ctrl Pts',(-0.757442676862724,1.,-2.00028834739178));
#26914=CARTESIAN_POINT('Ctrl Pts',(-0.758281796766761,1.,-1.99399831098817));
#26915=CARTESIAN_POINT('Ctrl Pts',(-0.759080037802488,1.,-1.98771456680874));
#26916=CARTESIAN_POINT('Ctrl Pts',(-0.75983714745219,1.,-1.98143741418172));
#26917=CARTESIAN_POINT('Ctrl Pts',(-0.760552825409757,1.,-1.97516705321494));
#26918=CARTESIAN_POINT('Ctrl Pts',(-0.76122669048382,1.,-1.96890351582499));
#26919=CARTESIAN_POINT('Ctrl Pts',(-0.761858300014423,1.,-1.96264672744186));
#26920=CARTESIAN_POINT('Ctrl Pts',(-0.762447203806179,1.,-1.95639665309869));
#26921=CARTESIAN_POINT('Ctrl Pts',(-0.762992990878769,1.,-1.95015342590024));
#26922=CARTESIAN_POINT('Ctrl Pts',(-0.763495333538629,1.,-1.9439174661764));
#26923=CARTESIAN_POINT('Ctrl Pts',(-0.763954049121458,1.,-1.93768964875886));
#26924=CARTESIAN_POINT('Ctrl Pts',(-0.764369010673941,1.,-1.93147105496382));
#26925=CARTESIAN_POINT('Ctrl Pts',(-0.764740025488211,1.,-1.92526263537048));
#26926=CARTESIAN_POINT('Ctrl Pts',(-0.765066729667088,1.,-1.91906491634196));
#26927=CARTESIAN_POINT('Ctrl Pts',(-0.765348465884722,1.,-1.91287765805169));
#26928=CARTESIAN_POINT('Ctrl Pts',(-0.765584196937919,1.,-1.90669961402356));
#26929=CARTESIAN_POINT('Ctrl Pts',(-0.765772772593386,1.,-1.90052930393596));
#26930=CARTESIAN_POINT('Ctrl Pts',(-0.765913193856978,1.,-1.89436577771388));
#26931=CARTESIAN_POINT('Ctrl Pts',(-0.766004837062091,1.,-1.88820926433409));
#26932=CARTESIAN_POINT('Ctrl Pts',(-0.766047794851865,1.,-1.88206215302561));
#26933=CARTESIAN_POINT('Ctrl Pts',(-0.766042837036744,1.,-1.87592888967883));
#26934=CARTESIAN_POINT('Ctrl Pts',(-0.765990708546091,1.,-1.86981398314341));
#26935=CARTESIAN_POINT('Ctrl Pts',(-0.765891519092547,1.,-1.86372027063312));
#26936=CARTESIAN_POINT('Ctrl Pts',(-0.765744212909318,1.,-1.85764741390394));
#26937=CARTESIAN_POINT('Ctrl Pts',(-0.765545710619062,1.,-1.85158945130063));
#26938=CARTESIAN_POINT('Ctrl Pts',(-0.765291664862029,1.,-1.84553698875924));
#26939=CARTESIAN_POINT('Ctrl Pts',(-0.764978057881737,1.,-1.83948181064835));
#26940=CARTESIAN_POINT('Ctrl Pts',(-0.764602549687853,1.,-1.83342077227142));
#26941=CARTESIAN_POINT('Ctrl Pts',(-0.764165902605995,1.,-1.82735991200065));
#26942=CARTESIAN_POINT('Ctrl Pts',(-0.763673465462726,1.,-1.82131873145266));
#26943=CARTESIAN_POINT('Ctrl Pts',(-0.763132003836634,1.,-1.8153211840553));
#26944=CARTESIAN_POINT('Ctrl Pts',(-0.762546129463938,1.,-1.80938551463965));
#26945=CARTESIAN_POINT('Ctrl Pts',(-0.761915336443547,1.,-1.80351583877342));
#26946=CARTESIAN_POINT('Ctrl Pts',(-0.761229695230558,1.,-1.79768986997783));
#26947=CARTESIAN_POINT('Ctrl Pts',(-0.760469555880749,1.,-1.7918581561088));
#26948=CARTESIAN_POINT('Ctrl Pts',(-0.759614401110189,1.,-1.78596964884604));
#26949=CARTESIAN_POINT('Ctrl Pts',(-0.758650626677518,1.,-1.77999411220945));
#26950=CARTESIAN_POINT('Ctrl Pts',(-0.757578264077029,1.,-1.77394167108292));
#26951=CARTESIAN_POINT('Ctrl Pts',(-0.75642189602781,1.,-1.76789396002998));
#26952=CARTESIAN_POINT('Ctrl Pts',(-0.755220979974461,1.,-1.76197817240128));
#26953=CARTESIAN_POINT('Ctrl Pts',(-0.754009254027829,1.,-1.75631083600019));
#26954=CARTESIAN_POINT('Ctrl Pts',(-0.752797683531314,1.,-1.75095139468794));
#26955=CARTESIAN_POINT('Ctrl Pts',(-0.751555614164482,1.,-1.74585086852502));
#26956=CARTESIAN_POINT('Ctrl Pts',(-0.750193435981249,1.,-1.74080458267114));
#26957=CARTESIAN_POINT('Ctrl Pts',(-0.74858246295687,1.,-1.7355035168033));
#26958=CARTESIAN_POINT('Ctrl Pts',(-0.746574710097752,1.,-1.72958533647714));
#26959=CARTESIAN_POINT('Ctrl Pts',(-0.744021445433093,1.,-1.72268229916769));
#26960=CARTESIAN_POINT('Ctrl Pts',(-0.74079516202821,1.,-1.71447789751001));
#26961=CARTESIAN_POINT('Ctrl Pts',(-0.736799665716932,1.,-1.70473309004249));
#26962=CARTESIAN_POINT('Ctrl Pts',(-0.731963238685357,1.,-1.69326921972915));
#26963=CARTESIAN_POINT('Ctrl Pts',(-0.726235967982445,1.,-1.67996158451922));
#26964=CARTESIAN_POINT('Ctrl Pts',(-0.71958543378795,1.,-1.66472880551777));
#26965=CARTESIAN_POINT('Ctrl Pts',(-0.711993139340447,1.,-1.64752408828442));
#26966=CARTESIAN_POINT('Ctrl Pts',(-0.705159151977294,1.,-1.6321654166204));
#26967=CARTESIAN_POINT('Ctrl Pts',(-0.699605146398837,1.,-1.61974673471117));
#26968=CARTESIAN_POINT('Ctrl Pts',(-0.69571209787897,1.,-1.61106790957619));
#26969=CARTESIAN_POINT('Ctrl Pts',(-0.693717979106305,1.,-1.60662857109684));
#26970=CARTESIAN_POINT('',(-0.745574324794401,0.,-2.0698113262342));
#26971=CARTESIAN_POINT('Origin',(-0.61342227326009,0.,-2.11275013067528));
#26972=CARTESIAN_POINT('',(-0.61342227326009,1.,-2.11275013067528));
#26973=CARTESIAN_POINT('',(-0.745574324794401,1.,-2.0698113262342));
#26974=CARTESIAN_POINT('',(-0.61342227326009,0.,-2.11275013067528));
#26975=CARTESIAN_POINT('Ctrl Pts',(-0.383122945602004,-1.,-1.7075470150345));
#26976=CARTESIAN_POINT('Ctrl Pts',(-0.383122945602004,1.,-1.7075470150345));
#26977=CARTESIAN_POINT('Ctrl Pts',(-0.384119047315542,-1.,-1.71231062891958));
#26978=CARTESIAN_POINT('Ctrl Pts',(-0.384119047315542,1.,-1.71231062891958));
#26979=CARTESIAN_POINT('Ctrl Pts',(-0.38607079032701,-1.,-1.72162022246158));
#26980=CARTESIAN_POINT('Ctrl Pts',(-0.38607079032701,1.,-1.72162022246158));
#26981=CARTESIAN_POINT('Ctrl Pts',(-0.388877023509191,-1.,-1.7349317097561));
#26982=CARTESIAN_POINT('Ctrl Pts',(-0.388877023509191,1.,-1.7349317097561));
#26983=CARTESIAN_POINT('Ctrl Pts',(-0.392375812294307,-1.,-1.75137405313962));
#26984=CARTESIAN_POINT('Ctrl Pts',(-0.392375812294307,1.,-1.75137405313962));
#26985=CARTESIAN_POINT('Ctrl Pts',(-0.39634619612042,-1.,-1.7697556004756));
#26986=CARTESIAN_POINT('Ctrl Pts',(-0.39634619612042,1.,-1.7697556004756));
#26987=CARTESIAN_POINT('Ctrl Pts',(-0.39991940378308,-1.,-1.78598826347533));
#26988=CARTESIAN_POINT('Ctrl Pts',(-0.39991940378308,1.,-1.78598826347533));
#26989=CARTESIAN_POINT('Ctrl Pts',(-0.403107976170441,-1.,-1.80012077176221));
#26990=CARTESIAN_POINT('Ctrl Pts',(-0.403107976170441,1.,-1.80012077176221));
#26991=CARTESIAN_POINT('Ctrl Pts',(-0.405933518411838,-1.,-1.81223801813988));
#26992=CARTESIAN_POINT('Ctrl Pts',(-0.405933518411838,1.,-1.81223801813988));
#26993=CARTESIAN_POINT('Ctrl Pts',(-0.408428948108533,-1.,-1.8224702267854));
#26994=CARTESIAN_POINT('Ctrl Pts',(-0.408428948108533,1.,-1.8224702267854));
#26995=CARTESIAN_POINT('Ctrl Pts',(-0.410641256301675,-1.,-1.83100408895216));
#26996=CARTESIAN_POINT('Ctrl Pts',(-0.410641256301675,1.,-1.83100408895216));
#26997=CARTESIAN_POINT('Ctrl Pts',(-0.412633125322162,-1.,-1.83808953475839));
#26998=CARTESIAN_POINT('Ctrl Pts',(-0.412633125322162,1.,-1.83808953475839));
#26999=CARTESIAN_POINT('Ctrl Pts',(-0.41448743825434,-1.,-1.8440575707371));
#27000=CARTESIAN_POINT('Ctrl Pts',(-0.41448743825434,1.,-1.8440575707371));
#27001=CARTESIAN_POINT('Ctrl Pts',(-0.416300022038864,-1.,-1.84929312929882));
#27002=CARTESIAN_POINT('Ctrl Pts',(-0.416300022038864,1.,-1.84929312929882));
#27003=CARTESIAN_POINT('Ctrl Pts',(-0.418164129143534,-1.,-1.85417632856234));
#27004=CARTESIAN_POINT('Ctrl Pts',(-0.418164129143534,1.,-1.85417632856234));
#27005=CARTESIAN_POINT('Ctrl Pts',(-0.420157287975619,-1.,-1.85903281096686));
#27006=CARTESIAN_POINT('Ctrl Pts',(-0.420157287975619,1.,-1.85903281096686));
#27007=CARTESIAN_POINT('Ctrl Pts',(-0.422327307418275,-1.,-1.86408083334028));
#27008=CARTESIAN_POINT('Ctrl Pts',(-0.422327307418275,1.,-1.86408083334028));
#27009=CARTESIAN_POINT('Ctrl Pts',(-0.424678177291359,-1.,-1.86937803944323));
#27010=CARTESIAN_POINT('Ctrl Pts',(-0.424678177291359,1.,-1.86937803944323));
#27011=CARTESIAN_POINT('Ctrl Pts',(-0.427183828519102,-1.,-1.87486989291484));
#27012=CARTESIAN_POINT('Ctrl Pts',(-0.427183828519102,1.,-1.87486989291484));
#27013=CARTESIAN_POINT('Ctrl Pts',(-0.429803062482344,-1.,-1.88044229001832));
#27014=CARTESIAN_POINT('Ctrl Pts',(-0.429803062482344,1.,-1.88044229001832));
#27015=CARTESIAN_POINT('Ctrl Pts',(-0.432493038548748,-1.,-1.88596913666793));
#27016=CARTESIAN_POINT('Ctrl Pts',(-0.432493038548748,1.,-1.88596913666793));
#27017=CARTESIAN_POINT('Ctrl Pts',(-0.435225660963383,-1.,-1.89136993975504));
#27018=CARTESIAN_POINT('Ctrl Pts',(-0.435225660963383,1.,-1.89136993975504));
#27019=CARTESIAN_POINT('Ctrl Pts',(-0.437995003948244,-1.,-1.89663648956466));
#27020=CARTESIAN_POINT('Ctrl Pts',(-0.437995003948244,1.,-1.89663648956466));
#27021=CARTESIAN_POINT('Ctrl Pts',(-0.440807833704038,-1.,-1.90180124389086));
#27022=CARTESIAN_POINT('Ctrl Pts',(-0.440807833704038,1.,-1.90180124389086));
#27023=CARTESIAN_POINT('Ctrl Pts',(-0.443677556849151,-1.,-1.90691756144898));
#27024=CARTESIAN_POINT('Ctrl Pts',(-0.443677556849151,1.,-1.90691756144898));
#27025=CARTESIAN_POINT('Ctrl Pts',(-0.446617343485711,-1.,-1.9120369998112));
#27026=CARTESIAN_POINT('Ctrl Pts',(-0.446617343485711,1.,-1.9120369998112));
#27027=CARTESIAN_POINT('Ctrl Pts',(-0.449632260106662,-1.,-1.91718342555755));
#27028=CARTESIAN_POINT('Ctrl Pts',(-0.449632260106662,1.,-1.91718342555755));
#27029=CARTESIAN_POINT('Ctrl Pts',(-0.452719478359432,-1.,-1.92235380648502));
#27030=CARTESIAN_POINT('Ctrl Pts',(-0.452719478359432,1.,-1.92235380648502));
#27031=CARTESIAN_POINT('Ctrl Pts',(-0.455872005174371,-1.,-1.92753067150476));
#27032=CARTESIAN_POINT('Ctrl Pts',(-0.455872005174371,1.,-1.92753067150476));
#27033=CARTESIAN_POINT('Ctrl Pts',(-0.459081234547926,-1.,-1.93269066517934));
#27034=CARTESIAN_POINT('Ctrl Pts',(-0.459081234547926,1.,-1.93269066517934));
#27035=CARTESIAN_POINT('Ctrl Pts',(-0.462340031009056,-1.,-1.93781486640821));
#27036=CARTESIAN_POINT('Ctrl Pts',(-0.462340031009056,1.,-1.93781486640821));
#27037=CARTESIAN_POINT('Ctrl Pts',(-0.46564546202603,-1.,-1.9428979419619));
#27038=CARTESIAN_POINT('Ctrl Pts',(-0.46564546202603,1.,-1.9428979419619));
#27039=CARTESIAN_POINT('Ctrl Pts',(-0.468997482913135,-1.,-1.94794381136514));
#27040=CARTESIAN_POINT('Ctrl Pts',(-0.468997482913135,1.,-1.94794381136514));
#27041=CARTESIAN_POINT('Ctrl Pts',(-0.472397672264072,-1.,-1.95296148278133));
#27042=CARTESIAN_POINT('Ctrl Pts',(-0.472397672264072,1.,-1.95296148278133));
#27043=CARTESIAN_POINT('Ctrl Pts',(-0.475848034683176,-1.,-1.95796111148177));
#27044=CARTESIAN_POINT('Ctrl Pts',(-0.475848034683176,1.,-1.95796111148177));
#27045=CARTESIAN_POINT('Ctrl Pts',(-0.479349583074855,-1.,-1.96294933055943));
#27046=CARTESIAN_POINT('Ctrl Pts',(-0.479349583074855,1.,-1.96294933055943));
#27047=CARTESIAN_POINT('Ctrl Pts',(-0.482901662120691,-1.,-1.96792703422362));
#27048=CARTESIAN_POINT('Ctrl Pts',(-0.482901662120691,1.,-1.96792703422362));
#27049=CARTESIAN_POINT('Ctrl Pts',(-0.486502692907659,-1.,-1.97289186263272));
#27050=CARTESIAN_POINT('Ctrl Pts',(-0.486502692907659,1.,-1.97289186263272));
#27051=CARTESIAN_POINT('Ctrl Pts',(-0.490150627860952,-1.,-1.97783973019229));
#27052=CARTESIAN_POINT('Ctrl Pts',(-0.490150627860952,1.,-1.97783973019229));
#27053=CARTESIAN_POINT('Ctrl Pts',(-0.493843476541495,-1.,-1.98276658761821));
#27054=CARTESIAN_POINT('Ctrl Pts',(-0.493843476541495,1.,-1.98276658761821));
#27055=CARTESIAN_POINT('Ctrl Pts',(-0.497579909545574,-1.,-1.98767044752932));
#27056=CARTESIAN_POINT('Ctrl Pts',(-0.497579909545574,1.,-1.98767044752932));
#27057=CARTESIAN_POINT('Ctrl Pts',(-0.501359287727146,-1.,-1.99255149126155));
#27058=CARTESIAN_POINT('Ctrl Pts',(-0.501359287727146,1.,-1.99255149126155));
#27059=CARTESIAN_POINT('Ctrl Pts',(-0.505181361323026,-1.,-1.99741107463572));
#27060=CARTESIAN_POINT('Ctrl Pts',(-0.505181361323026,1.,-1.99741107463572));
#27061=CARTESIAN_POINT('Ctrl Pts',(-0.509046069886157,-1.,-2.00225107134734));
#27062=CARTESIAN_POINT('Ctrl Pts',(-0.509046069886157,1.,-2.00225107134734));
#27063=CARTESIAN_POINT('Ctrl Pts',(-0.512953306961792,-1.,-2.00707309946949));
#27064=CARTESIAN_POINT('Ctrl Pts',(-0.512953306961792,1.,-2.00707309946949));
#27065=CARTESIAN_POINT('Ctrl Pts',(-0.516902681728687,-1.,-2.01187773939242));
#27066=CARTESIAN_POINT('Ctrl Pts',(-0.516902681728687,1.,-2.01187773939242));
#27067=CARTESIAN_POINT('Ctrl Pts',(-0.52089359039937,-1.,-2.01666477917286));
#27068=CARTESIAN_POINT('Ctrl Pts',(-0.52089359039937,1.,-2.01666477917286));
#27069=CARTESIAN_POINT('Ctrl Pts',(-0.524925318333476,-1.,-2.02143356304698));
#27070=CARTESIAN_POINT('Ctrl Pts',(-0.524925318333476,1.,-2.02143356304698));
#27071=CARTESIAN_POINT('Ctrl Pts',(-0.528997127241914,-1.,-2.0261832908329));
#27072=CARTESIAN_POINT('Ctrl Pts',(-0.528997127241914,1.,-2.0261832908329));
#27073=CARTESIAN_POINT('Ctrl Pts',(-0.533108355132977,-1.,-2.03091336214426));
#27074=CARTESIAN_POINT('Ctrl Pts',(-0.533108355132977,1.,-2.03091336214426));
#27075=CARTESIAN_POINT('Ctrl Pts',(-0.537258489833262,-1.,-2.03562362954037));
#27076=CARTESIAN_POINT('Ctrl Pts',(-0.537258489833262,1.,-2.03562362954037));
#27077=CARTESIAN_POINT('Ctrl Pts',(-0.541447120615659,-1.,-2.04031422690527));
#27078=CARTESIAN_POINT('Ctrl Pts',(-0.541447120615659,1.,-2.04031422690527));
#27079=CARTESIAN_POINT('Ctrl Pts',(-0.54567390381743,-1.,-2.04498544714588));
#27080=CARTESIAN_POINT('Ctrl Pts',(-0.54567390381743,1.,-2.04498544714588));
#27081=CARTESIAN_POINT('Ctrl Pts',(-0.549938525150295,-1.,-2.04963761077958));
#27082=CARTESIAN_POINT('Ctrl Pts',(-0.549938525150295,1.,-2.04963761077958));
#27083=CARTESIAN_POINT('Ctrl Pts',(-0.554240657463906,-1.,-2.05427091604413));
#27084=CARTESIAN_POINT('Ctrl Pts',(-0.554240657463906,1.,-2.05427091604413));
#27085=CARTESIAN_POINT('Ctrl Pts',(-0.558579940185151,-1.,-2.05888537756462));
#27086=CARTESIAN_POINT('Ctrl Pts',(-0.558579940185151,1.,-2.05888537756462));
#27087=CARTESIAN_POINT('Ctrl Pts',(-0.562955993082261,-1.,-2.06348090160589));
#27088=CARTESIAN_POINT('Ctrl Pts',(-0.562955993082261,1.,-2.06348090160589));
#27089=CARTESIAN_POINT('Ctrl Pts',(-0.567368421181087,-1.,-2.06805732997334));
#27090=CARTESIAN_POINT('Ctrl Pts',(-0.567368421181087,1.,-2.06805732997334));
#27091=CARTESIAN_POINT('Ctrl Pts',(-0.571816823242603,-1.,-2.07261449292824));
#27092=CARTESIAN_POINT('Ctrl Pts',(-0.571816823242603,1.,-2.07261449292824));
#27093=CARTESIAN_POINT('Ctrl Pts',(-0.576300797416844,-1.,-2.07715226767559));
#27094=CARTESIAN_POINT('Ctrl Pts',(-0.576300797416844,1.,-2.07715226767559));
#27095=CARTESIAN_POINT('Ctrl Pts',(-0.580819952108063,-1.,-2.08167059018418));
#27096=CARTESIAN_POINT('Ctrl Pts',(-0.580819952108063,1.,-2.08167059018418));
#27097=CARTESIAN_POINT('Ctrl Pts',(-0.585373918991617,-1.,-2.08616943727951));
#27098=CARTESIAN_POINT('Ctrl Pts',(-0.585373918991617,1.,-2.08616943727951));
#27099=CARTESIAN_POINT('Ctrl Pts',(-0.589962365403406,-1.,-2.09064881812129));
#27100=CARTESIAN_POINT('Ctrl Pts',(-0.589962365403406,1.,-2.09064881812129));
#27101=CARTESIAN_POINT('Ctrl Pts',(-0.594585006052162,-1.,-2.0951087622027));
#27102=CARTESIAN_POINT('Ctrl Pts',(-0.594585006052162,1.,-2.0951087622027));
#27103=CARTESIAN_POINT('Ctrl Pts',(-0.599241616420533,-1.,-2.0995493086477));
#27104=CARTESIAN_POINT('Ctrl Pts',(-0.599241616420533,1.,-2.0995493086477));
#27105=CARTESIAN_POINT('Ctrl Pts',(-0.60393203073603,-1.,-2.10397049886949));
#27106=CARTESIAN_POINT('Ctrl Pts',(-0.60393203073603,1.,-2.10397049886949));
#27107=CARTESIAN_POINT('Ctrl Pts',(-0.607711315454876,-1.,-2.1074919961518));
#27108=CARTESIAN_POINT('Ctrl Pts',(-0.607711315454876,1.,-2.1074919961518));
#27109=CARTESIAN_POINT('Ctrl Pts',(-0.610560911689899,-1.,-2.11012443807238));
#27110=CARTESIAN_POINT('Ctrl Pts',(-0.610560911689899,1.,-2.11012443807238));
#27111=CARTESIAN_POINT('Ctrl Pts',(-0.6124673655618,-1.,-2.11187554259986));
#27112=CARTESIAN_POINT('Ctrl Pts',(-0.6124673655618,1.,-2.11187554259986));
#27113=CARTESIAN_POINT('Ctrl Pts',(-0.61342227326009,-1.,-2.11275013067528));
#27114=CARTESIAN_POINT('Ctrl Pts',(-0.61342227326009,1.,-2.11275013067528));
#27115=CARTESIAN_POINT('',(-0.383122945602004,1.,-1.7075470150345));
#27116=CARTESIAN_POINT('Ctrl Pts',(-0.383122945602004,1.,-1.7075470150345));
#27117=CARTESIAN_POINT('Ctrl Pts',(-0.384119047315542,1.,-1.71231062891958));
#27118=CARTESIAN_POINT('Ctrl Pts',(-0.38607079032701,1.,-1.72162022246158));
#27119=CARTESIAN_POINT('Ctrl Pts',(-0.388877023509191,1.,-1.7349317097561));
#27120=CARTESIAN_POINT('Ctrl Pts',(-0.392375812294307,1.,-1.75137405313962));
#27121=CARTESIAN_POINT('Ctrl Pts',(-0.39634619612042,1.,-1.7697556004756));
#27122=CARTESIAN_POINT('Ctrl Pts',(-0.39991940378308,1.,-1.78598826347533));
#27123=CARTESIAN_POINT('Ctrl Pts',(-0.403107976170441,1.,-1.80012077176221));
#27124=CARTESIAN_POINT('Ctrl Pts',(-0.405933518411838,1.,-1.81223801813988));
#27125=CARTESIAN_POINT('Ctrl Pts',(-0.408428948108533,1.,-1.8224702267854));
#27126=CARTESIAN_POINT('Ctrl Pts',(-0.410641256301675,1.,-1.83100408895216));
#27127=CARTESIAN_POINT('Ctrl Pts',(-0.412633125322162,1.,-1.83808953475839));
#27128=CARTESIAN_POINT('Ctrl Pts',(-0.41448743825434,1.,-1.8440575707371));
#27129=CARTESIAN_POINT('Ctrl Pts',(-0.416300022038864,1.,-1.84929312929882));
#27130=CARTESIAN_POINT('Ctrl Pts',(-0.418164129143534,1.,-1.85417632856234));
#27131=CARTESIAN_POINT('Ctrl Pts',(-0.420157287975619,1.,-1.85903281096686));
#27132=CARTESIAN_POINT('Ctrl Pts',(-0.422327307418275,1.,-1.86408083334028));
#27133=CARTESIAN_POINT('Ctrl Pts',(-0.424678177291359,1.,-1.86937803944323));
#27134=CARTESIAN_POINT('Ctrl Pts',(-0.427183828519102,1.,-1.87486989291484));
#27135=CARTESIAN_POINT('Ctrl Pts',(-0.429803062482344,1.,-1.88044229001832));
#27136=CARTESIAN_POINT('Ctrl Pts',(-0.432493038548748,1.,-1.88596913666793));
#27137=CARTESIAN_POINT('Ctrl Pts',(-0.435225660963383,1.,-1.89136993975504));
#27138=CARTESIAN_POINT('Ctrl Pts',(-0.437995003948244,1.,-1.89663648956466));
#27139=CARTESIAN_POINT('Ctrl Pts',(-0.440807833704038,1.,-1.90180124389086));
#27140=CARTESIAN_POINT('Ctrl Pts',(-0.443677556849151,1.,-1.90691756144898));
#27141=CARTESIAN_POINT('Ctrl Pts',(-0.446617343485711,1.,-1.9120369998112));
#27142=CARTESIAN_POINT('Ctrl Pts',(-0.449632260106662,1.,-1.91718342555755));
#27143=CARTESIAN_POINT('Ctrl Pts',(-0.452719478359432,1.,-1.92235380648502));
#27144=CARTESIAN_POINT('Ctrl Pts',(-0.455872005174371,1.,-1.92753067150476));
#27145=CARTESIAN_POINT('Ctrl Pts',(-0.459081234547926,1.,-1.93269066517934));
#27146=CARTESIAN_POINT('Ctrl Pts',(-0.462340031009056,1.,-1.93781486640821));
#27147=CARTESIAN_POINT('Ctrl Pts',(-0.46564546202603,1.,-1.9428979419619));
#27148=CARTESIAN_POINT('Ctrl Pts',(-0.468997482913135,1.,-1.94794381136514));
#27149=CARTESIAN_POINT('Ctrl Pts',(-0.472397672264072,1.,-1.95296148278133));
#27150=CARTESIAN_POINT('Ctrl Pts',(-0.475848034683176,1.,-1.95796111148177));
#27151=CARTESIAN_POINT('Ctrl Pts',(-0.479349583074855,1.,-1.96294933055943));
#27152=CARTESIAN_POINT('Ctrl Pts',(-0.482901662120691,1.,-1.96792703422362));
#27153=CARTESIAN_POINT('Ctrl Pts',(-0.486502692907659,1.,-1.97289186263272));
#27154=CARTESIAN_POINT('Ctrl Pts',(-0.490150627860952,1.,-1.97783973019229));
#27155=CARTESIAN_POINT('Ctrl Pts',(-0.493843476541495,1.,-1.98276658761821));
#27156=CARTESIAN_POINT('Ctrl Pts',(-0.497579909545574,1.,-1.98767044752932));
#27157=CARTESIAN_POINT('Ctrl Pts',(-0.501359287727146,1.,-1.99255149126155));
#27158=CARTESIAN_POINT('Ctrl Pts',(-0.505181361323026,1.,-1.99741107463572));
#27159=CARTESIAN_POINT('Ctrl Pts',(-0.509046069886157,1.,-2.00225107134734));
#27160=CARTESIAN_POINT('Ctrl Pts',(-0.512953306961792,1.,-2.00707309946949));
#27161=CARTESIAN_POINT('Ctrl Pts',(-0.516902681728687,1.,-2.01187773939242));
#27162=CARTESIAN_POINT('Ctrl Pts',(-0.52089359039937,1.,-2.01666477917286));
#27163=CARTESIAN_POINT('Ctrl Pts',(-0.524925318333476,1.,-2.02143356304698));
#27164=CARTESIAN_POINT('Ctrl Pts',(-0.528997127241914,1.,-2.0261832908329));
#27165=CARTESIAN_POINT('Ctrl Pts',(-0.533108355132977,1.,-2.03091336214426));
#27166=CARTESIAN_POINT('Ctrl Pts',(-0.537258489833262,1.,-2.03562362954037));
#27167=CARTESIAN_POINT('Ctrl Pts',(-0.541447120615659,1.,-2.04031422690527));
#27168=CARTESIAN_POINT('Ctrl Pts',(-0.54567390381743,1.,-2.04498544714588));
#27169=CARTESIAN_POINT('Ctrl Pts',(-0.549938525150295,1.,-2.04963761077958));
#27170=CARTESIAN_POINT('Ctrl Pts',(-0.554240657463906,1.,-2.05427091604413));
#27171=CARTESIAN_POINT('Ctrl Pts',(-0.558579940185151,1.,-2.05888537756462));
#27172=CARTESIAN_POINT('Ctrl Pts',(-0.562955993082261,1.,-2.06348090160589));
#27173=CARTESIAN_POINT('Ctrl Pts',(-0.567368421181087,1.,-2.06805732997334));
#27174=CARTESIAN_POINT('Ctrl Pts',(-0.571816823242603,1.,-2.07261449292824));
#27175=CARTESIAN_POINT('Ctrl Pts',(-0.576300797416844,1.,-2.07715226767559));
#27176=CARTESIAN_POINT('Ctrl Pts',(-0.580819952108063,1.,-2.08167059018418));
#27177=CARTESIAN_POINT('Ctrl Pts',(-0.585373918991617,1.,-2.08616943727951));
#27178=CARTESIAN_POINT('Ctrl Pts',(-0.589962365403406,1.,-2.09064881812129));
#27179=CARTESIAN_POINT('Ctrl Pts',(-0.594585006052162,1.,-2.0951087622027));
#27180=CARTESIAN_POINT('Ctrl Pts',(-0.599241616420533,1.,-2.0995493086477));
#27181=CARTESIAN_POINT('Ctrl Pts',(-0.60393203073603,1.,-2.10397049886949));
#27182=CARTESIAN_POINT('Ctrl Pts',(-0.607711315454876,1.,-2.1074919961518));
#27183=CARTESIAN_POINT('Ctrl Pts',(-0.610560911689899,1.,-2.11012443807238));
#27184=CARTESIAN_POINT('Ctrl Pts',(-0.6124673655618,1.,-2.11187554259986));
#27185=CARTESIAN_POINT('Ctrl Pts',(-0.61342227326009,1.,-2.11275013067528));
#27186=CARTESIAN_POINT('',(-0.383122945602003,0.,-1.7075470150345));
#27187=CARTESIAN_POINT('Origin',(0.,0.,0.));
#27188=CARTESIAN_POINT('',(-0.163289472382896,1.,-1.74236521665491));
#27189=CARTESIAN_POINT('Origin',(0.,1.,0.));
#27190=CARTESIAN_POINT('',(-0.163289472382896,0.,-1.74236521665491));
#27191=CARTESIAN_POINT('Ctrl Pts',(-0.0694764450219581,-1.,-2.19890268624765));
#27192=CARTESIAN_POINT('Ctrl Pts',(-0.0694764450219581,1.,-2.19890268624765));
#27193=CARTESIAN_POINT('Ctrl Pts',(-0.070114353632549,-1.,-2.19777582085423));
#27194=CARTESIAN_POINT('Ctrl Pts',(-0.070114353632549,1.,-2.19777582085423));
#27195=CARTESIAN_POINT('Ctrl Pts',(-0.0713863779526154,-1.,-2.19552129484002));
#27196=CARTESIAN_POINT('Ctrl Pts',(-0.0713863779526154,1.,-2.19552129484002));
#27197=CARTESIAN_POINT('Ctrl Pts',(-0.0732830357306725,-1.,-2.19213712013662));
#27198=CARTESIAN_POINT('Ctrl Pts',(-0.0732830357306725,1.,-2.19213712013662));
#27199=CARTESIAN_POINT('Ctrl Pts',(-0.0757891465836148,-1.,-2.1876201139953));
#27200=CARTESIAN_POINT('Ctrl Pts',(-0.0757891465836148,1.,-2.1876201139953));
#27201=CARTESIAN_POINT('Ctrl Pts',(-0.0788837727685243,-1.,-2.18196589448887));
#27202=CARTESIAN_POINT('Ctrl Pts',(-0.0788837727685243,1.,-2.18196589448887));
#27203=CARTESIAN_POINT('Ctrl Pts',(-0.0819402680872765,-1.,-2.176303712113));
#27204=CARTESIAN_POINT('Ctrl Pts',(-0.0819402680872765,1.,-2.176303712113));
#27205=CARTESIAN_POINT('Ctrl Pts',(-0.0849584620835372,-1.,-2.17063357870952));
#27206=CARTESIAN_POINT('Ctrl Pts',(-0.0849584620835372,1.,-2.17063357870952));
#27207=CARTESIAN_POINT('Ctrl Pts',(-0.0879381291386923,-1.,-2.16495552645014));
#27208=CARTESIAN_POINT('Ctrl Pts',(-0.0879381291386923,1.,-2.16495552645014));
#27209=CARTESIAN_POINT('Ctrl Pts',(-0.0908789888107265,-1.,-2.15926961544516));
#27210=CARTESIAN_POINT('Ctrl Pts',(-0.0908789888107265,1.,-2.15926961544516));
#27211=CARTESIAN_POINT('Ctrl Pts',(-0.0937807218867643,-1.,-2.1535759397817));
#27212=CARTESIAN_POINT('Ctrl Pts',(-0.0937807218867643,1.,-2.1535759397817));
#27213=CARTESIAN_POINT('Ctrl Pts',(-0.0966429852305459,-1.,-2.14787463531795));
#27214=CARTESIAN_POINT('Ctrl Pts',(-0.0966429852305459,1.,-2.14787463531795));
#27215=CARTESIAN_POINT('Ctrl Pts',(-0.0994654261990915,-1.,-2.14216588396025));
#27216=CARTESIAN_POINT('Ctrl Pts',(-0.0994654261990915,1.,-2.14216588396025));
#27217=CARTESIAN_POINT('Ctrl Pts',(-0.1022477005561,-1.,-2.13644992667165));
#27218=CARTESIAN_POINT('Ctrl Pts',(-0.1022477005561,1.,-2.13644992667165));
#27219=CARTESIAN_POINT('Ctrl Pts',(-0.104989479152739,-1.,-2.13072704887293));
#27220=CARTESIAN_POINT('Ctrl Pts',(-0.104989479152739,1.,-2.13072704887293));
#27221=CARTESIAN_POINT('Ctrl Pts',(-0.10769043523109,-1.,-2.12499752307));
#27222=CARTESIAN_POINT('Ctrl Pts',(-0.10769043523109,1.,-2.12499752307));
#27223=CARTESIAN_POINT('Ctrl Pts',(-0.110350236135025,-1.,-2.11926155590865));
#27224=CARTESIAN_POINT('Ctrl Pts',(-0.110350236135025,1.,-2.11926155590865));
#27225=CARTESIAN_POINT('Ctrl Pts',(-0.112968534419737,-1.,-2.11351924490306));
#27226=CARTESIAN_POINT('Ctrl Pts',(-0.112968534419737,1.,-2.11351924490306));
#27227=CARTESIAN_POINT('Ctrl Pts',(-0.115544957687926,-1.,-2.10777050261309));
#27228=CARTESIAN_POINT('Ctrl Pts',(-0.115544957687926,1.,-2.10777050261309));
#27229=CARTESIAN_POINT('Ctrl Pts',(-0.118079107988355,-1.,-2.102015121329));
#27230=CARTESIAN_POINT('Ctrl Pts',(-0.118079107988355,1.,-2.102015121329));
#27231=CARTESIAN_POINT('Ctrl Pts',(-0.120570567965122,-1.,-2.0962529286773));
#27232=CARTESIAN_POINT('Ctrl Pts',(-0.120570567965122,1.,-2.0962529286773));
#27233=CARTESIAN_POINT('Ctrl Pts',(-0.123018905621083,-1.,-2.09048392424825));
#27234=CARTESIAN_POINT('Ctrl Pts',(-0.123018905621083,1.,-2.09048392424825));
#27235=CARTESIAN_POINT('Ctrl Pts',(-0.125423679412061,-1.,-2.08470840653643));
#27236=CARTESIAN_POINT('Ctrl Pts',(-0.125423679412061,1.,-2.08470840653643));
#27237=CARTESIAN_POINT('Ctrl Pts',(-0.12778444527612,-1.,-2.07892715110987));
#27238=CARTESIAN_POINT('Ctrl Pts',(-0.12778444527612,1.,-2.07892715110987));
#27239=CARTESIAN_POINT('Ctrl Pts',(-0.130100748328403,-1.,-2.07314114713063));
#27240=CARTESIAN_POINT('Ctrl Pts',(-0.130100748328403,1.,-2.07314114713063));
#27241=CARTESIAN_POINT('Ctrl Pts',(-0.13237211154771,-1.,-2.06735123910326));
#27242=CARTESIAN_POINT('Ctrl Pts',(-0.13237211154771,1.,-2.06735123910326));
#27243=CARTESIAN_POINT('Ctrl Pts',(-0.134598026192106,-1.,-2.06155781517842));
#27244=CARTESIAN_POINT('Ctrl Pts',(-0.134598026192106,1.,-2.06155781517842));
#27245=CARTESIAN_POINT('Ctrl Pts',(-0.136777941218044,-1.,-2.05576044414264));
#27246=CARTESIAN_POINT('Ctrl Pts',(-0.136777941218044,1.,-2.05576044414264));
#27247=CARTESIAN_POINT('Ctrl Pts',(-0.138911255368966,-1.,-2.04995762001328));
#27248=CARTESIAN_POINT('Ctrl Pts',(-0.138911255368966,1.,-2.04995762001328));
#27249=CARTESIAN_POINT('Ctrl Pts',(-0.140997332152546,-1.,-2.04414757947916));
#27250=CARTESIAN_POINT('Ctrl Pts',(-0.140997332152546,1.,-2.04414757947916));
#27251=CARTESIAN_POINT('Ctrl Pts',(-0.143035515058209,-1.,-2.03832911025912));
#27252=CARTESIAN_POINT('Ctrl Pts',(-0.143035515058209,1.,-2.03832911025912));
#27253=CARTESIAN_POINT('Ctrl Pts',(-0.145025140186057,-1.,-2.03250223739942));
#27254=CARTESIAN_POINT('Ctrl Pts',(-0.145025140186057,1.,-2.03250223739942));
#27255=CARTESIAN_POINT('Ctrl Pts',(-0.146965557332583,-1.,-2.02666926182017));
#27256=CARTESIAN_POINT('Ctrl Pts',(-0.146965557332583,1.,-2.02666926182017));
#27257=CARTESIAN_POINT('Ctrl Pts',(-0.148856124775337,-1.,-2.02083464969894));
#27258=CARTESIAN_POINT('Ctrl Pts',(-0.148856124775337,1.,-2.02083464969894));
#27259=CARTESIAN_POINT('Ctrl Pts',(-0.150696157673078,-1.,-2.01500291940238));
#27260=CARTESIAN_POINT('Ctrl Pts',(-0.150696157673078,1.,-2.01500291940238));
#27261=CARTESIAN_POINT('Ctrl Pts',(-0.15248488362145,-1.,-2.00917680318424));
#27262=CARTESIAN_POINT('Ctrl Pts',(-0.15248488362145,1.,-2.00917680318424));
#27263=CARTESIAN_POINT('Ctrl Pts',(-0.154221403049722,-1.,-2.00335565310543));
#27264=CARTESIAN_POINT('Ctrl Pts',(-0.154221403049722,1.,-2.00335565310543));
#27265=CARTESIAN_POINT('Ctrl Pts',(-0.155904629548783,-1.,-1.99753284771497));
#27266=CARTESIAN_POINT('Ctrl Pts',(-0.155904629548783,1.,-1.99753284771497));
#27267=CARTESIAN_POINT('Ctrl Pts',(-0.157533331459227,-1.,-1.99169810931908));
#27268=CARTESIAN_POINT('Ctrl Pts',(-0.157533331459227,1.,-1.99169810931908));
#27269=CARTESIAN_POINT('Ctrl Pts',(-0.159106226437299,-1.,-1.98584238283292));
#27270=CARTESIAN_POINT('Ctrl Pts',(-0.159106226437299,1.,-1.98584238283292));
#27271=CARTESIAN_POINT('Ctrl Pts',(-0.160622060784611,-1.,-1.97996195437559));
#27272=CARTESIAN_POINT('Ctrl Pts',(-0.160622060784611,1.,-1.97996195437559));
#27273=CARTESIAN_POINT('Ctrl Pts',(-0.162079693556289,-1.,-1.97406280235188));
#27274=CARTESIAN_POINT('Ctrl Pts',(-0.162079693556289,1.,-1.97406280235188));
#27275=CARTESIAN_POINT('Ctrl Pts',(-0.163478185457734,-1.,-1.96816512677967));
#27276=CARTESIAN_POINT('Ctrl Pts',(-0.163478185457734,1.,-1.96816512677967));
#27277=CARTESIAN_POINT('Ctrl Pts',(-0.164816568920269,-1.,-1.96229379940136));
#27278=CARTESIAN_POINT('Ctrl Pts',(-0.164816568920269,1.,-1.96229379940136));
#27279=CARTESIAN_POINT('Ctrl Pts',(-0.166093592002812,-1.,-1.9564675971873));
#27280=CARTESIAN_POINT('Ctrl Pts',(-0.166093592002812,1.,-1.9564675971873));
#27281=CARTESIAN_POINT('Ctrl Pts',(-0.167307501784475,-1.,-1.95069027794294));
#27282=CARTESIAN_POINT('Ctrl Pts',(-0.167307501784475,1.,-1.95069027794294));
#27283=CARTESIAN_POINT('Ctrl Pts',(-0.168455741607556,-1.,-1.94493757756931));
#27284=CARTESIAN_POINT('Ctrl Pts',(-0.168455741607556,1.,-1.94493757756931));
#27285=CARTESIAN_POINT('Ctrl Pts',(-0.169534904817491,-1.,-1.93915639211581));
#27286=CARTESIAN_POINT('Ctrl Pts',(-0.169534904817491,1.,-1.93915639211581));
#27287=CARTESIAN_POINT('Ctrl Pts',(-0.170541253116202,-1.,-1.93329183155539));
#27288=CARTESIAN_POINT('Ctrl Pts',(-0.170541253116202,1.,-1.93329183155539));
#27289=CARTESIAN_POINT('Ctrl Pts',(-0.171471191532988,-1.,-1.92731093582036));
#27290=CARTESIAN_POINT('Ctrl Pts',(-0.171471191532988,1.,-1.92731093582036));
#27291=CARTESIAN_POINT('Ctrl Pts',(-0.172321621259514,-1.,-1.9212233439798));
#27292=CARTESIAN_POINT('Ctrl Pts',(-0.172321621259514,1.,-1.9212233439798));
#27293=CARTESIAN_POINT('Ctrl Pts',(-0.173090695383496,-1.,-1.91511429159527));
#27294=CARTESIAN_POINT('Ctrl Pts',(-0.173090695383496,1.,-1.91511429159527));
#27295=CARTESIAN_POINT('Ctrl Pts',(-0.173776635257817,-1.,-1.90911693975267));
#27296=CARTESIAN_POINT('Ctrl Pts',(-0.173776635257817,1.,-1.90911693975267));
#27297=CARTESIAN_POINT('Ctrl Pts',(-0.174375518661085,-1.,-1.90335253862834));
#27298=CARTESIAN_POINT('Ctrl Pts',(-0.174375518661085,1.,-1.90335253862834));
#27299=CARTESIAN_POINT('Ctrl Pts',(-0.174879405091263,-1.,-1.89788101117132));
#27300=CARTESIAN_POINT('Ctrl Pts',(-0.174879405091263,1.,-1.89788101117132));
#27301=CARTESIAN_POINT('Ctrl Pts',(-0.175274276190844,-1.,-1.892646301985));
#27302=CARTESIAN_POINT('Ctrl Pts',(-0.175274276190844,1.,-1.892646301985));
#27303=CARTESIAN_POINT('Ctrl Pts',(-0.175538155840648,-1.,-1.88742606273259));
#27304=CARTESIAN_POINT('Ctrl Pts',(-0.175538155840648,1.,-1.88742606273259));
#27305=CARTESIAN_POINT('Ctrl Pts',(-0.175644148889699,-1.,-1.88188663145367));
#27306=CARTESIAN_POINT('Ctrl Pts',(-0.175644148889699,1.,-1.88188663145367));
#27307=CARTESIAN_POINT('Ctrl Pts',(-0.175563480746485,-1.,-1.87563767773588));
#27308=CARTESIAN_POINT('Ctrl Pts',(-0.175563480746485,1.,-1.87563767773588));
#27309=CARTESIAN_POINT('Ctrl Pts',(-0.175268337590758,-1.,-1.86828349694799));
#27310=CARTESIAN_POINT('Ctrl Pts',(-0.175268337590758,1.,-1.86828349694799));
#27311=CARTESIAN_POINT('Ctrl Pts',(-0.17473525927603,-1.,-1.85948367088837));
#27312=CARTESIAN_POINT('Ctrl Pts',(-0.17473525927603,1.,-1.85948367088837));
#27313=CARTESIAN_POINT('Ctrl Pts',(-0.173946627587731,-1.,-1.8489811319852));
#27314=CARTESIAN_POINT('Ctrl Pts',(-0.173946627587731,1.,-1.8489811319852));
#27315=CARTESIAN_POINT('Ctrl Pts',(-0.1728894428919,-1.,-1.83658380527692));
#27316=CARTESIAN_POINT('Ctrl Pts',(-0.1728894428919,1.,-1.83658380527692));
#27317=CARTESIAN_POINT('Ctrl Pts',(-0.171554770204119,-1.,-1.82215766811545));
#27318=CARTESIAN_POINT('Ctrl Pts',(-0.171554770204119,1.,-1.82215766811545));
#27319=CARTESIAN_POINT('Ctrl Pts',(-0.169936923904608,-1.,-1.80561530629706));
#27320=CARTESIAN_POINT('Ctrl Pts',(-0.169936923904608,1.,-1.80561530629706));
#27321=CARTESIAN_POINT('Ctrl Pts',(-0.168032772805197,-1.,-1.7869064998507));
#27322=CARTESIAN_POINT('Ctrl Pts',(-0.168032772805197,1.,-1.7869064998507));
#27323=CARTESIAN_POINT('Ctrl Pts',(-0.1662793551464,-1.,-1.77018771684844));
#27324=CARTESIAN_POINT('Ctrl Pts',(-0.1662793551464,1.,-1.77018771684844));
#27325=CARTESIAN_POINT('Ctrl Pts',(-0.164834765707158,-1.,-1.75666056638427));
#27326=CARTESIAN_POINT('Ctrl Pts',(-0.164834765707158,1.,-1.75666056638427));
#27327=CARTESIAN_POINT('Ctrl Pts',(-0.163814161002002,-1.,-1.7472034950333));
#27328=CARTESIAN_POINT('Ctrl Pts',(-0.163814161002002,1.,-1.7472034950333));
#27329=CARTESIAN_POINT('Ctrl Pts',(-0.163289472382896,-1.,-1.74236521665491));
#27330=CARTESIAN_POINT('Ctrl Pts',(-0.163289472382896,1.,-1.74236521665491));
#27331=CARTESIAN_POINT('',(-0.0694764450219581,1.,-2.19890268624765));
#27332=CARTESIAN_POINT('Ctrl Pts',(-0.0694764450219581,1.,-2.19890268624765));
#27333=CARTESIAN_POINT('Ctrl Pts',(-0.070114353632549,1.,-2.19777582085423));
#27334=CARTESIAN_POINT('Ctrl Pts',(-0.0713863779526154,1.,-2.19552129484002));
#27335=CARTESIAN_POINT('Ctrl Pts',(-0.0732830357306725,1.,-2.19213712013662));
#27336=CARTESIAN_POINT('Ctrl Pts',(-0.0757891465836148,1.,-2.1876201139953));
#27337=CARTESIAN_POINT('Ctrl Pts',(-0.0788837727685243,1.,-2.18196589448887));
#27338=CARTESIAN_POINT('Ctrl Pts',(-0.0819402680872765,1.,-2.176303712113));
#27339=CARTESIAN_POINT('Ctrl Pts',(-0.0849584620835372,1.,-2.17063357870952));
#27340=CARTESIAN_POINT('Ctrl Pts',(-0.0879381291386923,1.,-2.16495552645014));
#27341=CARTESIAN_POINT('Ctrl Pts',(-0.0908789888107265,1.,-2.15926961544516));
#27342=CARTESIAN_POINT('Ctrl Pts',(-0.0937807218867643,1.,-2.1535759397817));
#27343=CARTESIAN_POINT('Ctrl Pts',(-0.0966429852305459,1.,-2.14787463531795));
#27344=CARTESIAN_POINT('Ctrl Pts',(-0.0994654261990915,1.,-2.14216588396025));
#27345=CARTESIAN_POINT('Ctrl Pts',(-0.1022477005561,1.,-2.13644992667165));
#27346=CARTESIAN_POINT('Ctrl Pts',(-0.104989479152739,1.,-2.13072704887293));
#27347=CARTESIAN_POINT('Ctrl Pts',(-0.10769043523109,1.,-2.12499752307));
#27348=CARTESIAN_POINT('Ctrl Pts',(-0.110350236135025,1.,-2.11926155590865));
#27349=CARTESIAN_POINT('Ctrl Pts',(-0.112968534419737,1.,-2.11351924490306));
#27350=CARTESIAN_POINT('Ctrl Pts',(-0.115544957687926,1.,-2.10777050261309));
#27351=CARTESIAN_POINT('Ctrl Pts',(-0.118079107988355,1.,-2.102015121329));
#27352=CARTESIAN_POINT('Ctrl Pts',(-0.120570567965122,1.,-2.0962529286773));
#27353=CARTESIAN_POINT('Ctrl Pts',(-0.123018905621083,1.,-2.09048392424825));
#27354=CARTESIAN_POINT('Ctrl Pts',(-0.125423679412061,1.,-2.08470840653643));
#27355=CARTESIAN_POINT('Ctrl Pts',(-0.12778444527612,1.,-2.07892715110987));
#27356=CARTESIAN_POINT('Ctrl Pts',(-0.130100748328403,1.,-2.07314114713063));
#27357=CARTESIAN_POINT('Ctrl Pts',(-0.13237211154771,1.,-2.06735123910326));
#27358=CARTESIAN_POINT('Ctrl Pts',(-0.134598026192106,1.,-2.06155781517842));
#27359=CARTESIAN_POINT('Ctrl Pts',(-0.136777941218044,1.,-2.05576044414264));
#27360=CARTESIAN_POINT('Ctrl Pts',(-0.138911255368966,1.,-2.04995762001328));
#27361=CARTESIAN_POINT('Ctrl Pts',(-0.140997332152546,1.,-2.04414757947916));
#27362=CARTESIAN_POINT('Ctrl Pts',(-0.143035515058209,1.,-2.03832911025912));
#27363=CARTESIAN_POINT('Ctrl Pts',(-0.145025140186057,1.,-2.03250223739942));
#27364=CARTESIAN_POINT('Ctrl Pts',(-0.146965557332583,1.,-2.02666926182017));
#27365=CARTESIAN_POINT('Ctrl Pts',(-0.148856124775337,1.,-2.02083464969894));
#27366=CARTESIAN_POINT('Ctrl Pts',(-0.150696157673078,1.,-2.01500291940238));
#27367=CARTESIAN_POINT('Ctrl Pts',(-0.15248488362145,1.,-2.00917680318424));
#27368=CARTESIAN_POINT('Ctrl Pts',(-0.154221403049722,1.,-2.00335565310543));
#27369=CARTESIAN_POINT('Ctrl Pts',(-0.155904629548783,1.,-1.99753284771497));
#27370=CARTESIAN_POINT('Ctrl Pts',(-0.157533331459227,1.,-1.99169810931908));
#27371=CARTESIAN_POINT('Ctrl Pts',(-0.159106226437299,1.,-1.98584238283292));
#27372=CARTESIAN_POINT('Ctrl Pts',(-0.160622060784611,1.,-1.97996195437559));
#27373=CARTESIAN_POINT('Ctrl Pts',(-0.162079693556289,1.,-1.97406280235188));
#27374=CARTESIAN_POINT('Ctrl Pts',(-0.163478185457734,1.,-1.96816512677967));
#27375=CARTESIAN_POINT('Ctrl Pts',(-0.164816568920269,1.,-1.96229379940136));
#27376=CARTESIAN_POINT('Ctrl Pts',(-0.166093592002812,1.,-1.9564675971873));
#27377=CARTESIAN_POINT('Ctrl Pts',(-0.167307501784475,1.,-1.95069027794294));
#27378=CARTESIAN_POINT('Ctrl Pts',(-0.168455741607556,1.,-1.94493757756931));
#27379=CARTESIAN_POINT('Ctrl Pts',(-0.169534904817491,1.,-1.93915639211581));
#27380=CARTESIAN_POINT('Ctrl Pts',(-0.170541253116202,1.,-1.93329183155539));
#27381=CARTESIAN_POINT('Ctrl Pts',(-0.171471191532988,1.,-1.92731093582036));
#27382=CARTESIAN_POINT('Ctrl Pts',(-0.172321621259514,1.,-1.9212233439798));
#27383=CARTESIAN_POINT('Ctrl Pts',(-0.173090695383496,1.,-1.91511429159527));
#27384=CARTESIAN_POINT('Ctrl Pts',(-0.173776635257817,1.,-1.90911693975267));
#27385=CARTESIAN_POINT('Ctrl Pts',(-0.174375518661085,1.,-1.90335253862834));
#27386=CARTESIAN_POINT('Ctrl Pts',(-0.174879405091263,1.,-1.89788101117132));
#27387=CARTESIAN_POINT('Ctrl Pts',(-0.175274276190844,1.,-1.892646301985));
#27388=CARTESIAN_POINT('Ctrl Pts',(-0.175538155840648,1.,-1.88742606273259));
#27389=CARTESIAN_POINT('Ctrl Pts',(-0.175644148889699,1.,-1.88188663145367));
#27390=CARTESIAN_POINT('Ctrl Pts',(-0.175563480746485,1.,-1.87563767773588));
#27391=CARTESIAN_POINT('Ctrl Pts',(-0.175268337590758,1.,-1.86828349694799));
#27392=CARTESIAN_POINT('Ctrl Pts',(-0.17473525927603,1.,-1.85948367088837));
#27393=CARTESIAN_POINT('Ctrl Pts',(-0.173946627587731,1.,-1.8489811319852));
#27394=CARTESIAN_POINT('Ctrl Pts',(-0.1728894428919,1.,-1.83658380527692));
#27395=CARTESIAN_POINT('Ctrl Pts',(-0.171554770204119,1.,-1.82215766811545));
#27396=CARTESIAN_POINT('Ctrl Pts',(-0.169936923904608,1.,-1.80561530629706));
#27397=CARTESIAN_POINT('Ctrl Pts',(-0.168032772805197,1.,-1.7869064998507));
#27398=CARTESIAN_POINT('Ctrl Pts',(-0.1662793551464,1.,-1.77018771684844));
#27399=CARTESIAN_POINT('Ctrl Pts',(-0.164834765707158,1.,-1.75666056638427));
#27400=CARTESIAN_POINT('Ctrl Pts',(-0.163814161002002,1.,-1.7472034950333));
#27401=CARTESIAN_POINT('Ctrl Pts',(-0.163289472382896,1.,-1.74236521665491));
#27402=CARTESIAN_POINT('',(-0.0694764450219581,0.,-2.19890268624765));
#27403=CARTESIAN_POINT('Origin',(0.0694764450219584,0.,-2.19890268624765));
#27404=CARTESIAN_POINT('',(0.0694764450219584,1.,-2.19890268624765));
#27405=CARTESIAN_POINT('',(-0.0694764450219581,1.,-2.19890268624765));
#27406=CARTESIAN_POINT('',(0.0694764450219584,0.,-2.19890268624765));
#27407=CARTESIAN_POINT('Ctrl Pts',(0.163289472382896,-1.,-1.74236521665491));
#27408=CARTESIAN_POINT('Ctrl Pts',(0.163289472382896,1.,-1.74236521665491));
#27409=CARTESIAN_POINT('Ctrl Pts',(0.163814161002474,-1.,-1.74720349503904));
#27410=CARTESIAN_POINT('Ctrl Pts',(0.163814161002474,1.,-1.74720349503904));
#27411=CARTESIAN_POINT('Ctrl Pts',(0.164834765708484,-1.,-1.75666056640041));
#27412=CARTESIAN_POINT('Ctrl Pts',(0.164834765708484,1.,-1.75666056640041));
#27413=CARTESIAN_POINT('Ctrl Pts',(0.166279355148738,-1.,-1.77018771687692));
#27414=CARTESIAN_POINT('Ctrl Pts',(0.166279355148738,1.,-1.77018771687692));
#27415=CARTESIAN_POINT('Ctrl Pts',(0.16803277280837,-1.,-1.78690649988931));
#27416=CARTESIAN_POINT('Ctrl Pts',(0.16803277280837,1.,-1.78690649988931));
#27417=CARTESIAN_POINT('Ctrl Pts',(0.169936923908078,-1.,-1.80561530633924));
#27418=CARTESIAN_POINT('Ctrl Pts',(0.169936923908078,1.,-1.80561530633924));
#27419=CARTESIAN_POINT('Ctrl Pts',(0.171554770207306,-1.,-1.82215766815414));
#27420=CARTESIAN_POINT('Ctrl Pts',(0.171554770207306,1.,-1.82215766815414));
#27421=CARTESIAN_POINT('Ctrl Pts',(0.17288944289442,-1.,-1.83658380530747));
#27422=CARTESIAN_POINT('Ctrl Pts',(0.17288944289442,1.,-1.83658380530747));
#27423=CARTESIAN_POINT('Ctrl Pts',(0.173946627589401,-1.,-1.84898113200543));
#27424=CARTESIAN_POINT('Ctrl Pts',(0.173946627589401,1.,-1.84898113200543));
#27425=CARTESIAN_POINT('Ctrl Pts',(0.174735259276856,-1.,-1.85948367089838));
#27426=CARTESIAN_POINT('Ctrl Pts',(0.174735259276856,1.,-1.85948367089838));
#27427=CARTESIAN_POINT('Ctrl Pts',(0.175268337590901,-1.,-1.86828349694972));
#27428=CARTESIAN_POINT('Ctrl Pts',(0.175268337590901,1.,-1.86828349694972));
#27429=CARTESIAN_POINT('Ctrl Pts',(0.175563480746205,-1.,-1.87563767773249));
#27430=CARTESIAN_POINT('Ctrl Pts',(0.175563480746205,1.,-1.87563767773249));
#27431=CARTESIAN_POINT('Ctrl Pts',(0.175644148889271,-1.,-1.88188663144846));
#27432=CARTESIAN_POINT('Ctrl Pts',(0.175644148889271,1.,-1.88188663144846));
#27433=CARTESIAN_POINT('Ctrl Pts',(0.175538155840286,-1.,-1.88742606272818));
#27434=CARTESIAN_POINT('Ctrl Pts',(0.175538155840286,1.,-1.88742606272818));
#27435=CARTESIAN_POINT('Ctrl Pts',(0.175274276190664,-1.,-1.89264630198279));
#27436=CARTESIAN_POINT('Ctrl Pts',(0.175274276190664,1.,-1.89264630198279));
#27437=CARTESIAN_POINT('Ctrl Pts',(0.174879405091277,-1.,-1.89788101117148));
#27438=CARTESIAN_POINT('Ctrl Pts',(0.174879405091277,1.,-1.89788101117148));
#27439=CARTESIAN_POINT('Ctrl Pts',(0.174375518661222,-1.,-1.90335253863003));
#27440=CARTESIAN_POINT('Ctrl Pts',(0.174375518661222,1.,-1.90335253863003));
#27441=CARTESIAN_POINT('Ctrl Pts',(0.173776635257984,-1.,-1.90911693975475));
#27442=CARTESIAN_POINT('Ctrl Pts',(0.173776635257984,1.,-1.90911693975475));
#27443=CARTESIAN_POINT('Ctrl Pts',(0.173090695383619,-1.,-1.91511429159681));
#27444=CARTESIAN_POINT('Ctrl Pts',(0.173090695383619,1.,-1.91511429159681));
#27445=CARTESIAN_POINT('Ctrl Pts',(0.172321621259557,-1.,-1.92122334398034));
#27446=CARTESIAN_POINT('Ctrl Pts',(0.172321621259557,1.,-1.92122334398034));
#27447=CARTESIAN_POINT('Ctrl Pts',(0.17147119153296,-1.,-1.92731093582));
#27448=CARTESIAN_POINT('Ctrl Pts',(0.17147119153296,1.,-1.92731093582));
#27449=CARTESIAN_POINT('Ctrl Pts',(0.170541253116136,-1.,-1.93329183155455));
#27450=CARTESIAN_POINT('Ctrl Pts',(0.170541253116136,1.,-1.93329183155455));
#27451=CARTESIAN_POINT('Ctrl Pts',(0.169534904817425,-1.,-1.93915639211497));
#27452=CARTESIAN_POINT('Ctrl Pts',(0.169534904817425,1.,-1.93915639211497));
#27453=CARTESIAN_POINT('Ctrl Pts',(0.168455741607516,-1.,-1.94493757756879));
#27454=CARTESIAN_POINT('Ctrl Pts',(0.168455741607516,1.,-1.94493757756879));
#27455=CARTESIAN_POINT('Ctrl Pts',(0.167307501784469,-1.,-1.95069027794286));
#27456=CARTESIAN_POINT('Ctrl Pts',(0.167307501784469,1.,-1.95069027794286));
#27457=CARTESIAN_POINT('Ctrl Pts',(0.166093592002833,-1.,-1.95646759718755));
#27458=CARTESIAN_POINT('Ctrl Pts',(0.166093592002833,1.,-1.95646759718755));
#27459=CARTESIAN_POINT('Ctrl Pts',(0.1648165689203,-1.,-1.96229379940174));
#27460=CARTESIAN_POINT('Ctrl Pts',(0.1648165689203,1.,-1.96229379940174));
#27461=CARTESIAN_POINT('Ctrl Pts',(0.16347818545776,-1.,-1.96816512678));
#27462=CARTESIAN_POINT('Ctrl Pts',(0.16347818545776,1.,-1.96816512678));
#27463=CARTESIAN_POINT('Ctrl Pts',(0.162079693556302,-1.,-1.97406280235204));
#27464=CARTESIAN_POINT('Ctrl Pts',(0.162079693556302,1.,-1.97406280235204));
#27465=CARTESIAN_POINT('Ctrl Pts',(0.16062206078461,-1.,-1.97996195437557));
#27466=CARTESIAN_POINT('Ctrl Pts',(0.16062206078461,1.,-1.97996195437557));
#27467=CARTESIAN_POINT('Ctrl Pts',(0.159106226437288,-1.,-1.98584238283279));
#27468=CARTESIAN_POINT('Ctrl Pts',(0.159106226437288,1.,-1.98584238283279));
#27469=CARTESIAN_POINT('Ctrl Pts',(0.157533331459215,-1.,-1.99169810931893));
#27470=CARTESIAN_POINT('Ctrl Pts',(0.157533331459215,1.,-1.99169810931893));
#27471=CARTESIAN_POINT('Ctrl Pts',(0.155904629548774,-1.,-1.99753284771487));
#27472=CARTESIAN_POINT('Ctrl Pts',(0.155904629548774,1.,-1.99753284771487));
#27473=CARTESIAN_POINT('Ctrl Pts',(0.154221403049719,-1.,-2.00335565310539));
#27474=CARTESIAN_POINT('Ctrl Pts',(0.154221403049719,1.,-2.00335565310539));
#27475=CARTESIAN_POINT('Ctrl Pts',(0.152484883621452,-1.,-2.00917680318426));
#27476=CARTESIAN_POINT('Ctrl Pts',(0.152484883621452,1.,-2.00917680318426));
#27477=CARTESIAN_POINT('Ctrl Pts',(0.150696157673084,-1.,-2.01500291940243));
#27478=CARTESIAN_POINT('Ctrl Pts',(0.150696157673084,1.,-2.01500291940243));
#27479=CARTESIAN_POINT('Ctrl Pts',(0.148856124775343,-1.,-2.02083464969897));
#27480=CARTESIAN_POINT('Ctrl Pts',(0.148856124775343,1.,-2.02083464969897));
#27481=CARTESIAN_POINT('Ctrl Pts',(0.146965557332586,-1.,-2.02666926182017));
#27482=CARTESIAN_POINT('Ctrl Pts',(0.146965557332586,1.,-2.02666926182017));
#27483=CARTESIAN_POINT('Ctrl Pts',(0.145025140186058,-1.,-2.03250223739941));
#27484=CARTESIAN_POINT('Ctrl Pts',(0.145025140186058,1.,-2.03250223739941));
#27485=CARTESIAN_POINT('Ctrl Pts',(0.143035515058208,-1.,-2.03832911025913));
#27486=CARTESIAN_POINT('Ctrl Pts',(0.143035515058208,1.,-2.03832911025913));
#27487=CARTESIAN_POINT('Ctrl Pts',(0.140997332152545,-1.,-2.04414757947919));
#27488=CARTESIAN_POINT('Ctrl Pts',(0.140997332152545,1.,-2.04414757947919));
#27489=CARTESIAN_POINT('Ctrl Pts',(0.138911255368966,-1.,-2.04995762001333));
#27490=CARTESIAN_POINT('Ctrl Pts',(0.138911255368966,1.,-2.04995762001333));
#27491=CARTESIAN_POINT('Ctrl Pts',(0.136777941218044,-1.,-2.0557604441427));
#27492=CARTESIAN_POINT('Ctrl Pts',(0.136777941218044,1.,-2.0557604441427));
#27493=CARTESIAN_POINT('Ctrl Pts',(0.134598026192107,-1.,-2.06155781517844));
#27494=CARTESIAN_POINT('Ctrl Pts',(0.134598026192107,1.,-2.06155781517844));
#27495=CARTESIAN_POINT('Ctrl Pts',(0.13237211154771,-1.,-2.06735123910319));
#27496=CARTESIAN_POINT('Ctrl Pts',(0.13237211154771,1.,-2.06735123910319));
#27497=CARTESIAN_POINT('Ctrl Pts',(0.1301007483284,-1.,-2.07314114713047));
#27498=CARTESIAN_POINT('Ctrl Pts',(0.1301007483284,1.,-2.07314114713047));
#27499=CARTESIAN_POINT('Ctrl Pts',(0.127784445276116,-1.,-2.07892715110967));
#27500=CARTESIAN_POINT('Ctrl Pts',(0.127784445276116,1.,-2.07892715110967));
#27501=CARTESIAN_POINT('Ctrl Pts',(0.125423679412058,-1.,-2.08470840653628));
#27502=CARTESIAN_POINT('Ctrl Pts',(0.125423679412058,1.,-2.08470840653628));
#27503=CARTESIAN_POINT('Ctrl Pts',(0.123018905621083,-1.,-2.09048392424826));
#27504=CARTESIAN_POINT('Ctrl Pts',(0.123018905621083,1.,-2.09048392424826));
#27505=CARTESIAN_POINT('Ctrl Pts',(0.120570567965129,-1.,-2.09625292867756));
#27506=CARTESIAN_POINT('Ctrl Pts',(0.120570567965129,1.,-2.09625292867756));
#27507=CARTESIAN_POINT('Ctrl Pts',(0.118079107988368,-1.,-2.10201512132945));
#27508=CARTESIAN_POINT('Ctrl Pts',(0.118079107988368,1.,-2.10201512132945));
#27509=CARTESIAN_POINT('Ctrl Pts',(0.11554495768794,-1.,-2.10777050261359));
#27510=CARTESIAN_POINT('Ctrl Pts',(0.11554495768794,1.,-2.10777050261359));
#27511=CARTESIAN_POINT('Ctrl Pts',(0.112968534419746,-1.,-2.11351924490335));
#27512=CARTESIAN_POINT('Ctrl Pts',(0.112968534419746,1.,-2.11351924490335));
#27513=CARTESIAN_POINT('Ctrl Pts',(0.11035023613502,-1.,-2.11926155590849));
#27514=CARTESIAN_POINT('Ctrl Pts',(0.11035023613502,1.,-2.11926155590849));
#27515=CARTESIAN_POINT('Ctrl Pts',(0.107690435231068,-1.,-2.12499752306927));
#27516=CARTESIAN_POINT('Ctrl Pts',(0.107690435231068,1.,-2.12499752306927));
#27517=CARTESIAN_POINT('Ctrl Pts',(0.104989479152703,-1.,-2.1307270488718));
#27518=CARTESIAN_POINT('Ctrl Pts',(0.104989479152703,1.,-2.1307270488718));
#27519=CARTESIAN_POINT('Ctrl Pts',(0.102247700556064,-1.,-2.13644992667052));
#27520=CARTESIAN_POINT('Ctrl Pts',(0.102247700556064,1.,-2.13644992667052));
#27521=CARTESIAN_POINT('Ctrl Pts',(0.0994654261990743,-1.,-2.14216588395974));
#27522=CARTESIAN_POINT('Ctrl Pts',(0.0994654261990743,1.,-2.14216588395974));
#27523=CARTESIAN_POINT('Ctrl Pts',(0.0966429852305689,-1.,-2.14787463531864));
#27524=CARTESIAN_POINT('Ctrl Pts',(0.0966429852305689,1.,-2.14787463531864));
#27525=CARTESIAN_POINT('Ctrl Pts',(0.0937807218868345,-1.,-2.15357593978377));
#27526=CARTESIAN_POINT('Ctrl Pts',(0.0937807218868345,1.,-2.15357593978377));
#27527=CARTESIAN_POINT('Ctrl Pts',(0.0908789888108266,-1.,-2.15926961544808));
#27528=CARTESIAN_POINT('Ctrl Pts',(0.0908789888108266,1.,-2.15926961544808));
#27529=CARTESIAN_POINT('Ctrl Pts',(0.0879381291387823,-1.,-2.16495552645275));
#27530=CARTESIAN_POINT('Ctrl Pts',(0.0879381291387823,1.,-2.16495552645275));
#27531=CARTESIAN_POINT('Ctrl Pts',(0.0849584620835643,-1.,-2.17063357871031));
#27532=CARTESIAN_POINT('Ctrl Pts',(0.0849584620835643,1.,-2.17063357871031));
#27533=CARTESIAN_POINT('Ctrl Pts',(0.0819402680871939,-1.,-2.1763037121106));
#27534=CARTESIAN_POINT('Ctrl Pts',(0.0819402680871939,1.,-2.1763037121106));
#27535=CARTESIAN_POINT('Ctrl Pts',(0.0788837727683228,-1.,-2.18196589448304));
#27536=CARTESIAN_POINT('Ctrl Pts',(0.0788837727683228,1.,-2.18196589448304));
#27537=CARTESIAN_POINT('Ctrl Pts',(0.0757891465833411,-1.,-2.1876201139874));
#27538=CARTESIAN_POINT('Ctrl Pts',(0.0757891465833411,1.,-2.1876201139874));
#27539=CARTESIAN_POINT('Ctrl Pts',(0.0732830357304276,-1.,-2.19213712012956));
#27540=CARTESIAN_POINT('Ctrl Pts',(0.0732830357304276,1.,-2.19213712012956));
#27541=CARTESIAN_POINT('Ctrl Pts',(0.0713863779524627,-1.,-2.19552129483562));
#27542=CARTESIAN_POINT('Ctrl Pts',(0.0713863779524627,1.,-2.19552129483562));
#27543=CARTESIAN_POINT('Ctrl Pts',(0.0701143536324926,-1.,-2.19777582085261));
#27544=CARTESIAN_POINT('Ctrl Pts',(0.0701143536324926,1.,-2.19777582085261));
#27545=CARTESIAN_POINT('Ctrl Pts',(0.0694764450219584,-1.,-2.19890268624765));
#27546=CARTESIAN_POINT('Ctrl Pts',(0.0694764450219584,1.,-2.19890268624765));
#27547=CARTESIAN_POINT('',(0.163289472382896,1.,-1.74236521665491));
#27548=CARTESIAN_POINT('Ctrl Pts',(0.163289472382896,1.,-1.74236521665491));
#27549=CARTESIAN_POINT('Ctrl Pts',(0.163814161002474,1.,-1.74720349503904));
#27550=CARTESIAN_POINT('Ctrl Pts',(0.164834765708484,1.,-1.75666056640041));
#27551=CARTESIAN_POINT('Ctrl Pts',(0.166279355148738,1.,-1.77018771687692));
#27552=CARTESIAN_POINT('Ctrl Pts',(0.16803277280837,1.,-1.78690649988931));
#27553=CARTESIAN_POINT('Ctrl Pts',(0.169936923908078,1.,-1.80561530633924));
#27554=CARTESIAN_POINT('Ctrl Pts',(0.171554770207306,1.,-1.82215766815414));
#27555=CARTESIAN_POINT('Ctrl Pts',(0.17288944289442,1.,-1.83658380530747));
#27556=CARTESIAN_POINT('Ctrl Pts',(0.173946627589401,1.,-1.84898113200543));
#27557=CARTESIAN_POINT('Ctrl Pts',(0.174735259276856,1.,-1.85948367089838));
#27558=CARTESIAN_POINT('Ctrl Pts',(0.175268337590901,1.,-1.86828349694972));
#27559=CARTESIAN_POINT('Ctrl Pts',(0.175563480746205,1.,-1.87563767773249));
#27560=CARTESIAN_POINT('Ctrl Pts',(0.175644148889271,1.,-1.88188663144846));
#27561=CARTESIAN_POINT('Ctrl Pts',(0.175538155840286,1.,-1.88742606272818));
#27562=CARTESIAN_POINT('Ctrl Pts',(0.175274276190664,1.,-1.89264630198279));
#27563=CARTESIAN_POINT('Ctrl Pts',(0.174879405091277,1.,-1.89788101117148));
#27564=CARTESIAN_POINT('Ctrl Pts',(0.174375518661222,1.,-1.90335253863003));
#27565=CARTESIAN_POINT('Ctrl Pts',(0.173776635257984,1.,-1.90911693975475));
#27566=CARTESIAN_POINT('Ctrl Pts',(0.173090695383619,1.,-1.91511429159681));
#27567=CARTESIAN_POINT('Ctrl Pts',(0.172321621259557,1.,-1.92122334398034));
#27568=CARTESIAN_POINT('Ctrl Pts',(0.17147119153296,1.,-1.92731093582));
#27569=CARTESIAN_POINT('Ctrl Pts',(0.170541253116136,1.,-1.93329183155455));
#27570=CARTESIAN_POINT('Ctrl Pts',(0.169534904817425,1.,-1.93915639211497));
#27571=CARTESIAN_POINT('Ctrl Pts',(0.168455741607516,1.,-1.94493757756879));
#27572=CARTESIAN_POINT('Ctrl Pts',(0.167307501784469,1.,-1.95069027794286));
#27573=CARTESIAN_POINT('Ctrl Pts',(0.166093592002833,1.,-1.95646759718755));
#27574=CARTESIAN_POINT('Ctrl Pts',(0.1648165689203,1.,-1.96229379940174));
#27575=CARTESIAN_POINT('Ctrl Pts',(0.16347818545776,1.,-1.96816512678));
#27576=CARTESIAN_POINT('Ctrl Pts',(0.162079693556302,1.,-1.97406280235204));
#27577=CARTESIAN_POINT('Ctrl Pts',(0.16062206078461,1.,-1.97996195437557));
#27578=CARTESIAN_POINT('Ctrl Pts',(0.159106226437288,1.,-1.98584238283279));
#27579=CARTESIAN_POINT('Ctrl Pts',(0.157533331459215,1.,-1.99169810931893));
#27580=CARTESIAN_POINT('Ctrl Pts',(0.155904629548774,1.,-1.99753284771487));
#27581=CARTESIAN_POINT('Ctrl Pts',(0.154221403049719,1.,-2.00335565310539));
#27582=CARTESIAN_POINT('Ctrl Pts',(0.152484883621452,1.,-2.00917680318426));
#27583=CARTESIAN_POINT('Ctrl Pts',(0.150696157673084,1.,-2.01500291940243));
#27584=CARTESIAN_POINT('Ctrl Pts',(0.148856124775343,1.,-2.02083464969897));
#27585=CARTESIAN_POINT('Ctrl Pts',(0.146965557332586,1.,-2.02666926182017));
#27586=CARTESIAN_POINT('Ctrl Pts',(0.145025140186058,1.,-2.03250223739941));
#27587=CARTESIAN_POINT('Ctrl Pts',(0.143035515058208,1.,-2.03832911025913));
#27588=CARTESIAN_POINT('Ctrl Pts',(0.140997332152545,1.,-2.04414757947919));
#27589=CARTESIAN_POINT('Ctrl Pts',(0.138911255368966,1.,-2.04995762001333));
#27590=CARTESIAN_POINT('Ctrl Pts',(0.136777941218044,1.,-2.0557604441427));
#27591=CARTESIAN_POINT('Ctrl Pts',(0.134598026192107,1.,-2.06155781517844));
#27592=CARTESIAN_POINT('Ctrl Pts',(0.13237211154771,1.,-2.06735123910319));
#27593=CARTESIAN_POINT('Ctrl Pts',(0.1301007483284,1.,-2.07314114713047));
#27594=CARTESIAN_POINT('Ctrl Pts',(0.127784445276116,1.,-2.07892715110967));
#27595=CARTESIAN_POINT('Ctrl Pts',(0.125423679412058,1.,-2.08470840653628));
#27596=CARTESIAN_POINT('Ctrl Pts',(0.123018905621083,1.,-2.09048392424826));
#27597=CARTESIAN_POINT('Ctrl Pts',(0.120570567965129,1.,-2.09625292867756));
#27598=CARTESIAN_POINT('Ctrl Pts',(0.118079107988368,1.,-2.10201512132945));
#27599=CARTESIAN_POINT('Ctrl Pts',(0.11554495768794,1.,-2.10777050261359));
#27600=CARTESIAN_POINT('Ctrl Pts',(0.112968534419746,1.,-2.11351924490335));
#27601=CARTESIAN_POINT('Ctrl Pts',(0.11035023613502,1.,-2.11926155590849));
#27602=CARTESIAN_POINT('Ctrl Pts',(0.107690435231068,1.,-2.12499752306927));
#27603=CARTESIAN_POINT('Ctrl Pts',(0.104989479152703,1.,-2.1307270488718));
#27604=CARTESIAN_POINT('Ctrl Pts',(0.102247700556064,1.,-2.13644992667052));
#27605=CARTESIAN_POINT('Ctrl Pts',(0.0994654261990743,1.,-2.14216588395974));
#27606=CARTESIAN_POINT('Ctrl Pts',(0.0966429852305689,1.,-2.14787463531864));
#27607=CARTESIAN_POINT('Ctrl Pts',(0.0937807218868345,1.,-2.15357593978377));
#27608=CARTESIAN_POINT('Ctrl Pts',(0.0908789888108266,1.,-2.15926961544808));
#27609=CARTESIAN_POINT('Ctrl Pts',(0.0879381291387823,1.,-2.16495552645275));
#27610=CARTESIAN_POINT('Ctrl Pts',(0.0849584620835643,1.,-2.17063357871031));
#27611=CARTESIAN_POINT('Ctrl Pts',(0.0819402680871939,1.,-2.1763037121106));
#27612=CARTESIAN_POINT('Ctrl Pts',(0.0788837727683228,1.,-2.18196589448304));
#27613=CARTESIAN_POINT('Ctrl Pts',(0.0757891465833411,1.,-2.1876201139874));
#27614=CARTESIAN_POINT('Ctrl Pts',(0.0732830357304276,1.,-2.19213712012956));
#27615=CARTESIAN_POINT('Ctrl Pts',(0.0713863779524627,1.,-2.19552129483562));
#27616=CARTESIAN_POINT('Ctrl Pts',(0.0701143536324926,1.,-2.19777582085261));
#27617=CARTESIAN_POINT('Ctrl Pts',(0.0694764450219584,1.,-2.19890268624765));
#27618=CARTESIAN_POINT('',(0.163289472382896,0.,-1.74236521665491));
#27619=CARTESIAN_POINT('Origin',(0.,0.,0.));
#27620=CARTESIAN_POINT('',(0.383122945602004,1.,-1.7075470150345));
#27621=CARTESIAN_POINT('Origin',(0.,1.,0.));
#27622=CARTESIAN_POINT('',(0.383122945602004,0.,-1.7075470150345));
#27623=CARTESIAN_POINT('Ctrl Pts',(0.61342227326009,-1.,-2.11275013067528));
#27624=CARTESIAN_POINT('Ctrl Pts',(0.61342227326009,1.,-2.11275013067528));
#27625=CARTESIAN_POINT('Ctrl Pts',(0.61246736556225,-1.,-2.11187554260142));
#27626=CARTESIAN_POINT('Ctrl Pts',(0.61246736556225,1.,-2.11187554260142));
#27627=CARTESIAN_POINT('Ctrl Pts',(0.610560911691113,-1.,-2.11012443807661));
#27628=CARTESIAN_POINT('Ctrl Pts',(0.610560911691113,1.,-2.11012443807661));
#27629=CARTESIAN_POINT('Ctrl Pts',(0.607711315456826,-1.,-2.10749199615859));
#27630=CARTESIAN_POINT('Ctrl Pts',(0.607711315456826,1.,-2.10749199615859));
#27631=CARTESIAN_POINT('Ctrl Pts',(0.603932030738212,-1.,-2.10397049887709));
#27632=CARTESIAN_POINT('Ctrl Pts',(0.603932030738212,1.,-2.10397049887709));
#27633=CARTESIAN_POINT('Ctrl Pts',(0.599241616422144,-1.,-2.09954930865331));
#27634=CARTESIAN_POINT('Ctrl Pts',(0.599241616422144,1.,-2.09954930865331));
#27635=CARTESIAN_POINT('Ctrl Pts',(0.594585006052823,-1.,-2.09510876220501));
#27636=CARTESIAN_POINT('Ctrl Pts',(0.594585006052823,1.,-2.09510876220501));
#27637=CARTESIAN_POINT('Ctrl Pts',(0.589962365403189,-1.,-2.09064881812053));
#27638=CARTESIAN_POINT('Ctrl Pts',(0.589962365403189,1.,-2.09064881812053));
#27639=CARTESIAN_POINT('Ctrl Pts',(0.585373918990895,-1.,-2.086169437277));
#27640=CARTESIAN_POINT('Ctrl Pts',(0.585373918990895,1.,-2.086169437277));
#27641=CARTESIAN_POINT('Ctrl Pts',(0.580819952107256,-1.,-2.08167059018138));
#27642=CARTESIAN_POINT('Ctrl Pts',(0.580819952107256,1.,-2.08167059018138));
#27643=CARTESIAN_POINT('Ctrl Pts',(0.576300797416274,-1.,-2.07715226767361));
#27644=CARTESIAN_POINT('Ctrl Pts',(0.576300797416274,1.,-2.07715226767361));
#27645=CARTESIAN_POINT('Ctrl Pts',(0.571816823242411,-1.,-2.07261449292758));
#27646=CARTESIAN_POINT('Ctrl Pts',(0.571816823242411,1.,-2.07261449292758));
#27647=CARTESIAN_POINT('Ctrl Pts',(0.567368421181229,-1.,-2.06805732997383));
#27648=CARTESIAN_POINT('Ctrl Pts',(0.567368421181229,1.,-2.06805732997383));
#27649=CARTESIAN_POINT('Ctrl Pts',(0.562955993082574,-1.,-2.06348090160697));
#27650=CARTESIAN_POINT('Ctrl Pts',(0.562955993082574,1.,-2.06348090160697));
#27651=CARTESIAN_POINT('Ctrl Pts',(0.558579940185467,-1.,-2.05888537756571));
#27652=CARTESIAN_POINT('Ctrl Pts',(0.558579940185467,1.,-2.05888537756571));
#27653=CARTESIAN_POINT('Ctrl Pts',(0.554240657464109,-1.,-2.05427091604482));
#27654=CARTESIAN_POINT('Ctrl Pts',(0.554240657464109,1.,-2.05427091604482));
#27655=CARTESIAN_POINT('Ctrl Pts',(0.549938525150342,-1.,-2.04963761077974));
#27656=CARTESIAN_POINT('Ctrl Pts',(0.549938525150342,1.,-2.04963761077974));
#27657=CARTESIAN_POINT('Ctrl Pts',(0.545673903817348,-1.,-2.0449854471456));
#27658=CARTESIAN_POINT('Ctrl Pts',(0.545673903817348,1.,-2.0449854471456));
#27659=CARTESIAN_POINT('Ctrl Pts',(0.54144712061552,-1.,-2.0403142269048));
#27660=CARTESIAN_POINT('Ctrl Pts',(0.54144712061552,1.,-2.0403142269048));
#27661=CARTESIAN_POINT('Ctrl Pts',(0.537258489833134,-1.,-2.03562362953993));
#27662=CARTESIAN_POINT('Ctrl Pts',(0.537258489833134,1.,-2.03562362953993));
#27663=CARTESIAN_POINT('Ctrl Pts',(0.533108355132905,-1.,-2.03091336214401));
#27664=CARTESIAN_POINT('Ctrl Pts',(0.533108355132905,1.,-2.03091336214401));
#27665=CARTESIAN_POINT('Ctrl Pts',(0.52899712724191,-1.,-2.02618329083289));
#27666=CARTESIAN_POINT('Ctrl Pts',(0.52899712724191,1.,-2.02618329083289));
#27667=CARTESIAN_POINT('Ctrl Pts',(0.524925318333518,-1.,-2.02143356304712));
#27668=CARTESIAN_POINT('Ctrl Pts',(0.524925318333518,1.,-2.02143356304712));
#27669=CARTESIAN_POINT('Ctrl Pts',(0.520893590399428,-1.,-2.01666477917306));
#27670=CARTESIAN_POINT('Ctrl Pts',(0.520893590399428,1.,-2.01666477917306));
#27671=CARTESIAN_POINT('Ctrl Pts',(0.516902681728733,-1.,-2.01187773939257));
#27672=CARTESIAN_POINT('Ctrl Pts',(0.516902681728733,1.,-2.01187773939257));
#27673=CARTESIAN_POINT('Ctrl Pts',(0.512953306961813,-1.,-2.00707309946955));
#27674=CARTESIAN_POINT('Ctrl Pts',(0.512953306961813,1.,-2.00707309946955));
#27675=CARTESIAN_POINT('Ctrl Pts',(0.509046069886152,-1.,-2.00225107134733));
#27676=CARTESIAN_POINT('Ctrl Pts',(0.509046069886152,1.,-2.00225107134733));
#27677=CARTESIAN_POINT('Ctrl Pts',(0.505181361323011,-1.,-1.99741107463567));
#27678=CARTESIAN_POINT('Ctrl Pts',(0.505181361323011,1.,-1.99741107463567));
#27679=CARTESIAN_POINT('Ctrl Pts',(0.501359287727129,-1.,-1.9925514912615));
#27680=CARTESIAN_POINT('Ctrl Pts',(0.501359287727129,1.,-1.9925514912615));
#27681=CARTESIAN_POINT('Ctrl Pts',(0.497579909545564,-1.,-1.98767044752929));
#27682=CARTESIAN_POINT('Ctrl Pts',(0.497579909545564,1.,-1.98767044752929));
#27683=CARTESIAN_POINT('Ctrl Pts',(0.493843476541492,-1.,-1.9827665876182));
#27684=CARTESIAN_POINT('Ctrl Pts',(0.493843476541492,1.,-1.9827665876182));
#27685=CARTESIAN_POINT('Ctrl Pts',(0.490150627860955,-1.,-1.97783973019229));
#27686=CARTESIAN_POINT('Ctrl Pts',(0.490150627860955,1.,-1.97783973019229));
#27687=CARTESIAN_POINT('Ctrl Pts',(0.486502692907661,-1.,-1.97289186263272));
#27688=CARTESIAN_POINT('Ctrl Pts',(0.486502692907661,1.,-1.97289186263272));
#27689=CARTESIAN_POINT('Ctrl Pts',(0.482901662120686,-1.,-1.96792703422358));
#27690=CARTESIAN_POINT('Ctrl Pts',(0.482901662120686,1.,-1.96792703422358));
#27691=CARTESIAN_POINT('Ctrl Pts',(0.479349583074846,-1.,-1.96294933055938));
#27692=CARTESIAN_POINT('Ctrl Pts',(0.479349583074846,1.,-1.96294933055938));
#27693=CARTESIAN_POINT('Ctrl Pts',(0.475848034683171,-1.,-1.95796111148175));
#27694=CARTESIAN_POINT('Ctrl Pts',(0.475848034683171,1.,-1.95796111148175));
#27695=CARTESIAN_POINT('Ctrl Pts',(0.472397672264079,-1.,-1.95296148278136));
#27696=CARTESIAN_POINT('Ctrl Pts',(0.472397672264079,1.,-1.95296148278136));
#27697=CARTESIAN_POINT('Ctrl Pts',(0.468997482913158,-1.,-1.94794381136524));
#27698=CARTESIAN_POINT('Ctrl Pts',(0.468997482913158,1.,-1.94794381136524));
#27699=CARTESIAN_POINT('Ctrl Pts',(0.465645462026064,-1.,-1.94289794196205));
#27700=CARTESIAN_POINT('Ctrl Pts',(0.465645462026064,1.,-1.94289794196205));
#27701=CARTESIAN_POINT('Ctrl Pts',(0.462340031009087,-1.,-1.93781486640834));
#27702=CARTESIAN_POINT('Ctrl Pts',(0.462340031009087,1.,-1.93781486640834));
#27703=CARTESIAN_POINT('Ctrl Pts',(0.459081234547931,-1.,-1.93269066517936));
#27704=CARTESIAN_POINT('Ctrl Pts',(0.459081234547931,1.,-1.93269066517936));
#27705=CARTESIAN_POINT('Ctrl Pts',(0.455872005174335,-1.,-1.92753067150461));
#27706=CARTESIAN_POINT('Ctrl Pts',(0.455872005174335,1.,-1.92753067150461));
#27707=CARTESIAN_POINT('Ctrl Pts',(0.452719478359356,-1.,-1.9223538064847));
#27708=CARTESIAN_POINT('Ctrl Pts',(0.452719478359356,1.,-1.9223538064847));
#27709=CARTESIAN_POINT('Ctrl Pts',(0.449632260106572,-1.,-1.91718342555717));
#27710=CARTESIAN_POINT('Ctrl Pts',(0.449632260106572,1.,-1.91718342555717));
#27711=CARTESIAN_POINT('Ctrl Pts',(0.446617343485651,-1.,-1.91203699981095));
#27712=CARTESIAN_POINT('Ctrl Pts',(0.446617343485651,1.,-1.91203699981095));
#27713=CARTESIAN_POINT('Ctrl Pts',(0.44367755684917,-1.,-1.90691756144906));
#27714=CARTESIAN_POINT('Ctrl Pts',(0.44367755684917,1.,-1.90691756144906));
#27715=CARTESIAN_POINT('Ctrl Pts',(0.44080783370416,-1.,-1.90180124389137));
#27716=CARTESIAN_POINT('Ctrl Pts',(0.44080783370416,1.,-1.90180124389137));
#27717=CARTESIAN_POINT('Ctrl Pts',(0.437995003948443,-1.,-1.89663648956549));
#27718=CARTESIAN_POINT('Ctrl Pts',(0.437995003948443,1.,-1.89663648956549));
#27719=CARTESIAN_POINT('Ctrl Pts',(0.43522566096358,-1.,-1.89136993975585));
#27720=CARTESIAN_POINT('Ctrl Pts',(0.43522566096358,1.,-1.89136993975585));
#27721=CARTESIAN_POINT('Ctrl Pts',(0.432493038548833,-1.,-1.88596913666828));
#27722=CARTESIAN_POINT('Ctrl Pts',(0.432493038548833,1.,-1.88596913666828));
#27723=CARTESIAN_POINT('Ctrl Pts',(0.429803062482217,-1.,-1.88044229001779));
#27724=CARTESIAN_POINT('Ctrl Pts',(0.429803062482217,1.,-1.88044229001779));
#27725=CARTESIAN_POINT('Ctrl Pts',(0.427183828518743,-1.,-1.87486989291334));
#27726=CARTESIAN_POINT('Ctrl Pts',(0.427183828518743,1.,-1.87486989291334));
#27727=CARTESIAN_POINT('Ctrl Pts',(0.424678177290876,-1.,-1.8693780394412));
#27728=CARTESIAN_POINT('Ctrl Pts',(0.424678177290876,1.,-1.8693780394412));
#27729=CARTESIAN_POINT('Ctrl Pts',(0.422327307417884,-1.,-1.86408083333863));
#27730=CARTESIAN_POINT('Ctrl Pts',(0.422327307417884,1.,-1.86408083333863));
#27731=CARTESIAN_POINT('Ctrl Pts',(0.420157287975583,-1.,-1.8590328109667));
#27732=CARTESIAN_POINT('Ctrl Pts',(0.420157287975583,1.,-1.8590328109667));
#27733=CARTESIAN_POINT('Ctrl Pts',(0.418164129144045,-1.,-1.8541763285645));
#27734=CARTESIAN_POINT('Ctrl Pts',(0.418164129144045,1.,-1.8541763285645));
#27735=CARTESIAN_POINT('Ctrl Pts',(0.416300022039885,-1.,-1.84929312930314));
#27736=CARTESIAN_POINT('Ctrl Pts',(0.416300022039885,1.,-1.84929312930314));
#27737=CARTESIAN_POINT('Ctrl Pts',(0.414487438255542,-1.,-1.84405757074218));
#27738=CARTESIAN_POINT('Ctrl Pts',(0.414487438255542,1.,-1.84405757074218));
#27739=CARTESIAN_POINT('Ctrl Pts',(0.412633125322945,-1.,-1.8380895347617));
#27740=CARTESIAN_POINT('Ctrl Pts',(0.412633125322945,1.,-1.8380895347617));
#27741=CARTESIAN_POINT('Ctrl Pts',(0.410641256301276,-1.,-1.83100408895047));
#27742=CARTESIAN_POINT('Ctrl Pts',(0.410641256301276,1.,-1.83100408895047));
#27743=CARTESIAN_POINT('Ctrl Pts',(0.408428948106227,-1.,-1.82247022677562));
#27744=CARTESIAN_POINT('Ctrl Pts',(0.408428948106227,1.,-1.82247022677562));
#27745=CARTESIAN_POINT('Ctrl Pts',(0.405933518407175,-1.,-1.81223801812013));
#27746=CARTESIAN_POINT('Ctrl Pts',(0.405933518407175,1.,-1.81223801812013));
#27747=CARTESIAN_POINT('Ctrl Pts',(0.403107976163396,-1.,-1.80012077173238));
#27748=CARTESIAN_POINT('Ctrl Pts',(0.403107976163396,1.,-1.80012077173238));
#27749=CARTESIAN_POINT('Ctrl Pts',(0.399919403774155,-1.,-1.78598826343754));
#27750=CARTESIAN_POINT('Ctrl Pts',(0.399919403774155,1.,-1.78598826343754));
#27751=CARTESIAN_POINT('Ctrl Pts',(0.396346196110688,-1.,-1.76975560043442));
#27752=CARTESIAN_POINT('Ctrl Pts',(0.396346196110688,1.,-1.76975560043442));
#27753=CARTESIAN_POINT('Ctrl Pts',(0.392375812285395,-1.,-1.75137405310193));
#27754=CARTESIAN_POINT('Ctrl Pts',(0.392375812285395,1.,-1.75137405310193));
#27755=CARTESIAN_POINT('Ctrl Pts',(0.388877023502615,-1.,-1.73493170972829));
#27756=CARTESIAN_POINT('Ctrl Pts',(0.388877023502615,1.,-1.73493170972829));
#27757=CARTESIAN_POINT('Ctrl Pts',(0.386070790323281,-1.,-1.72162022244582));
#27758=CARTESIAN_POINT('Ctrl Pts',(0.386070790323281,1.,-1.72162022244582));
#27759=CARTESIAN_POINT('Ctrl Pts',(0.384119047314215,-1.,-1.71231062891398));
#27760=CARTESIAN_POINT('Ctrl Pts',(0.384119047314215,1.,-1.71231062891398));
#27761=CARTESIAN_POINT('Ctrl Pts',(0.383122945602004,-1.,-1.7075470150345));
#27762=CARTESIAN_POINT('Ctrl Pts',(0.383122945602004,1.,-1.7075470150345));
#27763=CARTESIAN_POINT('',(0.61342227326009,1.,-2.11275013067528));
#27764=CARTESIAN_POINT('Ctrl Pts',(0.61342227326009,1.,-2.11275013067528));
#27765=CARTESIAN_POINT('Ctrl Pts',(0.61246736556225,1.,-2.11187554260142));
#27766=CARTESIAN_POINT('Ctrl Pts',(0.610560911691113,1.,-2.11012443807661));
#27767=CARTESIAN_POINT('Ctrl Pts',(0.607711315456826,1.,-2.10749199615859));
#27768=CARTESIAN_POINT('Ctrl Pts',(0.603932030738212,1.,-2.10397049887709));
#27769=CARTESIAN_POINT('Ctrl Pts',(0.599241616422144,1.,-2.09954930865331));
#27770=CARTESIAN_POINT('Ctrl Pts',(0.594585006052823,1.,-2.09510876220501));
#27771=CARTESIAN_POINT('Ctrl Pts',(0.589962365403189,1.,-2.09064881812053));
#27772=CARTESIAN_POINT('Ctrl Pts',(0.585373918990895,1.,-2.086169437277));
#27773=CARTESIAN_POINT('Ctrl Pts',(0.580819952107256,1.,-2.08167059018138));
#27774=CARTESIAN_POINT('Ctrl Pts',(0.576300797416274,1.,-2.07715226767361));
#27775=CARTESIAN_POINT('Ctrl Pts',(0.571816823242411,1.,-2.07261449292758));
#27776=CARTESIAN_POINT('Ctrl Pts',(0.567368421181229,1.,-2.06805732997383));
#27777=CARTESIAN_POINT('Ctrl Pts',(0.562955993082574,1.,-2.06348090160697));
#27778=CARTESIAN_POINT('Ctrl Pts',(0.558579940185467,1.,-2.05888537756571));
#27779=CARTESIAN_POINT('Ctrl Pts',(0.554240657464109,1.,-2.05427091604482));
#27780=CARTESIAN_POINT('Ctrl Pts',(0.549938525150342,1.,-2.04963761077974));
#27781=CARTESIAN_POINT('Ctrl Pts',(0.545673903817348,1.,-2.0449854471456));
#27782=CARTESIAN_POINT('Ctrl Pts',(0.54144712061552,1.,-2.0403142269048));
#27783=CARTESIAN_POINT('Ctrl Pts',(0.537258489833134,1.,-2.03562362953993));
#27784=CARTESIAN_POINT('Ctrl Pts',(0.533108355132905,1.,-2.03091336214401));
#27785=CARTESIAN_POINT('Ctrl Pts',(0.52899712724191,1.,-2.02618329083289));
#27786=CARTESIAN_POINT('Ctrl Pts',(0.524925318333518,1.,-2.02143356304712));
#27787=CARTESIAN_POINT('Ctrl Pts',(0.520893590399428,1.,-2.01666477917306));
#27788=CARTESIAN_POINT('Ctrl Pts',(0.516902681728733,1.,-2.01187773939257));
#27789=CARTESIAN_POINT('Ctrl Pts',(0.512953306961813,1.,-2.00707309946955));
#27790=CARTESIAN_POINT('Ctrl Pts',(0.509046069886152,1.,-2.00225107134733));
#27791=CARTESIAN_POINT('Ctrl Pts',(0.505181361323011,1.,-1.99741107463567));
#27792=CARTESIAN_POINT('Ctrl Pts',(0.501359287727129,1.,-1.9925514912615));
#27793=CARTESIAN_POINT('Ctrl Pts',(0.497579909545564,1.,-1.98767044752929));
#27794=CARTESIAN_POINT('Ctrl Pts',(0.493843476541492,1.,-1.9827665876182));
#27795=CARTESIAN_POINT('Ctrl Pts',(0.490150627860955,1.,-1.97783973019229));
#27796=CARTESIAN_POINT('Ctrl Pts',(0.486502692907661,1.,-1.97289186263272));
#27797=CARTESIAN_POINT('Ctrl Pts',(0.482901662120686,1.,-1.96792703422358));
#27798=CARTESIAN_POINT('Ctrl Pts',(0.479349583074846,1.,-1.96294933055938));
#27799=CARTESIAN_POINT('Ctrl Pts',(0.475848034683171,1.,-1.95796111148175));
#27800=CARTESIAN_POINT('Ctrl Pts',(0.472397672264079,1.,-1.95296148278136));
#27801=CARTESIAN_POINT('Ctrl Pts',(0.468997482913158,1.,-1.94794381136524));
#27802=CARTESIAN_POINT('Ctrl Pts',(0.465645462026064,1.,-1.94289794196205));
#27803=CARTESIAN_POINT('Ctrl Pts',(0.462340031009087,1.,-1.93781486640834));
#27804=CARTESIAN_POINT('Ctrl Pts',(0.459081234547931,1.,-1.93269066517936));
#27805=CARTESIAN_POINT('Ctrl Pts',(0.455872005174335,1.,-1.92753067150461));
#27806=CARTESIAN_POINT('Ctrl Pts',(0.452719478359356,1.,-1.9223538064847));
#27807=CARTESIAN_POINT('Ctrl Pts',(0.449632260106572,1.,-1.91718342555717));
#27808=CARTESIAN_POINT('Ctrl Pts',(0.446617343485651,1.,-1.91203699981095));
#27809=CARTESIAN_POINT('Ctrl Pts',(0.44367755684917,1.,-1.90691756144906));
#27810=CARTESIAN_POINT('Ctrl Pts',(0.44080783370416,1.,-1.90180124389137));
#27811=CARTESIAN_POINT('Ctrl Pts',(0.437995003948443,1.,-1.89663648956549));
#27812=CARTESIAN_POINT('Ctrl Pts',(0.43522566096358,1.,-1.89136993975585));
#27813=CARTESIAN_POINT('Ctrl Pts',(0.432493038548833,1.,-1.88596913666828));
#27814=CARTESIAN_POINT('Ctrl Pts',(0.429803062482217,1.,-1.88044229001779));
#27815=CARTESIAN_POINT('Ctrl Pts',(0.427183828518743,1.,-1.87486989291334));
#27816=CARTESIAN_POINT('Ctrl Pts',(0.424678177290876,1.,-1.8693780394412));
#27817=CARTESIAN_POINT('Ctrl Pts',(0.422327307417884,1.,-1.86408083333863));
#27818=CARTESIAN_POINT('Ctrl Pts',(0.420157287975583,1.,-1.8590328109667));
#27819=CARTESIAN_POINT('Ctrl Pts',(0.418164129144045,1.,-1.8541763285645));
#27820=CARTESIAN_POINT('Ctrl Pts',(0.416300022039885,1.,-1.84929312930314));
#27821=CARTESIAN_POINT('Ctrl Pts',(0.414487438255542,1.,-1.84405757074218));
#27822=CARTESIAN_POINT('Ctrl Pts',(0.412633125322945,1.,-1.8380895347617));
#27823=CARTESIAN_POINT('Ctrl Pts',(0.410641256301276,1.,-1.83100408895047));
#27824=CARTESIAN_POINT('Ctrl Pts',(0.408428948106227,1.,-1.82247022677562));
#27825=CARTESIAN_POINT('Ctrl Pts',(0.405933518407175,1.,-1.81223801812013));
#27826=CARTESIAN_POINT('Ctrl Pts',(0.403107976163396,1.,-1.80012077173238));
#27827=CARTESIAN_POINT('Ctrl Pts',(0.399919403774155,1.,-1.78598826343754));
#27828=CARTESIAN_POINT('Ctrl Pts',(0.396346196110688,1.,-1.76975560043442));
#27829=CARTESIAN_POINT('Ctrl Pts',(0.392375812285395,1.,-1.75137405310193));
#27830=CARTESIAN_POINT('Ctrl Pts',(0.388877023502615,1.,-1.73493170972829));
#27831=CARTESIAN_POINT('Ctrl Pts',(0.386070790323281,1.,-1.72162022244582));
#27832=CARTESIAN_POINT('Ctrl Pts',(0.384119047314215,1.,-1.71231062891398));
#27833=CARTESIAN_POINT('Ctrl Pts',(0.383122945602004,1.,-1.7075470150345));
#27834=CARTESIAN_POINT('',(0.61342227326009,0.,-2.11275013067528));
#27835=CARTESIAN_POINT('Origin',(0.745574324794401,0.,-2.0698113262342));
#27836=CARTESIAN_POINT('',(0.745574324794401,1.,-2.0698113262342));
#27837=CARTESIAN_POINT('',(0.61342227326009,1.,-2.11275013067528));
#27838=CARTESIAN_POINT('',(0.745574324794401,0.,-2.0698113262342));
#27839=CARTESIAN_POINT('Ctrl Pts',(0.693717979106306,-1.,-1.60662857109684));
#27840=CARTESIAN_POINT('Ctrl Pts',(0.693717979106306,1.,-1.60662857109684));
#27841=CARTESIAN_POINT('Ctrl Pts',(0.695712097881194,-1.,-1.61106790958151));
#27842=CARTESIAN_POINT('Ctrl Pts',(0.695712097881194,1.,-1.61106790958151));
#27843=CARTESIAN_POINT('Ctrl Pts',(0.699605146405088,-1.,-1.61974673472612));
#27844=CARTESIAN_POINT('Ctrl Pts',(0.699605146405088,1.,-1.61974673472612));
#27845=CARTESIAN_POINT('Ctrl Pts',(0.705159151988319,-1.,-1.63216541664676));
#27846=CARTESIAN_POINT('Ctrl Pts',(0.705159151988319,1.,-1.63216541664676));
#27847=CARTESIAN_POINT('Ctrl Pts',(0.711993139355394,-1.,-1.64752408832016));
#27848=CARTESIAN_POINT('Ctrl Pts',(0.711993139355394,1.,-1.64752408832016));
#27849=CARTESIAN_POINT('Ctrl Pts',(0.719585433804282,-1.,-1.6647288055568));
#27850=CARTESIAN_POINT('Ctrl Pts',(0.719585433804282,1.,-1.6647288055568));
#27851=CARTESIAN_POINT('Ctrl Pts',(0.726235967997433,-1.,-1.67996158455503));
#27852=CARTESIAN_POINT('Ctrl Pts',(0.726235967997433,1.,-1.67996158455503));
#27853=CARTESIAN_POINT('Ctrl Pts',(0.731963238697195,-1.,-1.69326921975743));
#27854=CARTESIAN_POINT('Ctrl Pts',(0.731963238697195,1.,-1.69326921975743));
#27855=CARTESIAN_POINT('Ctrl Pts',(0.736799665724771,-1.,-1.70473309006121));
#27856=CARTESIAN_POINT('Ctrl Pts',(0.736799665724771,1.,-1.70473309006121));
#27857=CARTESIAN_POINT('Ctrl Pts',(0.740795162032087,-1.,-1.71447789751927));
#27858=CARTESIAN_POINT('Ctrl Pts',(0.740795162032087,1.,-1.71447789751927));
#27859=CARTESIAN_POINT('Ctrl Pts',(0.744021445433764,-1.,-1.7226822991693));
#27860=CARTESIAN_POINT('Ctrl Pts',(0.744021445433764,1.,-1.7226822991693));
#27861=CARTESIAN_POINT('Ctrl Pts',(0.746574710096436,-1.,-1.72958533647399));
#27862=CARTESIAN_POINT('Ctrl Pts',(0.746574710096436,1.,-1.72958533647399));
#27863=CARTESIAN_POINT('Ctrl Pts',(0.748582462954854,-1.,-1.73550351679848));
#27864=CARTESIAN_POINT('Ctrl Pts',(0.748582462954854,1.,-1.73550351679848));
#27865=CARTESIAN_POINT('Ctrl Pts',(0.75019343597954,-1.,-1.74080458266705));
#27866=CARTESIAN_POINT('Ctrl Pts',(0.75019343597954,1.,-1.74080458266705));
#27867=CARTESIAN_POINT('Ctrl Pts',(0.751555614163629,-1.,-1.74585086852298));
#27868=CARTESIAN_POINT('Ctrl Pts',(0.751555614163629,1.,-1.74585086852298));
#27869=CARTESIAN_POINT('Ctrl Pts',(0.752797683531377,-1.,-1.75095139468809));
#27870=CARTESIAN_POINT('Ctrl Pts',(0.752797683531377,1.,-1.75095139468809));
#27871=CARTESIAN_POINT('Ctrl Pts',(0.75400925402848,-1.,-1.75631083600175));
#27872=CARTESIAN_POINT('Ctrl Pts',(0.75400925402848,1.,-1.75631083600175));
#27873=CARTESIAN_POINT('Ctrl Pts',(0.755220979975262,-1.,-1.7619781724032));
#27874=CARTESIAN_POINT('Ctrl Pts',(0.755220979975262,1.,-1.7619781724032));
#27875=CARTESIAN_POINT('Ctrl Pts',(0.756421896028403,-1.,-1.76789396003141));
#27876=CARTESIAN_POINT('Ctrl Pts',(0.756421896028403,1.,-1.76789396003141));
#27877=CARTESIAN_POINT('Ctrl Pts',(0.757578264077238,-1.,-1.77394167108342));
#27878=CARTESIAN_POINT('Ctrl Pts',(0.757578264077238,1.,-1.77394167108342));
#27879=CARTESIAN_POINT('Ctrl Pts',(0.75865062667738,-1.,-1.77999411220912));
#27880=CARTESIAN_POINT('Ctrl Pts',(0.75865062667738,1.,-1.77999411220912));
#27881=CARTESIAN_POINT('Ctrl Pts',(0.759614401109868,-1.,-1.78596964884527));
#27882=CARTESIAN_POINT('Ctrl Pts',(0.759614401109868,1.,-1.78596964884527));
#27883=CARTESIAN_POINT('Ctrl Pts',(0.760469555880425,-1.,-1.79185815610802));
#27884=CARTESIAN_POINT('Ctrl Pts',(0.760469555880425,1.,-1.79185815610802));
#27885=CARTESIAN_POINT('Ctrl Pts',(0.761229695230359,-1.,-1.79768986997735));
#27886=CARTESIAN_POINT('Ctrl Pts',(0.761229695230359,1.,-1.79768986997735));
#27887=CARTESIAN_POINT('Ctrl Pts',(0.761915336443515,-1.,-1.80351583877334));
#27888=CARTESIAN_POINT('Ctrl Pts',(0.761915336443515,1.,-1.80351583877334));
#27889=CARTESIAN_POINT('Ctrl Pts',(0.762546129464036,-1.,-1.80938551463989));
#27890=CARTESIAN_POINT('Ctrl Pts',(0.762546129464036,1.,-1.80938551463989));
#27891=CARTESIAN_POINT('Ctrl Pts',(0.763132003836783,-1.,-1.81532118405566));
#27892=CARTESIAN_POINT('Ctrl Pts',(0.763132003836783,1.,-1.81532118405566));
#27893=CARTESIAN_POINT('Ctrl Pts',(0.763673465462854,-1.,-1.82131873145297));
#27894=CARTESIAN_POINT('Ctrl Pts',(0.763673465462854,1.,-1.82131873145297));
#27895=CARTESIAN_POINT('Ctrl Pts',(0.764165902606055,-1.,-1.8273599120008));
#27896=CARTESIAN_POINT('Ctrl Pts',(0.764165902606055,1.,-1.8273599120008));
#27897=CARTESIAN_POINT('Ctrl Pts',(0.764602549687845,-1.,-1.8334207722714));
#27898=CARTESIAN_POINT('Ctrl Pts',(0.764602549687845,1.,-1.8334207722714));
#27899=CARTESIAN_POINT('Ctrl Pts',(0.764978057881687,-1.,-1.83948181064823));
#27900=CARTESIAN_POINT('Ctrl Pts',(0.764978057881687,1.,-1.83948181064823));
#27901=CARTESIAN_POINT('Ctrl Pts',(0.765291664861971,-1.,-1.84553698875911));
#27902=CARTESIAN_POINT('Ctrl Pts',(0.765291664861971,1.,-1.84553698875911));
#27903=CARTESIAN_POINT('Ctrl Pts',(0.765545710619023,-1.,-1.85158945130054));
#27904=CARTESIAN_POINT('Ctrl Pts',(0.765545710619023,1.,-1.85158945130054));
#27905=CARTESIAN_POINT('Ctrl Pts',(0.765744212909305,-1.,-1.85764741390391));
#27906=CARTESIAN_POINT('Ctrl Pts',(0.765744212909305,1.,-1.85764741390391));
#27907=CARTESIAN_POINT('Ctrl Pts',(0.765891519092557,-1.,-1.86372027063315));
#27908=CARTESIAN_POINT('Ctrl Pts',(0.765891519092557,1.,-1.86372027063315));
#27909=CARTESIAN_POINT('Ctrl Pts',(0.765990708546111,-1.,-1.86981398314345));
#27910=CARTESIAN_POINT('Ctrl Pts',(0.765990708546111,1.,-1.86981398314345));
#27911=CARTESIAN_POINT('Ctrl Pts',(0.766042837036759,-1.,-1.87592888967886));
#27912=CARTESIAN_POINT('Ctrl Pts',(0.766042837036759,1.,-1.87592888967886));
#27913=CARTESIAN_POINT('Ctrl Pts',(0.766047794851868,-1.,-1.88206215302561));
#27914=CARTESIAN_POINT('Ctrl Pts',(0.766047794851868,1.,-1.88206215302561));
#27915=CARTESIAN_POINT('Ctrl Pts',(0.76600483706209,-1.,-1.88820926433409));
#27916=CARTESIAN_POINT('Ctrl Pts',(0.76600483706209,1.,-1.88820926433409));
#27917=CARTESIAN_POINT('Ctrl Pts',(0.765913193856979,-1.,-1.89436577771389));
#27918=CARTESIAN_POINT('Ctrl Pts',(0.765913193856979,1.,-1.89436577771389));
#27919=CARTESIAN_POINT('Ctrl Pts',(0.765772772593395,-1.,-1.90052930393599));
#27920=CARTESIAN_POINT('Ctrl Pts',(0.765772772593395,1.,-1.90052930393599));
#27921=CARTESIAN_POINT('Ctrl Pts',(0.765584196937936,-1.,-1.90669961402362));
#27922=CARTESIAN_POINT('Ctrl Pts',(0.765584196937936,1.,-1.90669961402362));
#27923=CARTESIAN_POINT('Ctrl Pts',(0.765348465884739,-1.,-1.91287765805174));
#27924=CARTESIAN_POINT('Ctrl Pts',(0.765348465884739,1.,-1.91287765805174));
#27925=CARTESIAN_POINT('Ctrl Pts',(0.765066729667095,-1.,-1.91906491634197));
#27926=CARTESIAN_POINT('Ctrl Pts',(0.765066729667095,1.,-1.91906491634197));
#27927=CARTESIAN_POINT('Ctrl Pts',(0.764740025488189,-1.,-1.92526263537041));
#27928=CARTESIAN_POINT('Ctrl Pts',(0.764740025488189,1.,-1.92526263537041));
#27929=CARTESIAN_POINT('Ctrl Pts',(0.764369010673889,-1.,-1.93147105496367));
#27930=CARTESIAN_POINT('Ctrl Pts',(0.764369010673889,1.,-1.93147105496367));
#27931=CARTESIAN_POINT('Ctrl Pts',(0.763954049121393,-1.,-1.93768964875867));
#27932=CARTESIAN_POINT('Ctrl Pts',(0.763954049121393,1.,-1.93768964875867));
#27933=CARTESIAN_POINT('Ctrl Pts',(0.76349533353858,-1.,-1.94391746617626));
#27934=CARTESIAN_POINT('Ctrl Pts',(0.76349533353858,1.,-1.94391746617626));
#27935=CARTESIAN_POINT('Ctrl Pts',(0.762992990878774,-1.,-1.95015342590025));
#27936=CARTESIAN_POINT('Ctrl Pts',(0.762992990878774,1.,-1.95015342590025));
#27937=CARTESIAN_POINT('Ctrl Pts',(0.762447203806263,-1.,-1.95639665309893));
#27938=CARTESIAN_POINT('Ctrl Pts',(0.762447203806263,1.,-1.95639665309893));
#27939=CARTESIAN_POINT('Ctrl Pts',(0.761858300014575,-1.,-1.96264672744229));
#27940=CARTESIAN_POINT('Ctrl Pts',(0.761858300014575,1.,-1.96264672744229));
#27941=CARTESIAN_POINT('Ctrl Pts',(0.761226690483986,-1.,-1.96890351582545));
#27942=CARTESIAN_POINT('Ctrl Pts',(0.761226690483986,1.,-1.96890351582545));
#27943=CARTESIAN_POINT('Ctrl Pts',(0.760552825409855,-1.,-1.97516705321521));
#27944=CARTESIAN_POINT('Ctrl Pts',(0.760552825409855,1.,-1.97516705321521));
#27945=CARTESIAN_POINT('Ctrl Pts',(0.759837147452135,-1.,-1.98143741418156));
#27946=CARTESIAN_POINT('Ctrl Pts',(0.759837147452135,1.,-1.98143741418156));
#27947=CARTESIAN_POINT('Ctrl Pts',(0.759080037802242,-1.,-1.98771456680806));
#27948=CARTESIAN_POINT('Ctrl Pts',(0.759080037802242,1.,-1.98771456680806));
#27949=CARTESIAN_POINT('Ctrl Pts',(0.758281796766377,-1.,-1.9939983109871));
#27950=CARTESIAN_POINT('Ctrl Pts',(0.758281796766377,1.,-1.9939983109871));
#27951=CARTESIAN_POINT('Ctrl Pts',(0.757442676862341,-1.,-2.00028834739072));
#27952=CARTESIAN_POINT('Ctrl Pts',(0.757442676862341,1.,-2.00028834739072));
#27953=CARTESIAN_POINT('Ctrl Pts',(0.756562904646496,-1.,-2.00658431587682));
#27954=CARTESIAN_POINT('Ctrl Pts',(0.756562904646496,1.,-2.00658431587682));
#27955=CARTESIAN_POINT('Ctrl Pts',(0.7556427049581,-1.,-2.01288584328149));
#27956=CARTESIAN_POINT('Ctrl Pts',(0.7556427049581,1.,-2.01288584328149));
#27957=CARTESIAN_POINT('Ctrl Pts',(0.75468233072352,-1.,-2.01919259406003));
#27958=CARTESIAN_POINT('Ctrl Pts',(0.75468233072352,1.,-2.01919259406003));
#27959=CARTESIAN_POINT('Ctrl Pts',(0.753682061113765,-1.,-2.02550428623587));
#27960=CARTESIAN_POINT('Ctrl Pts',(0.753682061113765,1.,-2.02550428623587));
#27961=CARTESIAN_POINT('Ctrl Pts',(0.752642180488104,-1.,-2.03182068456467));
#27962=CARTESIAN_POINT('Ctrl Pts',(0.752642180488104,1.,-2.03182068456467));
#27963=CARTESIAN_POINT('Ctrl Pts',(0.751562963361383,-1.,-2.03814160092173));
#27964=CARTESIAN_POINT('Ctrl Pts',(0.751562963361383,1.,-2.03814160092173));
#27965=CARTESIAN_POINT('Ctrl Pts',(0.750444657874758,-1.,-2.04446689147754));
#27966=CARTESIAN_POINT('Ctrl Pts',(0.750444657874758,1.,-2.04446689147754));
#27967=CARTESIAN_POINT('Ctrl Pts',(0.749287468663053,-1.,-2.05079645591606));
#27968=CARTESIAN_POINT('Ctrl Pts',(0.749287468663053,1.,-2.05079645591606));
#27969=CARTESIAN_POINT('Ctrl Pts',(0.748091554181101,-1.,-2.05713023030263));
#27970=CARTESIAN_POINT('Ctrl Pts',(0.748091554181101,1.,-2.05713023030263));
#27971=CARTESIAN_POINT('Ctrl Pts',(0.747103932785504,-1.,-2.06220058927162));
#27972=CARTESIAN_POINT('Ctrl Pts',(0.747103932785504,1.,-2.06220058927162));
#27973=CARTESIAN_POINT('Ctrl Pts',(0.746345871542695,-1.,-2.06600523016401));
#27974=CARTESIAN_POINT('Ctrl Pts',(0.746345871542695,1.,-2.06600523016401));
#27975=CARTESIAN_POINT('Ctrl Pts',(0.74583279137781,-1.,-2.06854248895575));
#27976=CARTESIAN_POINT('Ctrl Pts',(0.74583279137781,1.,-2.06854248895575));
#27977=CARTESIAN_POINT('Ctrl Pts',(0.745574324794401,-1.,-2.0698113262342));
#27978=CARTESIAN_POINT('Ctrl Pts',(0.745574324794401,1.,-2.0698113262342));
#27979=CARTESIAN_POINT('',(0.693717979106306,1.,-1.60662857109684));
#27980=CARTESIAN_POINT('Ctrl Pts',(0.693717979106306,1.,-1.60662857109684));
#27981=CARTESIAN_POINT('Ctrl Pts',(0.695712097881194,1.,-1.61106790958151));
#27982=CARTESIAN_POINT('Ctrl Pts',(0.699605146405088,1.,-1.61974673472612));
#27983=CARTESIAN_POINT('Ctrl Pts',(0.705159151988319,1.,-1.63216541664676));
#27984=CARTESIAN_POINT('Ctrl Pts',(0.711993139355394,1.,-1.64752408832016));
#27985=CARTESIAN_POINT('Ctrl Pts',(0.719585433804282,1.,-1.6647288055568));
#27986=CARTESIAN_POINT('Ctrl Pts',(0.726235967997433,1.,-1.67996158455503));
#27987=CARTESIAN_POINT('Ctrl Pts',(0.731963238697195,1.,-1.69326921975743));
#27988=CARTESIAN_POINT('Ctrl Pts',(0.736799665724771,1.,-1.70473309006121));
#27989=CARTESIAN_POINT('Ctrl Pts',(0.740795162032087,1.,-1.71447789751927));
#27990=CARTESIAN_POINT('Ctrl Pts',(0.744021445433764,1.,-1.7226822991693));
#27991=CARTESIAN_POINT('Ctrl Pts',(0.746574710096436,1.,-1.72958533647399));
#27992=CARTESIAN_POINT('Ctrl Pts',(0.748582462954854,1.,-1.73550351679848));
#27993=CARTESIAN_POINT('Ctrl Pts',(0.75019343597954,1.,-1.74080458266705));
#27994=CARTESIAN_POINT('Ctrl Pts',(0.751555614163629,1.,-1.74585086852298));
#27995=CARTESIAN_POINT('Ctrl Pts',(0.752797683531377,1.,-1.75095139468809));
#27996=CARTESIAN_POINT('Ctrl Pts',(0.75400925402848,1.,-1.75631083600175));
#27997=CARTESIAN_POINT('Ctrl Pts',(0.755220979975262,1.,-1.7619781724032));
#27998=CARTESIAN_POINT('Ctrl Pts',(0.756421896028403,1.,-1.76789396003141));
#27999=CARTESIAN_POINT('Ctrl Pts',(0.757578264077238,1.,-1.77394167108342));
#28000=CARTESIAN_POINT('Ctrl Pts',(0.75865062667738,1.,-1.77999411220912));
#28001=CARTESIAN_POINT('Ctrl Pts',(0.759614401109868,1.,-1.78596964884527));
#28002=CARTESIAN_POINT('Ctrl Pts',(0.760469555880425,1.,-1.79185815610802));
#28003=CARTESIAN_POINT('Ctrl Pts',(0.761229695230359,1.,-1.79768986997735));
#28004=CARTESIAN_POINT('Ctrl Pts',(0.761915336443515,1.,-1.80351583877334));
#28005=CARTESIAN_POINT('Ctrl Pts',(0.762546129464036,1.,-1.80938551463989));
#28006=CARTESIAN_POINT('Ctrl Pts',(0.763132003836783,1.,-1.81532118405566));
#28007=CARTESIAN_POINT('Ctrl Pts',(0.763673465462854,1.,-1.82131873145297));
#28008=CARTESIAN_POINT('Ctrl Pts',(0.764165902606055,1.,-1.8273599120008));
#28009=CARTESIAN_POINT('Ctrl Pts',(0.764602549687845,1.,-1.8334207722714));
#28010=CARTESIAN_POINT('Ctrl Pts',(0.764978057881687,1.,-1.83948181064823));
#28011=CARTESIAN_POINT('Ctrl Pts',(0.765291664861971,1.,-1.84553698875911));
#28012=CARTESIAN_POINT('Ctrl Pts',(0.765545710619023,1.,-1.85158945130054));
#28013=CARTESIAN_POINT('Ctrl Pts',(0.765744212909305,1.,-1.85764741390391));
#28014=CARTESIAN_POINT('Ctrl Pts',(0.765891519092557,1.,-1.86372027063315));
#28015=CARTESIAN_POINT('Ctrl Pts',(0.765990708546111,1.,-1.86981398314345));
#28016=CARTESIAN_POINT('Ctrl Pts',(0.766042837036759,1.,-1.87592888967886));
#28017=CARTESIAN_POINT('Ctrl Pts',(0.766047794851868,1.,-1.88206215302561));
#28018=CARTESIAN_POINT('Ctrl Pts',(0.76600483706209,1.,-1.88820926433409));
#28019=CARTESIAN_POINT('Ctrl Pts',(0.765913193856979,1.,-1.89436577771389));
#28020=CARTESIAN_POINT('Ctrl Pts',(0.765772772593395,1.,-1.90052930393599));
#28021=CARTESIAN_POINT('Ctrl Pts',(0.765584196937936,1.,-1.90669961402362));
#28022=CARTESIAN_POINT('Ctrl Pts',(0.765348465884739,1.,-1.91287765805174));
#28023=CARTESIAN_POINT('Ctrl Pts',(0.765066729667095,1.,-1.91906491634197));
#28024=CARTESIAN_POINT('Ctrl Pts',(0.764740025488189,1.,-1.92526263537041));
#28025=CARTESIAN_POINT('Ctrl Pts',(0.764369010673889,1.,-1.93147105496367));
#28026=CARTESIAN_POINT('Ctrl Pts',(0.763954049121393,1.,-1.93768964875867));
#28027=CARTESIAN_POINT('Ctrl Pts',(0.76349533353858,1.,-1.94391746617626));
#28028=CARTESIAN_POINT('Ctrl Pts',(0.762992990878774,1.,-1.95015342590025));
#28029=CARTESIAN_POINT('Ctrl Pts',(0.762447203806263,1.,-1.95639665309893));
#28030=CARTESIAN_POINT('Ctrl Pts',(0.761858300014575,1.,-1.96264672744229));
#28031=CARTESIAN_POINT('Ctrl Pts',(0.761226690483986,1.,-1.96890351582545));
#28032=CARTESIAN_POINT('Ctrl Pts',(0.760552825409855,1.,-1.97516705321521));
#28033=CARTESIAN_POINT('Ctrl Pts',(0.759837147452135,1.,-1.98143741418156));
#28034=CARTESIAN_POINT('Ctrl Pts',(0.759080037802242,1.,-1.98771456680806));
#28035=CARTESIAN_POINT('Ctrl Pts',(0.758281796766377,1.,-1.9939983109871));
#28036=CARTESIAN_POINT('Ctrl Pts',(0.757442676862341,1.,-2.00028834739072));
#28037=CARTESIAN_POINT('Ctrl Pts',(0.756562904646496,1.,-2.00658431587682));
#28038=CARTESIAN_POINT('Ctrl Pts',(0.7556427049581,1.,-2.01288584328149));
#28039=CARTESIAN_POINT('Ctrl Pts',(0.75468233072352,1.,-2.01919259406003));
#28040=CARTESIAN_POINT('Ctrl Pts',(0.753682061113765,1.,-2.02550428623587));
#28041=CARTESIAN_POINT('Ctrl Pts',(0.752642180488104,1.,-2.03182068456467));
#28042=CARTESIAN_POINT('Ctrl Pts',(0.751562963361383,1.,-2.03814160092173));
#28043=CARTESIAN_POINT('Ctrl Pts',(0.750444657874758,1.,-2.04446689147754));
#28044=CARTESIAN_POINT('Ctrl Pts',(0.749287468663053,1.,-2.05079645591606));
#28045=CARTESIAN_POINT('Ctrl Pts',(0.748091554181101,1.,-2.05713023030263));
#28046=CARTESIAN_POINT('Ctrl Pts',(0.747103932785504,1.,-2.06220058927162));
#28047=CARTESIAN_POINT('Ctrl Pts',(0.746345871542695,1.,-2.06600523016401));
#28048=CARTESIAN_POINT('Ctrl Pts',(0.74583279137781,1.,-2.06854248895575));
#28049=CARTESIAN_POINT('Ctrl Pts',(0.745574324794401,1.,-2.0698113262342));
#28050=CARTESIAN_POINT('',(0.693717979106306,0.,-1.60662857109684));
#28051=CARTESIAN_POINT('Origin',(0.,0.,0.));
#28052=CARTESIAN_POINT('',(0.892032620296855,1.,-1.5055822144029));
#28053=CARTESIAN_POINT('Origin',(0.,1.,0.));
#28054=CARTESIAN_POINT('',(0.892032620296855,0.,-1.5055822144029));
#28055=CARTESIAN_POINT('Ctrl Pts',(1.23627494547115,-1.,-1.81978687191668));
#28056=CARTESIAN_POINT('Ctrl Pts',(1.23627494547115,1.,-1.81978687191668));
#28057=CARTESIAN_POINT('Ctrl Pts',(1.23509651170476,-1.,-1.81925017193666));
#28058=CARTESIAN_POINT('Ctrl Pts',(1.23509651170476,1.,-1.81925017193666));
#28059=CARTESIAN_POINT('Ctrl Pts',(1.2327422452705,-1.,-1.81817389921279));
#28060=CARTESIAN_POINT('Ctrl Pts',(1.2327422452705,1.,-1.81817389921279));
#28061=CARTESIAN_POINT('Ctrl Pts',(1.2292186489137,-1.,-1.8165508718364));
#28062=CARTESIAN_POINT('Ctrl Pts',(1.2292186489137,1.,-1.8165508718364));
#28063=CARTESIAN_POINT('Ctrl Pts',(1.2245361330495,-1.,-1.81436959210434));
#28064=CARTESIAN_POINT('Ctrl Pts',(1.2245361330495,1.,-1.81436959210434));
#28065=CARTESIAN_POINT('Ctrl Pts',(1.21870906103557,-1.,-1.81161420806656));
#28066=CARTESIAN_POINT('Ctrl Pts',(1.21870906103557,1.,-1.81161420806656));
#28067=CARTESIAN_POINT('Ctrl Pts',(1.21290815708314,-1.,-1.80882996917129));
#28068=CARTESIAN_POINT('Ctrl Pts',(1.21290815708314,1.,-1.80882996917129));
#28069=CARTESIAN_POINT('Ctrl Pts',(1.20713356605475,-1.,-1.80601678480707));
#28070=CARTESIAN_POINT('Ctrl Pts',(1.20713356605475,1.,-1.80601678480707));
#28071=CARTESIAN_POINT('Ctrl Pts',(1.20138548938974,-1.,-1.80317454838603));
#28072=CARTESIAN_POINT('Ctrl Pts',(1.20138548938974,1.,-1.80317454838603));
#28073=CARTESIAN_POINT('Ctrl Pts',(1.19566418930242,-1.,-1.80030314369879));
#28074=CARTESIAN_POINT('Ctrl Pts',(1.19566418930242,1.,-1.80030314369879));
#28075=CARTESIAN_POINT('Ctrl Pts',(1.18996997934445,-1.,-1.79740245923478));
#28076=CARTESIAN_POINT('Ctrl Pts',(1.18996997934445,1.,-1.79740245923478));
#28077=CARTESIAN_POINT('Ctrl Pts',(1.18430321697432,-1.,-1.79447240321515));
#28078=CARTESIAN_POINT('Ctrl Pts',(1.18430321697432,1.,-1.79447240321515));
#28079=CARTESIAN_POINT('Ctrl Pts',(1.17866429440809,-1.,-1.79151291552689));
#28080=CARTESIAN_POINT('Ctrl Pts',(1.17866429440809,1.,-1.79151291552689));
#28081=CARTESIAN_POINT('Ctrl Pts',(1.17305363177328,-1.,-1.78852398877617));
#28082=CARTESIAN_POINT('Ctrl Pts',(1.17305363177328,1.,-1.78852398877617));
#28083=CARTESIAN_POINT('Ctrl Pts',(1.16747166312303,-1.,-1.78550566040443));
#28084=CARTESIAN_POINT('Ctrl Pts',(1.16747166312303,1.,-1.78550566040443));
#28085=CARTESIAN_POINT('Ctrl Pts',(1.16191881298499,-1.,-1.78245795881009));
#28086=CARTESIAN_POINT('Ctrl Pts',(1.16191881298499,1.,-1.78245795881009));
#28087=CARTESIAN_POINT('Ctrl Pts',(1.15639547194698,-1.,-1.77938085564275));
#28088=CARTESIAN_POINT('Ctrl Pts',(1.15639547194698,1.,-1.77938085564275));
#28089=CARTESIAN_POINT('Ctrl Pts',(1.15090197841514,-1.,-1.7762742255701));
#28090=CARTESIAN_POINT('Ctrl Pts',(1.15090197841514,1.,-1.7762742255701));
#28091=CARTESIAN_POINT('Ctrl Pts',(1.1454385822692,-1.,-1.77313777896194));
#28092=CARTESIAN_POINT('Ctrl Pts',(1.1454385822692,1.,-1.77313777896194));
#28093=CARTESIAN_POINT('Ctrl Pts',(1.14000548336975,-1.,-1.76997111386769));
#28094=CARTESIAN_POINT('Ctrl Pts',(1.14000548336975,1.,-1.76997111386769));
#28095=CARTESIAN_POINT('Ctrl Pts',(1.1346029180462,-1.,-1.76677384551862));
#28096=CARTESIAN_POINT('Ctrl Pts',(1.1346029180462,1.,-1.76677384551862));
#28097=CARTESIAN_POINT('Ctrl Pts',(1.12923123555075,-1.,-1.7635457196617));
#28098=CARTESIAN_POINT('Ctrl Pts',(1.12923123555075,1.,-1.7635457196617));
#28099=CARTESIAN_POINT('Ctrl Pts',(1.12389096855086,-1.,-1.76028671825096));
#28100=CARTESIAN_POINT('Ctrl Pts',(1.12389096855086,1.,-1.76028671825096));
#28101=CARTESIAN_POINT('Ctrl Pts',(1.11858293216763,-1.,-1.75699720772105));
#28102=CARTESIAN_POINT('Ctrl Pts',(1.11858293216763,1.,-1.75699720772105));
#28103=CARTESIAN_POINT('Ctrl Pts',(1.11330807582551,-1.,-1.7536777209463));
#28104=CARTESIAN_POINT('Ctrl Pts',(1.11330807582551,1.,-1.7536777209463));
#28105=CARTESIAN_POINT('Ctrl Pts',(1.10806728183007,-1.,-1.7503286607592));
#28106=CARTESIAN_POINT('Ctrl Pts',(1.10806728183007,1.,-1.7503286607592));
#28107=CARTESIAN_POINT('Ctrl Pts',(1.10286118991143,-1.,-1.74695004214923));
#28108=CARTESIAN_POINT('Ctrl Pts',(1.10286118991143,1.,-1.74695004214923));
#28109=CARTESIAN_POINT('Ctrl Pts',(1.09768999241225,-1.,-1.74354119236208));
#28110=CARTESIAN_POINT('Ctrl Pts',(1.09768999241225,1.,-1.74354119236208));
#28111=CARTESIAN_POINT('Ctrl Pts',(1.09255329056493,-1.,-1.74010053962247));
#28112=CARTESIAN_POINT('Ctrl Pts',(1.09255329056493,1.,-1.74010053962247));
#28113=CARTESIAN_POINT('Ctrl Pts',(1.08745056285427,-1.,-1.73662628326091));
#28114=CARTESIAN_POINT('Ctrl Pts',(1.08745056285427,1.,-1.73662628326091));
#28115=CARTESIAN_POINT('Ctrl Pts',(1.08238162784749,-1.,-1.73311705663407));
#28116=CARTESIAN_POINT('Ctrl Pts',(1.08238162784749,1.,-1.73311705663407));
#28117=CARTESIAN_POINT('Ctrl Pts',(1.0773470373727,-1.,-1.72957248977424));
#28118=CARTESIAN_POINT('Ctrl Pts',(1.0773470373727,1.,-1.72957248977424));
#28119=CARTESIAN_POINT('Ctrl Pts',(1.07234866990252,-1.,-1.72599406198488));
#28120=CARTESIAN_POINT('Ctrl Pts',(1.07234866990252,1.,-1.72599406198488));
#28121=CARTESIAN_POINT('Ctrl Pts',(1.06738966975462,-1.,-1.72238500928453));
#28122=CARTESIAN_POINT('Ctrl Pts',(1.06738966975462,1.,-1.72238500928453));
#28123=CARTESIAN_POINT('Ctrl Pts',(1.06247324680647,-1.,-1.71874858456904));
#28124=CARTESIAN_POINT('Ctrl Pts',(1.06247324680647,1.,-1.71874858456904));
#28125=CARTESIAN_POINT('Ctrl Pts',(1.05760163192479,-1.,-1.7150865442702));
#28126=CARTESIAN_POINT('Ctrl Pts',(1.05760163192479,1.,-1.7150865442702));
#28127=CARTESIAN_POINT('Ctrl Pts',(1.05277517202855,-1.,-1.71139783543989));
#28128=CARTESIAN_POINT('Ctrl Pts',(1.05277517202855,1.,-1.71139783543989));
#28129=CARTESIAN_POINT('Ctrl Pts',(1.04799085404995,-1.,-1.70767646263649));
#28130=CARTESIAN_POINT('Ctrl Pts',(1.04799085404995,1.,-1.70767646263649));
#28131=CARTESIAN_POINT('Ctrl Pts',(1.04324363334554,-1.,-1.70391338707982));
#28132=CARTESIAN_POINT('Ctrl Pts',(1.04324363334554,1.,-1.70391338707982));
#28133=CARTESIAN_POINT('Ctrl Pts',(1.03852922490789,-1.,-1.70010052930962));
#28134=CARTESIAN_POINT('Ctrl Pts',(1.03852922490789,1.,-1.70010052930962));
#28135=CARTESIAN_POINT('Ctrl Pts',(1.03384646003588,-1.,-1.69623414782771));
#28136=CARTESIAN_POINT('Ctrl Pts',(1.03384646003588,1.,-1.69623414782771));
#28137=CARTESIAN_POINT('Ctrl Pts',(1.02919977579147,-1.,-1.69231840863458));
#28138=CARTESIAN_POINT('Ctrl Pts',(1.02919977579147,1.,-1.69231840863458));
#28139=CARTESIAN_POINT('Ctrl Pts',(1.02460180535255,-1.,-1.68836910178447));
#28140=CARTESIAN_POINT('Ctrl Pts',(1.02460180535255,1.,-1.68836910178447));
#28141=CARTESIAN_POINT('Ctrl Pts',(1.02006795074201,-1.,-1.68440578021706));
#28142=CARTESIAN_POINT('Ctrl Pts',(1.02006795074201,1.,-1.68440578021706));
#28143=CARTESIAN_POINT('Ctrl Pts',(1.01561026162773,-1.,-1.68044289894798));
#28144=CARTESIAN_POINT('Ctrl Pts',(1.01561026162773,1.,-1.68044289894798));
#28145=CARTESIAN_POINT('Ctrl Pts',(1.01123236493511,-1.,-1.67648246776464));
#28146=CARTESIAN_POINT('Ctrl Pts',(1.01123236493511,1.,-1.67648246776464));
#28147=CARTESIAN_POINT('Ctrl Pts',(1.00692206696414,-1.,-1.67250335383293));
#28148=CARTESIAN_POINT('Ctrl Pts',(1.00692206696414,1.,-1.67250335383293));
#28149=CARTESIAN_POINT('Ctrl Pts',(1.00265091003727,-1.,-1.66846059277303));
#28150=CARTESIAN_POINT('Ctrl Pts',(1.00265091003727,1.,-1.66846059277303));
#28151=CARTESIAN_POINT('Ctrl Pts',(0.998389654952757,-1.,-1.66430758030376));
#28152=CARTESIAN_POINT('Ctrl Pts',(0.998389654952757,1.,-1.66430758030376));
#28153=CARTESIAN_POINT('Ctrl Pts',(0.994121836661305,-1.,-1.66001553809947));
#28154=CARTESIAN_POINT('Ctrl Pts',(0.994121836661305,1.,-1.66001553809947));
#28155=CARTESIAN_POINT('Ctrl Pts',(0.989855627854164,-1.,-1.65559044289699));
#28156=CARTESIAN_POINT('Ctrl Pts',(0.989855627854164,1.,-1.65559044289699));
#28157=CARTESIAN_POINT('Ctrl Pts',(0.98564262292082,-1.,-1.65110016612638));
#28158=CARTESIAN_POINT('Ctrl Pts',(0.98564262292082,1.,-1.65110016612638));
#28159=CARTESIAN_POINT('Ctrl Pts',(0.981562530939489,-1.,-1.64665139190656));
#28160=CARTESIAN_POINT('Ctrl Pts',(0.981562530939489,1.,-1.64665139190656));
#28161=CARTESIAN_POINT('Ctrl Pts',(0.977689794119416,-1.,-1.64233990826687));
#28162=CARTESIAN_POINT('Ctrl Pts',(0.977689794119416,1.,-1.64233990826687));
#28163=CARTESIAN_POINT('Ctrl Pts',(0.974066058287418,-1.,-1.63820952658144));
#28164=CARTESIAN_POINT('Ctrl Pts',(0.974066058287418,1.,-1.63820952658144));
#28165=CARTESIAN_POINT('Ctrl Pts',(0.970669715997509,-1.,-1.63420665729798));
#28166=CARTESIAN_POINT('Ctrl Pts',(0.970669715997509,1.,-1.63420665729798));
#28167=CARTESIAN_POINT('Ctrl Pts',(0.967387853230345,-1.,-1.63013849959462));
#28168=CARTESIAN_POINT('Ctrl Pts',(0.967387853230345,1.,-1.63013849959462));
#28169=CARTESIAN_POINT('Ctrl Pts',(0.964046107040535,-1.,-1.62571930670187));
#28170=CARTESIAN_POINT('Ctrl Pts',(0.964046107040535,1.,-1.62571930670187));
#28171=CARTESIAN_POINT('Ctrl Pts',(0.960438326101728,-1.,-1.62061638140221));
#28172=CARTESIAN_POINT('Ctrl Pts',(0.960438326101728,1.,-1.62061638140221));
#28173=CARTESIAN_POINT('Ctrl Pts',(0.95635442292067,-1.,-1.61449324337085));
#28174=CARTESIAN_POINT('Ctrl Pts',(0.95635442292067,1.,-1.61449324337085));
#28175=CARTESIAN_POINT('Ctrl Pts',(0.951613284356035,-1.,-1.60706069896936));
#28176=CARTESIAN_POINT('Ctrl Pts',(0.951613284356035,1.,-1.60706069896936));
#28177=CARTESIAN_POINT('Ctrl Pts',(0.946078063315257,-1.,-1.59810042043673));
#28178=CARTESIAN_POINT('Ctrl Pts',(0.946078063315257,1.,-1.59810042043673));
#28179=CARTESIAN_POINT('Ctrl Pts',(0.939646377893399,-1.,-1.58744937487176));
#28180=CARTESIAN_POINT('Ctrl Pts',(0.939646377893399,1.,-1.58744937487176));
#28181=CARTESIAN_POINT('Ctrl Pts',(0.932246680108685,-1.,-1.57499388382243));
#28182=CARTESIAN_POINT('Ctrl Pts',(0.932246680108685,1.,-1.57499388382243));
#28183=CARTESIAN_POINT('Ctrl Pts',(0.923832188944341,-1.,-1.56065988578893));
#28184=CARTESIAN_POINT('Ctrl Pts',(0.923832188944341,1.,-1.56065988578893));
#28185=CARTESIAN_POINT('Ctrl Pts',(0.914375919026456,-1.,-1.54440491149498));
#28186=CARTESIAN_POINT('Ctrl Pts',(0.914375919026456,1.,-1.54440491149498));
#28187=CARTESIAN_POINT('Ctrl Pts',(0.905967409625651,-1.,-1.52984849887993));
#28188=CARTESIAN_POINT('Ctrl Pts',(0.905967409625651,1.,-1.52984849887993));
#28189=CARTESIAN_POINT('Ctrl Pts',(0.89918504748351,-1.,-1.51805569590094));
#28190=CARTESIAN_POINT('Ctrl Pts',(0.89918504748351,1.,-1.51805569590094));
#28191=CARTESIAN_POINT('Ctrl Pts',(0.894452006964543,-1.,-1.50980486806688));
#28192=CARTESIAN_POINT('Ctrl Pts',(0.894452006964543,1.,-1.50980486806688));
#28193=CARTESIAN_POINT('Ctrl Pts',(0.892032620296855,-1.,-1.5055822144029));
#28194=CARTESIAN_POINT('Ctrl Pts',(0.892032620296855,1.,-1.5055822144029));
#28195=CARTESIAN_POINT('',(1.23627494547115,1.,-1.81978687191668));
#28196=CARTESIAN_POINT('Ctrl Pts',(1.23627494547115,1.,-1.81978687191668));
#28197=CARTESIAN_POINT('Ctrl Pts',(1.23509651170476,1.,-1.81925017193666));
#28198=CARTESIAN_POINT('Ctrl Pts',(1.2327422452705,1.,-1.81817389921279));
#28199=CARTESIAN_POINT('Ctrl Pts',(1.2292186489137,1.,-1.8165508718364));
#28200=CARTESIAN_POINT('Ctrl Pts',(1.2245361330495,1.,-1.81436959210434));
#28201=CARTESIAN_POINT('Ctrl Pts',(1.21870906103557,1.,-1.81161420806656));
#28202=CARTESIAN_POINT('Ctrl Pts',(1.21290815708314,1.,-1.80882996917129));
#28203=CARTESIAN_POINT('Ctrl Pts',(1.20713356605475,1.,-1.80601678480707));
#28204=CARTESIAN_POINT('Ctrl Pts',(1.20138548938974,1.,-1.80317454838603));
#28205=CARTESIAN_POINT('Ctrl Pts',(1.19566418930242,1.,-1.80030314369879));
#28206=CARTESIAN_POINT('Ctrl Pts',(1.18996997934445,1.,-1.79740245923478));
#28207=CARTESIAN_POINT('Ctrl Pts',(1.18430321697432,1.,-1.79447240321515));
#28208=CARTESIAN_POINT('Ctrl Pts',(1.17866429440809,1.,-1.79151291552689));
#28209=CARTESIAN_POINT('Ctrl Pts',(1.17305363177328,1.,-1.78852398877617));
#28210=CARTESIAN_POINT('Ctrl Pts',(1.16747166312303,1.,-1.78550566040443));
#28211=CARTESIAN_POINT('Ctrl Pts',(1.16191881298499,1.,-1.78245795881009));
#28212=CARTESIAN_POINT('Ctrl Pts',(1.15639547194698,1.,-1.77938085564275));
#28213=CARTESIAN_POINT('Ctrl Pts',(1.15090197841514,1.,-1.7762742255701));
#28214=CARTESIAN_POINT('Ctrl Pts',(1.1454385822692,1.,-1.77313777896194));
#28215=CARTESIAN_POINT('Ctrl Pts',(1.14000548336975,1.,-1.76997111386769));
#28216=CARTESIAN_POINT('Ctrl Pts',(1.1346029180462,1.,-1.76677384551862));
#28217=CARTESIAN_POINT('Ctrl Pts',(1.12923123555075,1.,-1.7635457196617));
#28218=CARTESIAN_POINT('Ctrl Pts',(1.12389096855086,1.,-1.76028671825096));
#28219=CARTESIAN_POINT('Ctrl Pts',(1.11858293216763,1.,-1.75699720772105));
#28220=CARTESIAN_POINT('Ctrl Pts',(1.11330807582551,1.,-1.7536777209463));
#28221=CARTESIAN_POINT('Ctrl Pts',(1.10806728183007,1.,-1.7503286607592));
#28222=CARTESIAN_POINT('Ctrl Pts',(1.10286118991143,1.,-1.74695004214923));
#28223=CARTESIAN_POINT('Ctrl Pts',(1.09768999241225,1.,-1.74354119236208));
#28224=CARTESIAN_POINT('Ctrl Pts',(1.09255329056493,1.,-1.74010053962247));
#28225=CARTESIAN_POINT('Ctrl Pts',(1.08745056285427,1.,-1.73662628326091));
#28226=CARTESIAN_POINT('Ctrl Pts',(1.08238162784749,1.,-1.73311705663407));
#28227=CARTESIAN_POINT('Ctrl Pts',(1.0773470373727,1.,-1.72957248977424));
#28228=CARTESIAN_POINT('Ctrl Pts',(1.07234866990252,1.,-1.72599406198488));
#28229=CARTESIAN_POINT('Ctrl Pts',(1.06738966975462,1.,-1.72238500928453));
#28230=CARTESIAN_POINT('Ctrl Pts',(1.06247324680647,1.,-1.71874858456904));
#28231=CARTESIAN_POINT('Ctrl Pts',(1.05760163192479,1.,-1.7150865442702));
#28232=CARTESIAN_POINT('Ctrl Pts',(1.05277517202855,1.,-1.71139783543989));
#28233=CARTESIAN_POINT('Ctrl Pts',(1.04799085404995,1.,-1.70767646263649));
#28234=CARTESIAN_POINT('Ctrl Pts',(1.04324363334554,1.,-1.70391338707982));
#28235=CARTESIAN_POINT('Ctrl Pts',(1.03852922490789,1.,-1.70010052930962));
#28236=CARTESIAN_POINT('Ctrl Pts',(1.03384646003588,1.,-1.69623414782771));
#28237=CARTESIAN_POINT('Ctrl Pts',(1.02919977579147,1.,-1.69231840863458));
#28238=CARTESIAN_POINT('Ctrl Pts',(1.02460180535255,1.,-1.68836910178447));
#28239=CARTESIAN_POINT('Ctrl Pts',(1.02006795074201,1.,-1.68440578021706));
#28240=CARTESIAN_POINT('Ctrl Pts',(1.01561026162773,1.,-1.68044289894798));
#28241=CARTESIAN_POINT('Ctrl Pts',(1.01123236493511,1.,-1.67648246776464));
#28242=CARTESIAN_POINT('Ctrl Pts',(1.00692206696414,1.,-1.67250335383293));
#28243=CARTESIAN_POINT('Ctrl Pts',(1.00265091003727,1.,-1.66846059277303));
#28244=CARTESIAN_POINT('Ctrl Pts',(0.998389654952757,1.,-1.66430758030376));
#28245=CARTESIAN_POINT('Ctrl Pts',(0.994121836661305,1.,-1.66001553809947));
#28246=CARTESIAN_POINT('Ctrl Pts',(0.989855627854164,1.,-1.65559044289699));
#28247=CARTESIAN_POINT('Ctrl Pts',(0.98564262292082,1.,-1.65110016612638));
#28248=CARTESIAN_POINT('Ctrl Pts',(0.981562530939489,1.,-1.64665139190656));
#28249=CARTESIAN_POINT('Ctrl Pts',(0.977689794119416,1.,-1.64233990826687));
#28250=CARTESIAN_POINT('Ctrl Pts',(0.974066058287418,1.,-1.63820952658144));
#28251=CARTESIAN_POINT('Ctrl Pts',(0.970669715997509,1.,-1.63420665729798));
#28252=CARTESIAN_POINT('Ctrl Pts',(0.967387853230345,1.,-1.63013849959462));
#28253=CARTESIAN_POINT('Ctrl Pts',(0.964046107040535,1.,-1.62571930670187));
#28254=CARTESIAN_POINT('Ctrl Pts',(0.960438326101728,1.,-1.62061638140221));
#28255=CARTESIAN_POINT('Ctrl Pts',(0.95635442292067,1.,-1.61449324337085));
#28256=CARTESIAN_POINT('Ctrl Pts',(0.951613284356035,1.,-1.60706069896936));
#28257=CARTESIAN_POINT('Ctrl Pts',(0.946078063315257,1.,-1.59810042043673));
#28258=CARTESIAN_POINT('Ctrl Pts',(0.939646377893399,1.,-1.58744937487176));
#28259=CARTESIAN_POINT('Ctrl Pts',(0.932246680108685,1.,-1.57499388382243));
#28260=CARTESIAN_POINT('Ctrl Pts',(0.923832188944341,1.,-1.56065988578893));
#28261=CARTESIAN_POINT('Ctrl Pts',(0.914375919026456,1.,-1.54440491149498));
#28262=CARTESIAN_POINT('Ctrl Pts',(0.905967409625651,1.,-1.52984849887993));
#28263=CARTESIAN_POINT('Ctrl Pts',(0.89918504748351,1.,-1.51805569590094));
#28264=CARTESIAN_POINT('Ctrl Pts',(0.894452006964543,1.,-1.50980486806688));
#28265=CARTESIAN_POINT('Ctrl Pts',(0.892032620296855,1.,-1.5055822144029));
#28266=CARTESIAN_POINT('',(1.23627494547115,0.,-1.81978687191668));
#28267=CARTESIAN_POINT('Origin',(1.34869019493419,0.,-1.73811241238545));
#28268=CARTESIAN_POINT('',(1.34869019493419,1.,-1.73811241238545));
#28269=CARTESIAN_POINT('',(1.23627494547115,1.,-1.81978687191668));
#28270=CARTESIAN_POINT('',(1.34869019493419,0.,-1.73811241238545));
#28271=CARTESIAN_POINT('Ctrl Pts',(1.15624053661742,-1.,-1.31362392696032));
#28272=CARTESIAN_POINT('Ctrl Pts',(1.15624053661742,1.,-1.31362392696032));
#28273=CARTESIAN_POINT('Ctrl Pts',(1.15950888730809,-1.,-1.31722977216397));
#28274=CARTESIAN_POINT('Ctrl Pts',(1.15950888730809,1.,-1.31722977216397));
#28275=CARTESIAN_POINT('Ctrl Pts',(1.16589330093588,-1.,-1.32428080721772));
#28276=CARTESIAN_POINT('Ctrl Pts',(1.16589330093588,1.,-1.32428080721772));
#28277=CARTESIAN_POINT('Ctrl Pts',(1.17501305789857,-1.,-1.33437539347008));
#28278=CARTESIAN_POINT('Ctrl Pts',(1.17501305789857,1.,-1.33437539347008));
#28279=CARTESIAN_POINT('Ctrl Pts',(1.18625865667441,-1.,-1.34687054001093));
#28280=CARTESIAN_POINT('Ctrl Pts',(1.18625865667441,1.,-1.34687054001093));
#28281=CARTESIAN_POINT('Ctrl Pts',(1.1987959077932,-1.,-1.36088705043885));
#28282=CARTESIAN_POINT('Ctrl Pts',(1.1987959077932,1.,-1.36088705043885));
#28283=CARTESIAN_POINT('Ctrl Pts',(1.20982812925645,-1.,-1.37331915607905));
#28284=CARTESIAN_POINT('Ctrl Pts',(1.20982812925645,1.,-1.37331915607905));
#28285=CARTESIAN_POINT('Ctrl Pts',(1.21938737280852,-1.,-1.38420564527715));
#28286=CARTESIAN_POINT('Ctrl Pts',(1.21938737280852,1.,-1.38420564527715));
#28287=CARTESIAN_POINT('Ctrl Pts',(1.22752961899387,-1.,-1.39361389568796));
#28288=CARTESIAN_POINT('Ctrl Pts',(1.22752961899387,1.,-1.39361389568796));
#28289=CARTESIAN_POINT('Ctrl Pts',(1.23434087290423,-1.,-1.40164708206106));
#28290=CARTESIAN_POINT('Ctrl Pts',(1.23434087290423,1.,-1.40164708206106));
#28291=CARTESIAN_POINT('Ctrl Pts',(1.23994455029534,-1.,-1.40845295531283));
#28292=CARTESIAN_POINT('Ctrl Pts',(1.23994455029534,1.,-1.40845295531283));
#28293=CARTESIAN_POINT('Ctrl Pts',(1.24450600513056,-1.,-1.41422913175179));
#28294=CARTESIAN_POINT('Ctrl Pts',(1.24450600513056,1.,-1.41422913175179));
#28295=CARTESIAN_POINT('Ctrl Pts',(1.24824430986571,-1.,-1.41923722596025));
#28296=CARTESIAN_POINT('Ctrl Pts',(1.24824430986571,1.,-1.41923722596025));
#28297=CARTESIAN_POINT('Ctrl Pts',(1.2514145557001,-1.,-1.42378102115575));
#28298=CARTESIAN_POINT('Ctrl Pts',(1.2514145557001,1.,-1.42378102115575));
#28299=CARTESIAN_POINT('Ctrl Pts',(1.25426945222639,-1.,-1.42815938799387));
#28300=CARTESIAN_POINT('Ctrl Pts',(1.25426945222639,1.,-1.42815938799387));
#28301=CARTESIAN_POINT('Ctrl Pts',(1.25702687965755,-1.,-1.43262645609691));
#28302=CARTESIAN_POINT('Ctrl Pts',(1.25702687965755,1.,-1.43262645609691));
#28303=CARTESIAN_POINT('Ctrl Pts',(1.25983531012005,-1.,-1.43734919180848));
#28304=CARTESIAN_POINT('Ctrl Pts',(1.25983531012005,1.,-1.43734919180848));
#28305=CARTESIAN_POINT('Ctrl Pts',(1.26273903323858,-1.,-1.44236470511303));
#28306=CARTESIAN_POINT('Ctrl Pts',(1.26273903323858,1.,-1.44236470511303));
#28307=CARTESIAN_POINT('Ctrl Pts',(1.26570925118868,-1.,-1.44761985001662));
#28308=CARTESIAN_POINT('Ctrl Pts',(1.26570925118868,1.,-1.44761985001662));
#28309=CARTESIAN_POINT('Ctrl Pts',(1.2686778680489,-1.,-1.45301422764247));
#28310=CARTESIAN_POINT('Ctrl Pts',(1.2686778680489,1.,-1.45301422764247));
#28311=CARTESIAN_POINT('Ctrl Pts',(1.27156805265289,-1.,-1.45843906294697));
#28312=CARTESIAN_POINT('Ctrl Pts',(1.27156805265289,1.,-1.45843906294697));
#28313=CARTESIAN_POINT('Ctrl Pts',(1.27433119897822,-1.,-1.46382431332476));
#28314=CARTESIAN_POINT('Ctrl Pts',(1.27433119897822,1.,-1.46382431332476));
#28315=CARTESIAN_POINT('Ctrl Pts',(1.27696414831089,-1.,-1.46916035917133));
#28316=CARTESIAN_POINT('Ctrl Pts',(1.27696414831089,1.,-1.46916035917133));
#28317=CARTESIAN_POINT('Ctrl Pts',(1.2794891824849,-1.,-1.4744717526707));
#28318=CARTESIAN_POINT('Ctrl Pts',(1.2794891824849,1.,-1.4744717526707));
#28319=CARTESIAN_POINT('Ctrl Pts',(1.28194158939517,-1.,-1.47980070347096));
#28320=CARTESIAN_POINT('Ctrl Pts',(1.28194158939517,1.,-1.47980070347096));
#28321=CARTESIAN_POINT('Ctrl Pts',(1.28435533880201,-1.,-1.4851881711891));
#28322=CARTESIAN_POINT('Ctrl Pts',(1.28435533880201,1.,-1.4851881711891));
#28323=CARTESIAN_POINT('Ctrl Pts',(1.2867467611644,-1.,-1.4906522831278));
#28324=CARTESIAN_POINT('Ctrl Pts',(1.2867467611644,1.,-1.4906522831278));
#28325=CARTESIAN_POINT('Ctrl Pts',(1.28911506584254,-1.,-1.49618896881754));
#28326=CARTESIAN_POINT('Ctrl Pts',(1.28911506584254,1.,-1.49618896881754));
#28327=CARTESIAN_POINT('Ctrl Pts',(1.29145022885181,-1.,-1.50178230149776));
#28328=CARTESIAN_POINT('Ctrl Pts',(1.29145022885181,1.,-1.50178230149776));
#28329=CARTESIAN_POINT('Ctrl Pts',(1.29373841372842,-1.,-1.50741159078365));
#28330=CARTESIAN_POINT('Ctrl Pts',(1.29373841372842,1.,-1.50741159078365));
#28331=CARTESIAN_POINT('Ctrl Pts',(1.29596850710509,-1.,-1.51305994241402));
#28332=CARTESIAN_POINT('Ctrl Pts',(1.29596850710509,1.,-1.51305994241402));
#28333=CARTESIAN_POINT('Ctrl Pts',(1.29813791800747,-1.,-1.51872184912724));
#28334=CARTESIAN_POINT('Ctrl Pts',(1.29813791800747,1.,-1.51872184912724));
#28335=CARTESIAN_POINT('Ctrl Pts',(1.30024984366328,-1.,-1.52439957861062));
#28336=CARTESIAN_POINT('Ctrl Pts',(1.30024984366328,1.,-1.52439957861062));
#28337=CARTESIAN_POINT('Ctrl Pts',(1.30231064395568,-1.,-1.53009970283891));
#28338=CARTESIAN_POINT('Ctrl Pts',(1.30231064395568,1.,-1.53009970283891));
#28339=CARTESIAN_POINT('Ctrl Pts',(1.30432735639489,-1.,-1.53582981268977));
#28340=CARTESIAN_POINT('Ctrl Pts',(1.30432735639489,1.,-1.53582981268977));
#28341=CARTESIAN_POINT('Ctrl Pts',(1.30630475189556,-1.,-1.54159462645432));
#28342=CARTESIAN_POINT('Ctrl Pts',(1.30630475189556,1.,-1.54159462645432));
#28343=CARTESIAN_POINT('Ctrl Pts',(1.30824393907473,-1.,-1.54739413957185));
#28344=CARTESIAN_POINT('Ctrl Pts',(1.30824393907473,1.,-1.54739413957185));
#28345=CARTESIAN_POINT('Ctrl Pts',(1.31014393684222,-1.,-1.55322568759481));
#28346=CARTESIAN_POINT('Ctrl Pts',(1.31014393684222,1.,-1.55322568759481));
#28347=CARTESIAN_POINT('Ctrl Pts',(1.31200264341696,-1.,-1.55908521254821));
#28348=CARTESIAN_POINT('Ctrl Pts',(1.31200264341696,1.,-1.55908521254821));
#28349=CARTESIAN_POINT('Ctrl Pts',(1.31381795281002,-1.,-1.56496872402353));
#28350=CARTESIAN_POINT('Ctrl Pts',(1.31381795281002,1.,-1.56496872402353));
#28351=CARTESIAN_POINT('Ctrl Pts',(1.31558903860016,-1.,-1.57087397835723));
#28352=CARTESIAN_POINT('Ctrl Pts',(1.31558903860016,1.,-1.57087397835723));
#28353=CARTESIAN_POINT('Ctrl Pts',(1.31731642317187,-1.,-1.5768005650559));
#28354=CARTESIAN_POINT('Ctrl Pts',(1.31731642317187,1.,-1.5768005650559));
#28355=CARTESIAN_POINT('Ctrl Pts',(1.31900135021432,-1.,-1.58274907898834));
#28356=CARTESIAN_POINT('Ctrl Pts',(1.31900135021432,1.,-1.58274907898834));
#28357=CARTESIAN_POINT('Ctrl Pts',(1.32064537110892,-1.,-1.58872057258245));
#28358=CARTESIAN_POINT('Ctrl Pts',(1.32064537110892,1.,-1.58872057258245));
#28359=CARTESIAN_POINT('Ctrl Pts',(1.32224985747682,-1.,-1.59471591079403));
#28360=CARTESIAN_POINT('Ctrl Pts',(1.32224985747682,1.,-1.59471591079403));
#28361=CARTESIAN_POINT('Ctrl Pts',(1.32381550858256,-1.,-1.60073511858687));
#28362=CARTESIAN_POINT('Ctrl Pts',(1.32381550858256,1.,-1.60073511858687));
#28363=CARTESIAN_POINT('Ctrl Pts',(1.32534250785782,-1.,-1.60677758290954));
#28364=CARTESIAN_POINT('Ctrl Pts',(1.32534250785782,1.,-1.60677758290954));
#28365=CARTESIAN_POINT('Ctrl Pts',(1.32683074483356,-1.,-1.6128423401575));
#28366=CARTESIAN_POINT('Ctrl Pts',(1.32683074483356,1.,-1.6128423401575));
#28367=CARTESIAN_POINT('Ctrl Pts',(1.32828000610449,-1.,-1.61892832270724));
#28368=CARTESIAN_POINT('Ctrl Pts',(1.32828000610449,1.,-1.61892832270724));
#28369=CARTESIAN_POINT('Ctrl Pts',(1.3296901950568,-1.,-1.62503464209797));
#28370=CARTESIAN_POINT('Ctrl Pts',(1.3296901950568,1.,-1.62503464209797));
#28371=CARTESIAN_POINT('Ctrl Pts',(1.33106149345645,-1.,-1.63116079730923));
#28372=CARTESIAN_POINT('Ctrl Pts',(1.33106149345645,1.,-1.63116079730923));
#28373=CARTESIAN_POINT('Ctrl Pts',(1.33239425103724,-1.,-1.63730653475089));
#28374=CARTESIAN_POINT('Ctrl Pts',(1.33239425103724,1.,-1.63730653475089));
#28375=CARTESIAN_POINT('Ctrl Pts',(1.33368890676572,-1.,-1.6434717485603));
#28376=CARTESIAN_POINT('Ctrl Pts',(1.33368890676572,1.,-1.6434717485603));
#28377=CARTESIAN_POINT('Ctrl Pts',(1.33494590467993,-1.,-1.6496563728683));
#28378=CARTESIAN_POINT('Ctrl Pts',(1.33494590467993,1.,-1.6496563728683));
#28379=CARTESIAN_POINT('Ctrl Pts',(1.33616559745172,-1.,-1.65586025952593));
#28380=CARTESIAN_POINT('Ctrl Pts',(1.33616559745172,1.,-1.65586025952593));
#28381=CARTESIAN_POINT('Ctrl Pts',(1.33734820885262,-1.,-1.66208312541983));
#28382=CARTESIAN_POINT('Ctrl Pts',(1.33734820885262,1.,-1.66208312541983));
#28383=CARTESIAN_POINT('Ctrl Pts',(1.33849388654388,-1.,-1.66832460783989));
#28384=CARTESIAN_POINT('Ctrl Pts',(1.33849388654388,1.,-1.66832460783989));
#28385=CARTESIAN_POINT('Ctrl Pts',(1.3396027347034,-1.,-1.67458429426086));
#28386=CARTESIAN_POINT('Ctrl Pts',(1.3396027347034,1.,-1.67458429426086));
#28387=CARTESIAN_POINT('Ctrl Pts',(1.34067485185203,-1.,-1.68086176030362));
#28388=CARTESIAN_POINT('Ctrl Pts',(1.34067485185203,1.,-1.68086176030362));
#28389=CARTESIAN_POINT('Ctrl Pts',(1.341710374848,-1.,-1.68715660868764));
#28390=CARTESIAN_POINT('Ctrl Pts',(1.341710374848,1.,-1.68715660868764));
#28391=CARTESIAN_POINT('Ctrl Pts',(1.34270948206319,-1.,-1.6934684849687));
#28392=CARTESIAN_POINT('Ctrl Pts',(1.34270948206319,1.,-1.6934684849687));
#28393=CARTESIAN_POINT('Ctrl Pts',(1.34367237124483,-1.,-1.69979707754427));
#28394=CARTESIAN_POINT('Ctrl Pts',(1.34367237124483,1.,-1.69979707754427));
#28395=CARTESIAN_POINT('Ctrl Pts',(1.34459924533831,-1.,-1.70614212266738));
#28396=CARTESIAN_POINT('Ctrl Pts',(1.34459924533831,1.,-1.70614212266738));
#28397=CARTESIAN_POINT('Ctrl Pts',(1.34549029589416,-1.,-1.71250340686822));
#28398=CARTESIAN_POINT('Ctrl Pts',(1.34549029589416,1.,-1.71250340686822));
#28399=CARTESIAN_POINT('Ctrl Pts',(1.34634568653227,-1.,-1.7188807715049));
#28400=CARTESIAN_POINT('Ctrl Pts',(1.34634568653227,1.,-1.7188807715049));
#28401=CARTESIAN_POINT('Ctrl Pts',(1.34716554819527,-1.,-1.72527410680674));
#28402=CARTESIAN_POINT('Ctrl Pts',(1.34716554819527,1.,-1.72527410680674));
#28403=CARTESIAN_POINT('Ctrl Pts',(1.34779309152035,-1.,-1.7304014965394));
#28404=CARTESIAN_POINT('Ctrl Pts',(1.34779309152035,1.,-1.7304014965394));
#28405=CARTESIAN_POINT('Ctrl Pts',(1.34824783112887,-1.,-1.73425417885907));
#28406=CARTESIAN_POINT('Ctrl Pts',(1.34824783112887,1.,-1.73425417885907));
#28407=CARTESIAN_POINT('Ctrl Pts',(1.34854391898045,-1.,-1.73682580585691));
#28408=CARTESIAN_POINT('Ctrl Pts',(1.34854391898045,1.,-1.73682580585691));
#28409=CARTESIAN_POINT('Ctrl Pts',(1.34869019493419,-1.,-1.73811241238545));
#28410=CARTESIAN_POINT('Ctrl Pts',(1.34869019493419,1.,-1.73811241238545));
#28411=CARTESIAN_POINT('',(1.15624053661742,1.,-1.31362392696032));
#28412=CARTESIAN_POINT('Ctrl Pts',(1.15624053661742,1.,-1.31362392696032));
#28413=CARTESIAN_POINT('Ctrl Pts',(1.15950888730809,1.,-1.31722977216397));
#28414=CARTESIAN_POINT('Ctrl Pts',(1.16589330093588,1.,-1.32428080721772));
#28415=CARTESIAN_POINT('Ctrl Pts',(1.17501305789857,1.,-1.33437539347008));
#28416=CARTESIAN_POINT('Ctrl Pts',(1.18625865667441,1.,-1.34687054001093));
#28417=CARTESIAN_POINT('Ctrl Pts',(1.1987959077932,1.,-1.36088705043885));
#28418=CARTESIAN_POINT('Ctrl Pts',(1.20982812925645,1.,-1.37331915607905));
#28419=CARTESIAN_POINT('Ctrl Pts',(1.21938737280852,1.,-1.38420564527715));
#28420=CARTESIAN_POINT('Ctrl Pts',(1.22752961899387,1.,-1.39361389568796));
#28421=CARTESIAN_POINT('Ctrl Pts',(1.23434087290423,1.,-1.40164708206106));
#28422=CARTESIAN_POINT('Ctrl Pts',(1.23994455029534,1.,-1.40845295531283));
#28423=CARTESIAN_POINT('Ctrl Pts',(1.24450600513056,1.,-1.41422913175179));
#28424=CARTESIAN_POINT('Ctrl Pts',(1.24824430986571,1.,-1.41923722596025));
#28425=CARTESIAN_POINT('Ctrl Pts',(1.2514145557001,1.,-1.42378102115575));
#28426=CARTESIAN_POINT('Ctrl Pts',(1.25426945222639,1.,-1.42815938799387));
#28427=CARTESIAN_POINT('Ctrl Pts',(1.25702687965755,1.,-1.43262645609691));
#28428=CARTESIAN_POINT('Ctrl Pts',(1.25983531012005,1.,-1.43734919180848));
#28429=CARTESIAN_POINT('Ctrl Pts',(1.26273903323858,1.,-1.44236470511303));
#28430=CARTESIAN_POINT('Ctrl Pts',(1.26570925118868,1.,-1.44761985001662));
#28431=CARTESIAN_POINT('Ctrl Pts',(1.2686778680489,1.,-1.45301422764247));
#28432=CARTESIAN_POINT('Ctrl Pts',(1.27156805265289,1.,-1.45843906294697));
#28433=CARTESIAN_POINT('Ctrl Pts',(1.27433119897822,1.,-1.46382431332476));
#28434=CARTESIAN_POINT('Ctrl Pts',(1.27696414831089,1.,-1.46916035917133));
#28435=CARTESIAN_POINT('Ctrl Pts',(1.2794891824849,1.,-1.4744717526707));
#28436=CARTESIAN_POINT('Ctrl Pts',(1.28194158939517,1.,-1.47980070347096));
#28437=CARTESIAN_POINT('Ctrl Pts',(1.28435533880201,1.,-1.4851881711891));
#28438=CARTESIAN_POINT('Ctrl Pts',(1.2867467611644,1.,-1.4906522831278));
#28439=CARTESIAN_POINT('Ctrl Pts',(1.28911506584254,1.,-1.49618896881754));
#28440=CARTESIAN_POINT('Ctrl Pts',(1.29145022885181,1.,-1.50178230149776));
#28441=CARTESIAN_POINT('Ctrl Pts',(1.29373841372842,1.,-1.50741159078365));
#28442=CARTESIAN_POINT('Ctrl Pts',(1.29596850710509,1.,-1.51305994241402));
#28443=CARTESIAN_POINT('Ctrl Pts',(1.29813791800747,1.,-1.51872184912724));
#28444=CARTESIAN_POINT('Ctrl Pts',(1.30024984366328,1.,-1.52439957861062));
#28445=CARTESIAN_POINT('Ctrl Pts',(1.30231064395568,1.,-1.53009970283891));
#28446=CARTESIAN_POINT('Ctrl Pts',(1.30432735639489,1.,-1.53582981268977));
#28447=CARTESIAN_POINT('Ctrl Pts',(1.30630475189556,1.,-1.54159462645432));
#28448=CARTESIAN_POINT('Ctrl Pts',(1.30824393907473,1.,-1.54739413957185));
#28449=CARTESIAN_POINT('Ctrl Pts',(1.31014393684222,1.,-1.55322568759481));
#28450=CARTESIAN_POINT('Ctrl Pts',(1.31200264341696,1.,-1.55908521254821));
#28451=CARTESIAN_POINT('Ctrl Pts',(1.31381795281002,1.,-1.56496872402353));
#28452=CARTESIAN_POINT('Ctrl Pts',(1.31558903860016,1.,-1.57087397835723));
#28453=CARTESIAN_POINT('Ctrl Pts',(1.31731642317187,1.,-1.5768005650559));
#28454=CARTESIAN_POINT('Ctrl Pts',(1.31900135021432,1.,-1.58274907898834));
#28455=CARTESIAN_POINT('Ctrl Pts',(1.32064537110892,1.,-1.58872057258245));
#28456=CARTESIAN_POINT('Ctrl Pts',(1.32224985747682,1.,-1.59471591079403));
#28457=CARTESIAN_POINT('Ctrl Pts',(1.32381550858256,1.,-1.60073511858687));
#28458=CARTESIAN_POINT('Ctrl Pts',(1.32534250785782,1.,-1.60677758290954));
#28459=CARTESIAN_POINT('Ctrl Pts',(1.32683074483356,1.,-1.6128423401575));
#28460=CARTESIAN_POINT('Ctrl Pts',(1.32828000610449,1.,-1.61892832270724));
#28461=CARTESIAN_POINT('Ctrl Pts',(1.3296901950568,1.,-1.62503464209797));
#28462=CARTESIAN_POINT('Ctrl Pts',(1.33106149345645,1.,-1.63116079730923));
#28463=CARTESIAN_POINT('Ctrl Pts',(1.33239425103724,1.,-1.63730653475089));
#28464=CARTESIAN_POINT('Ctrl Pts',(1.33368890676572,1.,-1.6434717485603));
#28465=CARTESIAN_POINT('Ctrl Pts',(1.33494590467993,1.,-1.6496563728683));
#28466=CARTESIAN_POINT('Ctrl Pts',(1.33616559745172,1.,-1.65586025952593));
#28467=CARTESIAN_POINT('Ctrl Pts',(1.33734820885262,1.,-1.66208312541983));
#28468=CARTESIAN_POINT('Ctrl Pts',(1.33849388654388,1.,-1.66832460783989));
#28469=CARTESIAN_POINT('Ctrl Pts',(1.3396027347034,1.,-1.67458429426086));
#28470=CARTESIAN_POINT('Ctrl Pts',(1.34067485185203,1.,-1.68086176030362));
#28471=CARTESIAN_POINT('Ctrl Pts',(1.341710374848,1.,-1.68715660868764));
#28472=CARTESIAN_POINT('Ctrl Pts',(1.34270948206319,1.,-1.6934684849687));
#28473=CARTESIAN_POINT('Ctrl Pts',(1.34367237124483,1.,-1.69979707754427));
#28474=CARTESIAN_POINT('Ctrl Pts',(1.34459924533831,1.,-1.70614212266738));
#28475=CARTESIAN_POINT('Ctrl Pts',(1.34549029589416,1.,-1.71250340686822));
#28476=CARTESIAN_POINT('Ctrl Pts',(1.34634568653227,1.,-1.7188807715049));
#28477=CARTESIAN_POINT('Ctrl Pts',(1.34716554819527,1.,-1.72527410680674));
#28478=CARTESIAN_POINT('Ctrl Pts',(1.34779309152035,1.,-1.7304014965394));
#28479=CARTESIAN_POINT('Ctrl Pts',(1.34824783112887,1.,-1.73425417885907));
#28480=CARTESIAN_POINT('Ctrl Pts',(1.34854391898045,1.,-1.73682580585691));
#28481=CARTESIAN_POINT('Ctrl Pts',(1.34869019493419,1.,-1.73811241238545));
#28482=CARTESIAN_POINT('',(1.15624053661742,0.,-1.31362392696032));
#28483=CARTESIAN_POINT('Origin',(0.,0.,0.));
#28484=CARTESIAN_POINT('',(1.31362392696032,1.,-1.15624053661742));
#28485=CARTESIAN_POINT('Origin',(0.,1.,0.));
#28486=CARTESIAN_POINT('',(1.31362392696032,0.,-1.15624053661742));
#28487=CARTESIAN_POINT('Ctrl Pts',(1.73811241238545,-1.,-1.34869019493419));
#28488=CARTESIAN_POINT('Ctrl Pts',(1.73811241238545,1.,-1.34869019493419));
#28489=CARTESIAN_POINT('Ctrl Pts',(1.73682580585819,-1.,-1.34854391898145));
#28490=CARTESIAN_POINT('Ctrl Pts',(1.73682580585819,1.,-1.34854391898145));
#28491=CARTESIAN_POINT('Ctrl Pts',(1.73425417886254,-1.,-1.34824783113158));
#28492=CARTESIAN_POINT('Ctrl Pts',(1.73425417886254,1.,-1.34824783113158));
#28493=CARTESIAN_POINT('Ctrl Pts',(1.73040149654497,-1.,-1.3477930915247));
#28494=CARTESIAN_POINT('Ctrl Pts',(1.73040149654497,1.,-1.3477930915247));
#28495=CARTESIAN_POINT('Ctrl Pts',(1.72527410681298,-1.,-1.34716554820013));
#28496=CARTESIAN_POINT('Ctrl Pts',(1.72527410681298,1.,-1.34716554820013));
#28497=CARTESIAN_POINT('Ctrl Pts',(1.7188807715095,-1.,-1.34634568653586));
#28498=CARTESIAN_POINT('Ctrl Pts',(1.7188807715095,1.,-1.34634568653586));
#28499=CARTESIAN_POINT('Ctrl Pts',(1.71250340687011,-1.,-1.34549029589563));
#28500=CARTESIAN_POINT('Ctrl Pts',(1.71250340687011,1.,-1.34549029589563));
#28501=CARTESIAN_POINT('Ctrl Pts',(1.70614212266676,-1.,-1.34459924533783));
#28502=CARTESIAN_POINT('Ctrl Pts',(1.70614212266676,1.,-1.34459924533783));
#28503=CARTESIAN_POINT('Ctrl Pts',(1.69979707754221,-1.,-1.34367237124322));
#28504=CARTESIAN_POINT('Ctrl Pts',(1.69979707754221,1.,-1.34367237124322));
#28505=CARTESIAN_POINT('Ctrl Pts',(1.6934684849664,-1.,-1.34270948206139));
#28506=CARTESIAN_POINT('Ctrl Pts',(1.6934684849664,1.,-1.34270948206139));
#28507=CARTESIAN_POINT('Ctrl Pts',(1.68715660868602,-1.,-1.34171037484673));
#28508=CARTESIAN_POINT('Ctrl Pts',(1.68715660868602,1.,-1.34171037484673));
#28509=CARTESIAN_POINT('Ctrl Pts',(1.68086176030308,-1.,-1.3406748518516));
#28510=CARTESIAN_POINT('Ctrl Pts',(1.68086176030308,1.,-1.3406748518516));
#28511=CARTESIAN_POINT('Ctrl Pts',(1.67458429426126,-1.,-1.33960273470372));
#28512=CARTESIAN_POINT('Ctrl Pts',(1.67458429426126,1.,-1.33960273470372));
#28513=CARTESIAN_POINT('Ctrl Pts',(1.66832460784078,-1.,-1.33849388654458));
#28514=CARTESIAN_POINT('Ctrl Pts',(1.66832460784078,1.,-1.33849388654458));
#28515=CARTESIAN_POINT('Ctrl Pts',(1.66208312542073,-1.,-1.33734820885331));
#28516=CARTESIAN_POINT('Ctrl Pts',(1.66208312542073,1.,-1.33734820885331));
#28517=CARTESIAN_POINT('Ctrl Pts',(1.65586025952651,-1.,-1.33616559745217));
#28518=CARTESIAN_POINT('Ctrl Pts',(1.65586025952651,1.,-1.33616559745217));
#28519=CARTESIAN_POINT('Ctrl Pts',(1.64965637286843,-1.,-1.33494590468003));
#28520=CARTESIAN_POINT('Ctrl Pts',(1.64965637286843,1.,-1.33494590468003));
#28521=CARTESIAN_POINT('Ctrl Pts',(1.64347174856007,-1.,-1.33368890676554));
#28522=CARTESIAN_POINT('Ctrl Pts',(1.64347174856007,1.,-1.33368890676554));
#28523=CARTESIAN_POINT('Ctrl Pts',(1.63730653475049,-1.,-1.33239425103694));
#28524=CARTESIAN_POINT('Ctrl Pts',(1.63730653475049,1.,-1.33239425103694));
#28525=CARTESIAN_POINT('Ctrl Pts',(1.63116079730887,-1.,-1.33106149345618));
#28526=CARTESIAN_POINT('Ctrl Pts',(1.63116079730887,1.,-1.33106149345618));
#28527=CARTESIAN_POINT('Ctrl Pts',(1.62503464209777,-1.,-1.32969019505665));
#28528=CARTESIAN_POINT('Ctrl Pts',(1.62503464209777,1.,-1.32969019505665));
#28529=CARTESIAN_POINT('Ctrl Pts',(1.61892832270723,-1.,-1.32828000610448));
#28530=CARTESIAN_POINT('Ctrl Pts',(1.61892832270723,1.,-1.32828000610448));
#28531=CARTESIAN_POINT('Ctrl Pts',(1.61284234015762,-1.,-1.32683074483365));
#28532=CARTESIAN_POINT('Ctrl Pts',(1.61284234015762,1.,-1.32683074483365));
#28533=CARTESIAN_POINT('Ctrl Pts',(1.6067775829097,-1.,-1.32534250785794));
#28534=CARTESIAN_POINT('Ctrl Pts',(1.6067775829097,1.,-1.32534250785794));
#28535=CARTESIAN_POINT('Ctrl Pts',(1.600735118587,-1.,-1.32381550858266));
#28536=CARTESIAN_POINT('Ctrl Pts',(1.600735118587,1.,-1.32381550858266));
#28537=CARTESIAN_POINT('Ctrl Pts',(1.59471591079408,-1.,-1.32224985747686));
#28538=CARTESIAN_POINT('Ctrl Pts',(1.59471591079408,1.,-1.32224985747686));
#28539=CARTESIAN_POINT('Ctrl Pts',(1.58872057258244,-1.,-1.32064537110891));
#28540=CARTESIAN_POINT('Ctrl Pts',(1.58872057258244,1.,-1.32064537110891));
#28541=CARTESIAN_POINT('Ctrl Pts',(1.58274907898829,-1.,-1.31900135021428));
#28542=CARTESIAN_POINT('Ctrl Pts',(1.58274907898829,1.,-1.31900135021428));
#28543=CARTESIAN_POINT('Ctrl Pts',(1.57680056505585,-1.,-1.31731642317183));
#28544=CARTESIAN_POINT('Ctrl Pts',(1.57680056505585,1.,-1.31731642317183));
#28545=CARTESIAN_POINT('Ctrl Pts',(1.57087397835721,-1.,-1.31558903860015));
#28546=CARTESIAN_POINT('Ctrl Pts',(1.57087397835721,1.,-1.31558903860015));
#28547=CARTESIAN_POINT('Ctrl Pts',(1.56496872402352,-1.,-1.31381795281002));
#28548=CARTESIAN_POINT('Ctrl Pts',(1.56496872402352,1.,-1.31381795281002));
#28549=CARTESIAN_POINT('Ctrl Pts',(1.55908521254822,-1.,-1.31200264341696));
#28550=CARTESIAN_POINT('Ctrl Pts',(1.55908521254822,1.,-1.31200264341696));
#28551=CARTESIAN_POINT('Ctrl Pts',(1.55322568759481,-1.,-1.31014393684221));
#28552=CARTESIAN_POINT('Ctrl Pts',(1.55322568759481,1.,-1.31014393684221));
#28553=CARTESIAN_POINT('Ctrl Pts',(1.54739413957183,-1.,-1.30824393907471));
#28554=CARTESIAN_POINT('Ctrl Pts',(1.54739413957183,1.,-1.30824393907471));
#28555=CARTESIAN_POINT('Ctrl Pts',(1.54159462645428,-1.,-1.30630475189553));
#28556=CARTESIAN_POINT('Ctrl Pts',(1.54159462645428,1.,-1.30630475189553));
#28557=CARTESIAN_POINT('Ctrl Pts',(1.53582981268976,-1.,-1.30432735639487));
#28558=CARTESIAN_POINT('Ctrl Pts',(1.53582981268976,1.,-1.30432735639487));
#28559=CARTESIAN_POINT('Ctrl Pts',(1.53009970283893,-1.,-1.3023106439557));
#28560=CARTESIAN_POINT('Ctrl Pts',(1.53009970283893,1.,-1.3023106439557));
#28561=CARTESIAN_POINT('Ctrl Pts',(1.5243995786107,-1.,-1.30024984366334));
#28562=CARTESIAN_POINT('Ctrl Pts',(1.5243995786107,1.,-1.30024984366334));
#28563=CARTESIAN_POINT('Ctrl Pts',(1.51872184912735,-1.,-1.29813791800757));
#28564=CARTESIAN_POINT('Ctrl Pts',(1.51872184912735,1.,-1.29813791800757));
#28565=CARTESIAN_POINT('Ctrl Pts',(1.51305994241412,-1.,-1.29596850710518));
#28566=CARTESIAN_POINT('Ctrl Pts',(1.51305994241412,1.,-1.29596850710518));
#28567=CARTESIAN_POINT('Ctrl Pts',(1.50741159078367,-1.,-1.29373841372843));
#28568=CARTESIAN_POINT('Ctrl Pts',(1.50741159078367,1.,-1.29373841372843));
#28569=CARTESIAN_POINT('Ctrl Pts',(1.50178230149764,-1.,-1.29145022885171));
#28570=CARTESIAN_POINT('Ctrl Pts',(1.50178230149764,1.,-1.29145022885171));
#28571=CARTESIAN_POINT('Ctrl Pts',(1.49618896881729,-1.,-1.28911506584232));
#28572=CARTESIAN_POINT('Ctrl Pts',(1.49618896881729,1.,-1.28911506584232));
#28573=CARTESIAN_POINT('Ctrl Pts',(1.4906522831275,-1.,-1.28674676116415));
#28574=CARTESIAN_POINT('Ctrl Pts',(1.4906522831275,1.,-1.28674676116415));
#28575=CARTESIAN_POINT('Ctrl Pts',(1.48518817118891,-1.,-1.28435533880184));
#28576=CARTESIAN_POINT('Ctrl Pts',(1.48518817118891,1.,-1.28435533880184));
#28577=CARTESIAN_POINT('Ctrl Pts',(1.47980070347102,-1.,-1.28194158939522));
#28578=CARTESIAN_POINT('Ctrl Pts',(1.47980070347102,1.,-1.28194158939522));
#28579=CARTESIAN_POINT('Ctrl Pts',(1.4744717526711,-1.,-1.27948918248524));
#28580=CARTESIAN_POINT('Ctrl Pts',(1.4744717526711,1.,-1.27948918248524));
#28581=CARTESIAN_POINT('Ctrl Pts',(1.46916035917197,-1.,-1.27696414831144));
#28582=CARTESIAN_POINT('Ctrl Pts',(1.46916035917197,1.,-1.27696414831144));
#28583=CARTESIAN_POINT('Ctrl Pts',(1.4638243133254,-1.,-1.27433119897877));
#28584=CARTESIAN_POINT('Ctrl Pts',(1.4638243133254,1.,-1.27433119897877));
#28585=CARTESIAN_POINT('Ctrl Pts',(1.45843906294725,-1.,-1.27156805265312));
#28586=CARTESIAN_POINT('Ctrl Pts',(1.45843906294725,1.,-1.27156805265312));
#28587=CARTESIAN_POINT('Ctrl Pts',(1.45301422764205,-1.,-1.26867786804854));
#28588=CARTESIAN_POINT('Ctrl Pts',(1.45301422764205,1.,-1.26867786804854));
#28589=CARTESIAN_POINT('Ctrl Pts',(1.44761985001544,-1.,-1.26570925118767));
#28590=CARTESIAN_POINT('Ctrl Pts',(1.44761985001544,1.,-1.26570925118767));
#28591=CARTESIAN_POINT('Ctrl Pts',(1.44236470511145,-1.,-1.26273903323723));
#28592=CARTESIAN_POINT('Ctrl Pts',(1.44236470511145,1.,-1.26273903323723));
#28593=CARTESIAN_POINT('Ctrl Pts',(1.43734919180719,-1.,-1.25983531011894));
#28594=CARTESIAN_POINT('Ctrl Pts',(1.43734919180719,1.,-1.25983531011894));
#28595=CARTESIAN_POINT('Ctrl Pts',(1.43262645609679,-1.,-1.25702687965744));
#28596=CARTESIAN_POINT('Ctrl Pts',(1.43262645609679,1.,-1.25702687965744));
#28597=CARTESIAN_POINT('Ctrl Pts',(1.42815938799555,-1.,-1.25426945222783));
#28598=CARTESIAN_POINT('Ctrl Pts',(1.42815938799555,1.,-1.25426945222783));
#28599=CARTESIAN_POINT('Ctrl Pts',(1.42378102115911,-1.,-1.25141455570299));
#28600=CARTESIAN_POINT('Ctrl Pts',(1.42378102115911,1.,-1.25141455570299));
#28601=CARTESIAN_POINT('Ctrl Pts',(1.41923722596421,-1.,-1.24824430986911));
#28602=CARTESIAN_POINT('Ctrl Pts',(1.41923722596421,1.,-1.24824430986911));
#28603=CARTESIAN_POINT('Ctrl Pts',(1.41422913175437,-1.,-1.24450600513278));
#28604=CARTESIAN_POINT('Ctrl Pts',(1.41422913175437,1.,-1.24450600513278));
#28605=CARTESIAN_POINT('Ctrl Pts',(1.40845295531151,-1.,-1.23994455029421));
#28606=CARTESIAN_POINT('Ctrl Pts',(1.40845295531151,1.,-1.23994455029421));
#28607=CARTESIAN_POINT('Ctrl Pts',(1.40164708205345,-1.,-1.23434087289768));
#28608=CARTESIAN_POINT('Ctrl Pts',(1.40164708205345,1.,-1.23434087289768));
#28609=CARTESIAN_POINT('Ctrl Pts',(1.39361389567257,-1.,-1.22752961898063));
#28610=CARTESIAN_POINT('Ctrl Pts',(1.39361389567257,1.,-1.22752961898063));
#28611=CARTESIAN_POINT('Ctrl Pts',(1.38420564525391,-1.,-1.21938737278853));
#28612=CARTESIAN_POINT('Ctrl Pts',(1.38420564525391,1.,-1.21938737278853));
#28613=CARTESIAN_POINT('Ctrl Pts',(1.37331915604962,-1.,-1.20982812923113));
#28614=CARTESIAN_POINT('Ctrl Pts',(1.37331915604962,1.,-1.20982812923113));
#28615=CARTESIAN_POINT('Ctrl Pts',(1.36088705040677,-1.,-1.1987959077656));
#28616=CARTESIAN_POINT('Ctrl Pts',(1.36088705040677,1.,-1.1987959077656));
#28617=CARTESIAN_POINT('Ctrl Pts',(1.34687053998157,-1.,-1.18625865664915));
#28618=CARTESIAN_POINT('Ctrl Pts',(1.34687053998157,1.,-1.18625865664915));
#28619=CARTESIAN_POINT('Ctrl Pts',(1.33437539344842,-1.,-1.17501305787994));
#28620=CARTESIAN_POINT('Ctrl Pts',(1.33437539344842,1.,-1.17501305787994));
#28621=CARTESIAN_POINT('Ctrl Pts',(1.32428080720544,-1.,-1.16589330092532));
#28622=CARTESIAN_POINT('Ctrl Pts',(1.32428080720544,1.,-1.16589330092532));
#28623=CARTESIAN_POINT('Ctrl Pts',(1.3172297721596,-1.,-1.15950888730433));
#28624=CARTESIAN_POINT('Ctrl Pts',(1.3172297721596,1.,-1.15950888730433));
#28625=CARTESIAN_POINT('Ctrl Pts',(1.31362392696032,-1.,-1.15624053661742));
#28626=CARTESIAN_POINT('Ctrl Pts',(1.31362392696032,1.,-1.15624053661742));
#28627=CARTESIAN_POINT('',(1.73811241238545,1.,-1.34869019493419));
#28628=CARTESIAN_POINT('Ctrl Pts',(1.73811241238545,1.,-1.34869019493419));
#28629=CARTESIAN_POINT('Ctrl Pts',(1.73682580585819,1.,-1.34854391898145));
#28630=CARTESIAN_POINT('Ctrl Pts',(1.73425417886254,1.,-1.34824783113158));
#28631=CARTESIAN_POINT('Ctrl Pts',(1.73040149654497,1.,-1.3477930915247));
#28632=CARTESIAN_POINT('Ctrl Pts',(1.72527410681298,1.,-1.34716554820013));
#28633=CARTESIAN_POINT('Ctrl Pts',(1.7188807715095,1.,-1.34634568653586));
#28634=CARTESIAN_POINT('Ctrl Pts',(1.71250340687011,1.,-1.34549029589563));
#28635=CARTESIAN_POINT('Ctrl Pts',(1.70614212266676,1.,-1.34459924533783));
#28636=CARTESIAN_POINT('Ctrl Pts',(1.69979707754221,1.,-1.34367237124322));
#28637=CARTESIAN_POINT('Ctrl Pts',(1.6934684849664,1.,-1.34270948206139));
#28638=CARTESIAN_POINT('Ctrl Pts',(1.68715660868602,1.,-1.34171037484673));
#28639=CARTESIAN_POINT('Ctrl Pts',(1.68086176030308,1.,-1.3406748518516));
#28640=CARTESIAN_POINT('Ctrl Pts',(1.67458429426126,1.,-1.33960273470372));
#28641=CARTESIAN_POINT('Ctrl Pts',(1.66832460784078,1.,-1.33849388654458));
#28642=CARTESIAN_POINT('Ctrl Pts',(1.66208312542073,1.,-1.33734820885331));
#28643=CARTESIAN_POINT('Ctrl Pts',(1.65586025952651,1.,-1.33616559745217));
#28644=CARTESIAN_POINT('Ctrl Pts',(1.64965637286843,1.,-1.33494590468003));
#28645=CARTESIAN_POINT('Ctrl Pts',(1.64347174856007,1.,-1.33368890676554));
#28646=CARTESIAN_POINT('Ctrl Pts',(1.63730653475049,1.,-1.33239425103694));
#28647=CARTESIAN_POINT('Ctrl Pts',(1.63116079730887,1.,-1.33106149345618));
#28648=CARTESIAN_POINT('Ctrl Pts',(1.62503464209777,1.,-1.32969019505665));
#28649=CARTESIAN_POINT('Ctrl Pts',(1.61892832270723,1.,-1.32828000610448));
#28650=CARTESIAN_POINT('Ctrl Pts',(1.61284234015762,1.,-1.32683074483365));
#28651=CARTESIAN_POINT('Ctrl Pts',(1.6067775829097,1.,-1.32534250785794));
#28652=CARTESIAN_POINT('Ctrl Pts',(1.600735118587,1.,-1.32381550858266));
#28653=CARTESIAN_POINT('Ctrl Pts',(1.59471591079408,1.,-1.32224985747686));
#28654=CARTESIAN_POINT('Ctrl Pts',(1.58872057258244,1.,-1.32064537110891));
#28655=CARTESIAN_POINT('Ctrl Pts',(1.58274907898829,1.,-1.31900135021428));
#28656=CARTESIAN_POINT('Ctrl Pts',(1.57680056505585,1.,-1.31731642317183));
#28657=CARTESIAN_POINT('Ctrl Pts',(1.57087397835721,1.,-1.31558903860015));
#28658=CARTESIAN_POINT('Ctrl Pts',(1.56496872402352,1.,-1.31381795281002));
#28659=CARTESIAN_POINT('Ctrl Pts',(1.55908521254822,1.,-1.31200264341696));
#28660=CARTESIAN_POINT('Ctrl Pts',(1.55322568759481,1.,-1.31014393684221));
#28661=CARTESIAN_POINT('Ctrl Pts',(1.54739413957183,1.,-1.30824393907471));
#28662=CARTESIAN_POINT('Ctrl Pts',(1.54159462645428,1.,-1.30630475189553));
#28663=CARTESIAN_POINT('Ctrl Pts',(1.53582981268976,1.,-1.30432735639487));
#28664=CARTESIAN_POINT('Ctrl Pts',(1.53009970283893,1.,-1.3023106439557));
#28665=CARTESIAN_POINT('Ctrl Pts',(1.5243995786107,1.,-1.30024984366334));
#28666=CARTESIAN_POINT('Ctrl Pts',(1.51872184912735,1.,-1.29813791800757));
#28667=CARTESIAN_POINT('Ctrl Pts',(1.51305994241412,1.,-1.29596850710518));
#28668=CARTESIAN_POINT('Ctrl Pts',(1.50741159078367,1.,-1.29373841372843));
#28669=CARTESIAN_POINT('Ctrl Pts',(1.50178230149764,1.,-1.29145022885171));
#28670=CARTESIAN_POINT('Ctrl Pts',(1.49618896881729,1.,-1.28911506584232));
#28671=CARTESIAN_POINT('Ctrl Pts',(1.4906522831275,1.,-1.28674676116415));
#28672=CARTESIAN_POINT('Ctrl Pts',(1.48518817118891,1.,-1.28435533880184));
#28673=CARTESIAN_POINT('Ctrl Pts',(1.47980070347102,1.,-1.28194158939522));
#28674=CARTESIAN_POINT('Ctrl Pts',(1.4744717526711,1.,-1.27948918248524));
#28675=CARTESIAN_POINT('Ctrl Pts',(1.46916035917197,1.,-1.27696414831144));
#28676=CARTESIAN_POINT('Ctrl Pts',(1.4638243133254,1.,-1.27433119897877));
#28677=CARTESIAN_POINT('Ctrl Pts',(1.45843906294725,1.,-1.27156805265312));
#28678=CARTESIAN_POINT('Ctrl Pts',(1.45301422764205,1.,-1.26867786804854));
#28679=CARTESIAN_POINT('Ctrl Pts',(1.44761985001544,1.,-1.26570925118767));
#28680=CARTESIAN_POINT('Ctrl Pts',(1.44236470511145,1.,-1.26273903323723));
#28681=CARTESIAN_POINT('Ctrl Pts',(1.43734919180719,1.,-1.25983531011894));
#28682=CARTESIAN_POINT('Ctrl Pts',(1.43262645609679,1.,-1.25702687965744));
#28683=CARTESIAN_POINT('Ctrl Pts',(1.42815938799555,1.,-1.25426945222783));
#28684=CARTESIAN_POINT('Ctrl Pts',(1.42378102115911,1.,-1.25141455570299));
#28685=CARTESIAN_POINT('Ctrl Pts',(1.41923722596421,1.,-1.24824430986911));
#28686=CARTESIAN_POINT('Ctrl Pts',(1.41422913175437,1.,-1.24450600513278));
#28687=CARTESIAN_POINT('Ctrl Pts',(1.40845295531151,1.,-1.23994455029421));
#28688=CARTESIAN_POINT('Ctrl Pts',(1.40164708205345,1.,-1.23434087289768));
#28689=CARTESIAN_POINT('Ctrl Pts',(1.39361389567257,1.,-1.22752961898063));
#28690=CARTESIAN_POINT('Ctrl Pts',(1.38420564525391,1.,-1.21938737278853));
#28691=CARTESIAN_POINT('Ctrl Pts',(1.37331915604962,1.,-1.20982812923113));
#28692=CARTESIAN_POINT('Ctrl Pts',(1.36088705040677,1.,-1.1987959077656));
#28693=CARTESIAN_POINT('Ctrl Pts',(1.34687053998157,1.,-1.18625865664915));
#28694=CARTESIAN_POINT('Ctrl Pts',(1.33437539344842,1.,-1.17501305787994));
#28695=CARTESIAN_POINT('Ctrl Pts',(1.32428080720544,1.,-1.16589330092532));
#28696=CARTESIAN_POINT('Ctrl Pts',(1.3172297721596,1.,-1.15950888730433));
#28697=CARTESIAN_POINT('Ctrl Pts',(1.31362392696032,1.,-1.15624053661742));
#28698=CARTESIAN_POINT('',(1.73811241238545,0.,-1.34869019493419));
#28699=CARTESIAN_POINT('Origin',(1.81978687191668,0.,-1.23627494547115));
#28700=CARTESIAN_POINT('',(1.81978687191668,1.,-1.23627494547115));
#28701=CARTESIAN_POINT('',(1.73811241238545,1.,-1.34869019493419));
#28702=CARTESIAN_POINT('',(1.81978687191668,0.,-1.23627494547115));
#28703=CARTESIAN_POINT('Ctrl Pts',(1.5055822144029,-1.,-0.892032620296855));
#28704=CARTESIAN_POINT('Ctrl Pts',(1.5055822144029,1.,-0.892032620296855));
#28705=CARTESIAN_POINT('Ctrl Pts',(1.50980486807181,-1.,-0.894452006967538));
#28706=CARTESIAN_POINT('Ctrl Pts',(1.50980486807181,1.,-0.894452006967538));
#28707=CARTESIAN_POINT('Ctrl Pts',(1.51805569591479,-1.,-0.89918504749193));
#28708=CARTESIAN_POINT('Ctrl Pts',(1.51805569591479,1.,-0.89918504749193));
#28709=CARTESIAN_POINT('Ctrl Pts',(1.52984849890434,-1.,-0.905967409640499));
#28710=CARTESIAN_POINT('Ctrl Pts',(1.52984849890434,1.,-0.905967409640499));
#28711=CARTESIAN_POINT('Ctrl Pts',(1.54440491152807,-1.,-0.91437591904658));
#28712=CARTESIAN_POINT('Ctrl Pts',(1.54440491152807,1.,-0.91437591904658));
#28713=CARTESIAN_POINT('Ctrl Pts',(1.56065988582509,-1.,-0.923832188966322));
#28714=CARTESIAN_POINT('Ctrl Pts',(1.56065988582509,1.,-0.923832188966322));
#28715=CARTESIAN_POINT('Ctrl Pts',(1.57499388385561,-1.,-0.932246680128849));
#28716=CARTESIAN_POINT('Ctrl Pts',(1.57499388385561,1.,-0.932246680128849));
#28717=CARTESIAN_POINT('Ctrl Pts',(1.58744937489796,-1.,-0.939646377909319));
#28718=CARTESIAN_POINT('Ctrl Pts',(1.58744937489796,1.,-0.939646377909319));
#28719=CARTESIAN_POINT('Ctrl Pts',(1.59810042045408,-1.,-0.946078063325796));
#28720=CARTESIAN_POINT('Ctrl Pts',(1.59810042045408,1.,-0.946078063325796));
#28721=CARTESIAN_POINT('Ctrl Pts',(1.60706069897794,-1.,-0.951613284361248));
#28722=CARTESIAN_POINT('Ctrl Pts',(1.60706069897794,1.,-0.951613284361248));
#28723=CARTESIAN_POINT('Ctrl Pts',(1.61449324337233,-1.,-0.956354422921573));
#28724=CARTESIAN_POINT('Ctrl Pts',(1.61449324337233,1.,-0.956354422921573));
#28725=CARTESIAN_POINT('Ctrl Pts',(1.62061638139929,-1.,-0.960438326099958));
#28726=CARTESIAN_POINT('Ctrl Pts',(1.62061638139929,1.,-0.960438326099958));
#28727=CARTESIAN_POINT('Ctrl Pts',(1.6257193066974,-1.,-0.964046107037821));
#28728=CARTESIAN_POINT('Ctrl Pts',(1.6257193066974,1.,-0.964046107037821));
#28729=CARTESIAN_POINT('Ctrl Pts',(1.63013849959083,-1.,-0.967387853228041));
#28730=CARTESIAN_POINT('Ctrl Pts',(1.63013849959083,1.,-0.967387853228041));
#28731=CARTESIAN_POINT('Ctrl Pts',(1.63420665729609,-1.,-0.970669715996356));
#28732=CARTESIAN_POINT('Ctrl Pts',(1.63420665729609,1.,-0.970669715996356));
#28733=CARTESIAN_POINT('Ctrl Pts',(1.63820952658157,-1.,-0.974066058287501));
#28734=CARTESIAN_POINT('Ctrl Pts',(1.63820952658157,1.,-0.974066058287501));
#28735=CARTESIAN_POINT('Ctrl Pts',(1.64233990826831,-1.,-0.977689794120297));
#28736=CARTESIAN_POINT('Ctrl Pts',(1.64233990826831,1.,-0.977689794120297));
#28737=CARTESIAN_POINT('Ctrl Pts',(1.64665139190834,-1.,-0.981562530940574));
#28738=CARTESIAN_POINT('Ctrl Pts',(1.64665139190834,1.,-0.981562530940574));
#28739=CARTESIAN_POINT('Ctrl Pts',(1.6511001661277,-1.,-0.985642622921626));
#28740=CARTESIAN_POINT('Ctrl Pts',(1.6511001661277,1.,-0.985642622921626));
#28741=CARTESIAN_POINT('Ctrl Pts',(1.65559044289746,-1.,-0.98985562785445));
#28742=CARTESIAN_POINT('Ctrl Pts',(1.65559044289746,1.,-0.98985562785445));
#28743=CARTESIAN_POINT('Ctrl Pts',(1.66001553809916,-1.,-0.994121836661116));
#28744=CARTESIAN_POINT('Ctrl Pts',(1.66001553809916,1.,-0.994121836661116));
#28745=CARTESIAN_POINT('Ctrl Pts',(1.66430758030304,-1.,-0.998389654952317));
#28746=CARTESIAN_POINT('Ctrl Pts',(1.66430758030304,1.,-0.998389654952317));
#28747=CARTESIAN_POINT('Ctrl Pts',(1.66846059277231,-1.,-1.00265091003682));
#28748=CARTESIAN_POINT('Ctrl Pts',(1.66846059277231,1.,-1.00265091003682));
#28749=CARTESIAN_POINT('Ctrl Pts',(1.67250335383248,-1.,-1.00692206696387));
#28750=CARTESIAN_POINT('Ctrl Pts',(1.67250335383248,1.,-1.00692206696387));
#28751=CARTESIAN_POINT('Ctrl Pts',(1.67648246776457,-1.,-1.01123236493507));
#28752=CARTESIAN_POINT('Ctrl Pts',(1.67648246776457,1.,-1.01123236493507));
#28753=CARTESIAN_POINT('Ctrl Pts',(1.6804428989482,-1.,-1.01561026162787));
#28754=CARTESIAN_POINT('Ctrl Pts',(1.6804428989482,1.,-1.01561026162787));
#28755=CARTESIAN_POINT('Ctrl Pts',(1.68440578021739,-1.,-1.02006795074222));
#28756=CARTESIAN_POINT('Ctrl Pts',(1.68440578021739,1.,-1.02006795074222));
#28757=CARTESIAN_POINT('Ctrl Pts',(1.68836910178475,-1.,-1.02460180535272));
#28758=CARTESIAN_POINT('Ctrl Pts',(1.68836910178475,1.,-1.02460180535272));
#28759=CARTESIAN_POINT('Ctrl Pts',(1.69231840863471,-1.,-1.02919977579155));
#28760=CARTESIAN_POINT('Ctrl Pts',(1.69231840863471,1.,-1.02919977579155));
#28761=CARTESIAN_POINT('Ctrl Pts',(1.69623414782769,-1.,-1.03384646003587));
#28762=CARTESIAN_POINT('Ctrl Pts',(1.69623414782769,1.,-1.03384646003587));
#28763=CARTESIAN_POINT('Ctrl Pts',(1.70010052930951,-1.,-1.03852922490782));
#28764=CARTESIAN_POINT('Ctrl Pts',(1.70010052930951,1.,-1.03852922490782));
#28765=CARTESIAN_POINT('Ctrl Pts',(1.70391338707969,-1.,-1.04324363334546));
#28766=CARTESIAN_POINT('Ctrl Pts',(1.70391338707969,1.,-1.04324363334546));
#28767=CARTESIAN_POINT('Ctrl Pts',(1.70767646263641,-1.,-1.0479908540499));
#28768=CARTESIAN_POINT('Ctrl Pts',(1.70767646263641,1.,-1.0479908540499));
#28769=CARTESIAN_POINT('Ctrl Pts',(1.71139783543986,-1.,-1.05277517202854));
#28770=CARTESIAN_POINT('Ctrl Pts',(1.71139783543986,1.,-1.05277517202854));
#28771=CARTESIAN_POINT('Ctrl Pts',(1.71508654427022,-1.,-1.05760163192481));
#28772=CARTESIAN_POINT('Ctrl Pts',(1.71508654427022,1.,-1.05760163192481));
#28773=CARTESIAN_POINT('Ctrl Pts',(1.71874858456908,-1.,-1.0624732468065));
#28774=CARTESIAN_POINT('Ctrl Pts',(1.71874858456908,1.,-1.0624732468065));
#28775=CARTESIAN_POINT('Ctrl Pts',(1.72238500928456,-1.,-1.06738966975463));
#28776=CARTESIAN_POINT('Ctrl Pts',(1.72238500928456,1.,-1.06738966975463));
#28777=CARTESIAN_POINT('Ctrl Pts',(1.72599406198489,-1.,-1.07234866990252));
#28778=CARTESIAN_POINT('Ctrl Pts',(1.72599406198489,1.,-1.07234866990252));
#28779=CARTESIAN_POINT('Ctrl Pts',(1.72957248977424,-1.,-1.0773470373727));
#28780=CARTESIAN_POINT('Ctrl Pts',(1.72957248977424,1.,-1.0773470373727));
#28781=CARTESIAN_POINT('Ctrl Pts',(1.73311705663407,-1.,-1.08238162784749));
#28782=CARTESIAN_POINT('Ctrl Pts',(1.73311705663407,1.,-1.08238162784749));
#28783=CARTESIAN_POINT('Ctrl Pts',(1.73662628326093,-1.,-1.08745056285429));
#28784=CARTESIAN_POINT('Ctrl Pts',(1.73662628326093,1.,-1.08745056285429));
#28785=CARTESIAN_POINT('Ctrl Pts',(1.74010053962252,-1.,-1.09255329056496));
#28786=CARTESIAN_POINT('Ctrl Pts',(1.74010053962252,1.,-1.09255329056496));
#28787=CARTESIAN_POINT('Ctrl Pts',(1.74354119236212,-1.,-1.09768999241229));
#28788=CARTESIAN_POINT('Ctrl Pts',(1.74354119236212,1.,-1.09768999241229));
#28789=CARTESIAN_POINT('Ctrl Pts',(1.74695004214924,-1.,-1.10286118991144));
#28790=CARTESIAN_POINT('Ctrl Pts',(1.74695004214924,1.,-1.10286118991144));
#28791=CARTESIAN_POINT('Ctrl Pts',(1.75032866075914,-1.,-1.10806728183003));
#28792=CARTESIAN_POINT('Ctrl Pts',(1.75032866075914,1.,-1.10806728183003));
#28793=CARTESIAN_POINT('Ctrl Pts',(1.75367772094617,-1.,-1.11330807582542));
#28794=CARTESIAN_POINT('Ctrl Pts',(1.75367772094617,1.,-1.11330807582542));
#28795=CARTESIAN_POINT('Ctrl Pts',(1.75699720772089,-1.,-1.11858293216752));
#28796=CARTESIAN_POINT('Ctrl Pts',(1.75699720772089,1.,-1.11858293216752));
#28797=CARTESIAN_POINT('Ctrl Pts',(1.76028671825084,-1.,-1.12389096855078));
#28798=CARTESIAN_POINT('Ctrl Pts',(1.76028671825084,1.,-1.12389096855078));
#28799=CARTESIAN_POINT('Ctrl Pts',(1.76354571966171,-1.,-1.12923123555076));
#28800=CARTESIAN_POINT('Ctrl Pts',(1.76354571966171,1.,-1.12923123555076));
#28801=CARTESIAN_POINT('Ctrl Pts',(1.76677384551883,-1.,-1.13460291804635));
#28802=CARTESIAN_POINT('Ctrl Pts',(1.76677384551883,1.,-1.13460291804635));
#28803=CARTESIAN_POINT('Ctrl Pts',(1.76997111386806,-1.,-1.14000548337));
#28804=CARTESIAN_POINT('Ctrl Pts',(1.76997111386806,1.,-1.14000548337));
#28805=CARTESIAN_POINT('Ctrl Pts',(1.77313777896234,-1.,-1.14543858226948));
#28806=CARTESIAN_POINT('Ctrl Pts',(1.77313777896234,1.,-1.14543858226948));
#28807=CARTESIAN_POINT('Ctrl Pts',(1.77627422557034,-1.,-1.15090197841531));
#28808=CARTESIAN_POINT('Ctrl Pts',(1.77627422557034,1.,-1.15090197841531));
#28809=CARTESIAN_POINT('Ctrl Pts',(1.77938085564261,-1.,-1.15639547194689));
#28810=CARTESIAN_POINT('Ctrl Pts',(1.77938085564261,1.,-1.15639547194689));
#28811=CARTESIAN_POINT('Ctrl Pts',(1.78245795880949,-1.,-1.16191881298458));
#28812=CARTESIAN_POINT('Ctrl Pts',(1.78245795880949,1.,-1.16191881298458));
#28813=CARTESIAN_POINT('Ctrl Pts',(1.78550566040349,-1.,-1.16747166312239));
#28814=CARTESIAN_POINT('Ctrl Pts',(1.78550566040349,1.,-1.16747166312239));
#28815=CARTESIAN_POINT('Ctrl Pts',(1.78852398877523,-1.,-1.17305363177265));
#28816=CARTESIAN_POINT('Ctrl Pts',(1.78852398877523,1.,-1.17305363177265));
#28817=CARTESIAN_POINT('Ctrl Pts',(1.79151291552646,-1.,-1.17866429440781));
#28818=CARTESIAN_POINT('Ctrl Pts',(1.79151291552646,1.,-1.17866429440781));
#28819=CARTESIAN_POINT('Ctrl Pts',(1.79447240321572,-1.,-1.18430321697471));
#28820=CARTESIAN_POINT('Ctrl Pts',(1.79447240321572,1.,-1.18430321697471));
#28821=CARTESIAN_POINT('Ctrl Pts',(1.79740245923649,-1.,-1.1899699793456));
#28822=CARTESIAN_POINT('Ctrl Pts',(1.79740245923649,1.,-1.1899699793456));
#28823=CARTESIAN_POINT('Ctrl Pts',(1.80030314370121,-1.,-1.19566418930405));
#28824=CARTESIAN_POINT('Ctrl Pts',(1.80030314370121,1.,-1.19566418930405));
#28825=CARTESIAN_POINT('Ctrl Pts',(1.8031745483882,-1.,-1.2013854893912));
#28826=CARTESIAN_POINT('Ctrl Pts',(1.8031745483882,1.,-1.2013854893912));
#28827=CARTESIAN_POINT('Ctrl Pts',(1.80601678480772,-1.,-1.20713356605519));
#28828=CARTESIAN_POINT('Ctrl Pts',(1.80601678480772,1.,-1.20713356605519));
#28829=CARTESIAN_POINT('Ctrl Pts',(1.80882996916931,-1.,-1.2129081570818));
#28830=CARTESIAN_POINT('Ctrl Pts',(1.80882996916931,1.,-1.2129081570818));
#28831=CARTESIAN_POINT('Ctrl Pts',(1.81161420806172,-1.,-1.2187090610323));
#28832=CARTESIAN_POINT('Ctrl Pts',(1.81161420806172,1.,-1.2187090610323));
#28833=CARTESIAN_POINT('Ctrl Pts',(1.81436959209778,-1.,-1.22453613304507));
#28834=CARTESIAN_POINT('Ctrl Pts',(1.81436959209778,1.,-1.22453613304507));
#28835=CARTESIAN_POINT('Ctrl Pts',(1.81655087183054,-1.,-1.22921864890975));
#28836=CARTESIAN_POINT('Ctrl Pts',(1.81655087183054,1.,-1.22921864890975));
#28837=CARTESIAN_POINT('Ctrl Pts',(1.81817389920914,-1.,-1.23274224526804));
#28838=CARTESIAN_POINT('Ctrl Pts',(1.81817389920914,1.,-1.23274224526804));
#28839=CARTESIAN_POINT('Ctrl Pts',(1.81925017193531,-1.,-1.23509651170384));
#28840=CARTESIAN_POINT('Ctrl Pts',(1.81925017193531,1.,-1.23509651170384));
#28841=CARTESIAN_POINT('Ctrl Pts',(1.81978687191668,-1.,-1.23627494547115));
#28842=CARTESIAN_POINT('Ctrl Pts',(1.81978687191668,1.,-1.23627494547115));
#28843=CARTESIAN_POINT('',(1.5055822144029,1.,-0.892032620296855));
#28844=CARTESIAN_POINT('Ctrl Pts',(1.5055822144029,1.,-0.892032620296855));
#28845=CARTESIAN_POINT('Ctrl Pts',(1.50980486807181,1.,-0.894452006967538));
#28846=CARTESIAN_POINT('Ctrl Pts',(1.51805569591479,1.,-0.89918504749193));
#28847=CARTESIAN_POINT('Ctrl Pts',(1.52984849890434,1.,-0.905967409640499));
#28848=CARTESIAN_POINT('Ctrl Pts',(1.54440491152807,1.,-0.91437591904658));
#28849=CARTESIAN_POINT('Ctrl Pts',(1.56065988582509,1.,-0.923832188966322));
#28850=CARTESIAN_POINT('Ctrl Pts',(1.57499388385561,1.,-0.932246680128849));
#28851=CARTESIAN_POINT('Ctrl Pts',(1.58744937489796,1.,-0.939646377909319));
#28852=CARTESIAN_POINT('Ctrl Pts',(1.59810042045408,1.,-0.946078063325796));
#28853=CARTESIAN_POINT('Ctrl Pts',(1.60706069897794,1.,-0.951613284361248));
#28854=CARTESIAN_POINT('Ctrl Pts',(1.61449324337233,1.,-0.956354422921573));
#28855=CARTESIAN_POINT('Ctrl Pts',(1.62061638139929,1.,-0.960438326099958));
#28856=CARTESIAN_POINT('Ctrl Pts',(1.6257193066974,1.,-0.964046107037821));
#28857=CARTESIAN_POINT('Ctrl Pts',(1.63013849959083,1.,-0.967387853228041));
#28858=CARTESIAN_POINT('Ctrl Pts',(1.63420665729609,1.,-0.970669715996356));
#28859=CARTESIAN_POINT('Ctrl Pts',(1.63820952658157,1.,-0.974066058287501));
#28860=CARTESIAN_POINT('Ctrl Pts',(1.64233990826831,1.,-0.977689794120297));
#28861=CARTESIAN_POINT('Ctrl Pts',(1.64665139190834,1.,-0.981562530940574));
#28862=CARTESIAN_POINT('Ctrl Pts',(1.6511001661277,1.,-0.985642622921626));
#28863=CARTESIAN_POINT('Ctrl Pts',(1.65559044289746,1.,-0.98985562785445));
#28864=CARTESIAN_POINT('Ctrl Pts',(1.66001553809916,1.,-0.994121836661116));
#28865=CARTESIAN_POINT('Ctrl Pts',(1.66430758030304,1.,-0.998389654952317));
#28866=CARTESIAN_POINT('Ctrl Pts',(1.66846059277231,1.,-1.00265091003682));
#28867=CARTESIAN_POINT('Ctrl Pts',(1.67250335383248,1.,-1.00692206696387));
#28868=CARTESIAN_POINT('Ctrl Pts',(1.67648246776457,1.,-1.01123236493507));
#28869=CARTESIAN_POINT('Ctrl Pts',(1.6804428989482,1.,-1.01561026162787));
#28870=CARTESIAN_POINT('Ctrl Pts',(1.68440578021739,1.,-1.02006795074222));
#28871=CARTESIAN_POINT('Ctrl Pts',(1.68836910178475,1.,-1.02460180535272));
#28872=CARTESIAN_POINT('Ctrl Pts',(1.69231840863471,1.,-1.02919977579155));
#28873=CARTESIAN_POINT('Ctrl Pts',(1.69623414782769,1.,-1.03384646003587));
#28874=CARTESIAN_POINT('Ctrl Pts',(1.70010052930951,1.,-1.03852922490782));
#28875=CARTESIAN_POINT('Ctrl Pts',(1.70391338707969,1.,-1.04324363334546));
#28876=CARTESIAN_POINT('Ctrl Pts',(1.70767646263641,1.,-1.0479908540499));
#28877=CARTESIAN_POINT('Ctrl Pts',(1.71139783543986,1.,-1.05277517202854));
#28878=CARTESIAN_POINT('Ctrl Pts',(1.71508654427022,1.,-1.05760163192481));
#28879=CARTESIAN_POINT('Ctrl Pts',(1.71874858456908,1.,-1.0624732468065));
#28880=CARTESIAN_POINT('Ctrl Pts',(1.72238500928456,1.,-1.06738966975463));
#28881=CARTESIAN_POINT('Ctrl Pts',(1.72599406198489,1.,-1.07234866990252));
#28882=CARTESIAN_POINT('Ctrl Pts',(1.72957248977424,1.,-1.0773470373727));
#28883=CARTESIAN_POINT('Ctrl Pts',(1.73311705663407,1.,-1.08238162784749));
#28884=CARTESIAN_POINT('Ctrl Pts',(1.73662628326093,1.,-1.08745056285429));
#28885=CARTESIAN_POINT('Ctrl Pts',(1.74010053962252,1.,-1.09255329056496));
#28886=CARTESIAN_POINT('Ctrl Pts',(1.74354119236212,1.,-1.09768999241229));
#28887=CARTESIAN_POINT('Ctrl Pts',(1.74695004214924,1.,-1.10286118991144));
#28888=CARTESIAN_POINT('Ctrl Pts',(1.75032866075914,1.,-1.10806728183003));
#28889=CARTESIAN_POINT('Ctrl Pts',(1.75367772094617,1.,-1.11330807582542));
#28890=CARTESIAN_POINT('Ctrl Pts',(1.75699720772089,1.,-1.11858293216752));
#28891=CARTESIAN_POINT('Ctrl Pts',(1.76028671825084,1.,-1.12389096855078));
#28892=CARTESIAN_POINT('Ctrl Pts',(1.76354571966171,1.,-1.12923123555076));
#28893=CARTESIAN_POINT('Ctrl Pts',(1.76677384551883,1.,-1.13460291804635));
#28894=CARTESIAN_POINT('Ctrl Pts',(1.76997111386806,1.,-1.14000548337));
#28895=CARTESIAN_POINT('Ctrl Pts',(1.77313777896234,1.,-1.14543858226948));
#28896=CARTESIAN_POINT('Ctrl Pts',(1.77627422557034,1.,-1.15090197841531));
#28897=CARTESIAN_POINT('Ctrl Pts',(1.77938085564261,1.,-1.15639547194689));
#28898=CARTESIAN_POINT('Ctrl Pts',(1.78245795880949,1.,-1.16191881298458));
#28899=CARTESIAN_POINT('Ctrl Pts',(1.78550566040349,1.,-1.16747166312239));
#28900=CARTESIAN_POINT('Ctrl Pts',(1.78852398877523,1.,-1.17305363177265));
#28901=CARTESIAN_POINT('Ctrl Pts',(1.79151291552646,1.,-1.17866429440781));
#28902=CARTESIAN_POINT('Ctrl Pts',(1.79447240321572,1.,-1.18430321697471));
#28903=CARTESIAN_POINT('Ctrl Pts',(1.79740245923649,1.,-1.1899699793456));
#28904=CARTESIAN_POINT('Ctrl Pts',(1.80030314370121,1.,-1.19566418930405));
#28905=CARTESIAN_POINT('Ctrl Pts',(1.8031745483882,1.,-1.2013854893912));
#28906=CARTESIAN_POINT('Ctrl Pts',(1.80601678480772,1.,-1.20713356605519));
#28907=CARTESIAN_POINT('Ctrl Pts',(1.80882996916931,1.,-1.2129081570818));
#28908=CARTESIAN_POINT('Ctrl Pts',(1.81161420806172,1.,-1.2187090610323));
#28909=CARTESIAN_POINT('Ctrl Pts',(1.81436959209778,1.,-1.22453613304507));
#28910=CARTESIAN_POINT('Ctrl Pts',(1.81655087183054,1.,-1.22921864890975));
#28911=CARTESIAN_POINT('Ctrl Pts',(1.81817389920914,1.,-1.23274224526804));
#28912=CARTESIAN_POINT('Ctrl Pts',(1.81925017193531,1.,-1.23509651170384));
#28913=CARTESIAN_POINT('Ctrl Pts',(1.81978687191668,1.,-1.23627494547115));
#28914=CARTESIAN_POINT('',(1.5055822144029,0.,-0.892032620296855));
#28915=CARTESIAN_POINT('Origin',(0.,0.,0.));
#28916=CARTESIAN_POINT('',(1.60662857109684,1.,-0.693717979106306));
#28917=CARTESIAN_POINT('Origin',(0.,1.,0.));
#28918=CARTESIAN_POINT('',(1.60662857109684,0.,-0.693717979106308));
#28919=CARTESIAN_POINT('Ctrl Pts',(2.0698113262342,-1.,-0.745574324794401));
#28920=CARTESIAN_POINT('Ctrl Pts',(2.0698113262342,1.,-0.745574324794401));
#28921=CARTESIAN_POINT('Ctrl Pts',(2.06854248895728,-1.,-0.745832791378367));
#28922=CARTESIAN_POINT('Ctrl Pts',(2.06854248895728,1.,-0.745832791378367));
#28923=CARTESIAN_POINT('Ctrl Pts',(2.06600523016815,-1.,-0.746345871544201));
#28924=CARTESIAN_POINT('Ctrl Pts',(2.06600523016815,1.,-0.746345871544201));
#28925=CARTESIAN_POINT('Ctrl Pts',(2.06220058927826,-1.,-0.74710393278792));
#28926=CARTESIAN_POINT('Ctrl Pts',(2.06220058927826,1.,-0.74710393278792));
#28927=CARTESIAN_POINT('Ctrl Pts',(2.05713023031006,-1.,-0.748091554183803));
#28928=CARTESIAN_POINT('Ctrl Pts',(2.05713023031006,1.,-0.748091554183803));
#28929=CARTESIAN_POINT('Ctrl Pts',(2.05079645592154,-1.,-0.749287468665046));
#28930=CARTESIAN_POINT('Ctrl Pts',(2.05079645592154,1.,-0.749287468665046));
#28931=CARTESIAN_POINT('Ctrl Pts',(2.04446689147979,-1.,-0.750444657875576));
#28932=CARTESIAN_POINT('Ctrl Pts',(2.04446689147979,1.,-0.750444657875576));
#28933=CARTESIAN_POINT('Ctrl Pts',(2.03814160092099,-1.,-0.751562963361115));
#28934=CARTESIAN_POINT('Ctrl Pts',(2.03814160092099,1.,-0.751562963361115));
#28935=CARTESIAN_POINT('Ctrl Pts',(2.03182068456221,-1.,-0.752642180487211));
#28936=CARTESIAN_POINT('Ctrl Pts',(2.03182068456221,1.,-0.752642180487211));
#28937=CARTESIAN_POINT('Ctrl Pts',(2.02550428623313,-1.,-0.753682061112768));
#28938=CARTESIAN_POINT('Ctrl Pts',(2.02550428623313,1.,-0.753682061112768));
#28939=CARTESIAN_POINT('Ctrl Pts',(2.01919259405809,-1.,-0.754682330722816));
#28940=CARTESIAN_POINT('Ctrl Pts',(2.01919259405809,1.,-0.754682330722816));
#28941=CARTESIAN_POINT('Ctrl Pts',(2.01288584328084,-1.,-0.755642704957865));
#28942=CARTESIAN_POINT('Ctrl Pts',(2.01288584328084,1.,-0.755642704957865));
#28943=CARTESIAN_POINT('Ctrl Pts',(2.0065843158773,-1.,-0.756562904646671));
#28944=CARTESIAN_POINT('Ctrl Pts',(2.0065843158773,1.,-0.756562904646671));
#28945=CARTESIAN_POINT('Ctrl Pts',(2.00028834739178,-1.,-0.757442676862724));
#28946=CARTESIAN_POINT('Ctrl Pts',(2.00028834739178,1.,-0.757442676862724));
#28947=CARTESIAN_POINT('Ctrl Pts',(1.99399831098817,-1.,-0.758281796766761));
#28948=CARTESIAN_POINT('Ctrl Pts',(1.99399831098817,1.,-0.758281796766761));
#28949=CARTESIAN_POINT('Ctrl Pts',(1.98771456680874,-1.,-0.759080037802488));
#28950=CARTESIAN_POINT('Ctrl Pts',(1.98771456680874,1.,-0.759080037802488));
#28951=CARTESIAN_POINT('Ctrl Pts',(1.98143741418172,-1.,-0.75983714745219));
#28952=CARTESIAN_POINT('Ctrl Pts',(1.98143741418172,1.,-0.75983714745219));
#28953=CARTESIAN_POINT('Ctrl Pts',(1.97516705321494,-1.,-0.760552825409757));
#28954=CARTESIAN_POINT('Ctrl Pts',(1.97516705321494,1.,-0.760552825409757));
#28955=CARTESIAN_POINT('Ctrl Pts',(1.96890351582499,-1.,-0.761226690483821));
#28956=CARTESIAN_POINT('Ctrl Pts',(1.96890351582499,1.,-0.761226690483821));
#28957=CARTESIAN_POINT('Ctrl Pts',(1.96264672744186,-1.,-0.761858300014424));
#28958=CARTESIAN_POINT('Ctrl Pts',(1.96264672744186,1.,-0.761858300014424));
#28959=CARTESIAN_POINT('Ctrl Pts',(1.95639665309869,-1.,-0.762447203806179));
#28960=CARTESIAN_POINT('Ctrl Pts',(1.95639665309869,1.,-0.762447203806179));
#28961=CARTESIAN_POINT('Ctrl Pts',(1.95015342590024,-1.,-0.762992990878769));
#28962=CARTESIAN_POINT('Ctrl Pts',(1.95015342590024,1.,-0.762992990878769));
#28963=CARTESIAN_POINT('Ctrl Pts',(1.9439174661764,-1.,-0.763495333538629));
#28964=CARTESIAN_POINT('Ctrl Pts',(1.9439174661764,1.,-0.763495333538629));
#28965=CARTESIAN_POINT('Ctrl Pts',(1.93768964875886,-1.,-0.763954049121459));
#28966=CARTESIAN_POINT('Ctrl Pts',(1.93768964875886,1.,-0.763954049121459));
#28967=CARTESIAN_POINT('Ctrl Pts',(1.93147105496382,-1.,-0.764369010673941));
#28968=CARTESIAN_POINT('Ctrl Pts',(1.93147105496382,1.,-0.764369010673941));
#28969=CARTESIAN_POINT('Ctrl Pts',(1.92526263537048,-1.,-0.764740025488212));
#28970=CARTESIAN_POINT('Ctrl Pts',(1.92526263537048,1.,-0.764740025488212));
#28971=CARTESIAN_POINT('Ctrl Pts',(1.91906491634196,-1.,-0.765066729667089));
#28972=CARTESIAN_POINT('Ctrl Pts',(1.91906491634196,1.,-0.765066729667089));
#28973=CARTESIAN_POINT('Ctrl Pts',(1.91287765805169,-1.,-0.765348465884722));
#28974=CARTESIAN_POINT('Ctrl Pts',(1.91287765805169,1.,-0.765348465884722));
#28975=CARTESIAN_POINT('Ctrl Pts',(1.90669961402356,-1.,-0.765584196937919));
#28976=CARTESIAN_POINT('Ctrl Pts',(1.90669961402356,1.,-0.765584196937919));
#28977=CARTESIAN_POINT('Ctrl Pts',(1.90052930393596,-1.,-0.765772772593386));
#28978=CARTESIAN_POINT('Ctrl Pts',(1.90052930393596,1.,-0.765772772593386));
#28979=CARTESIAN_POINT('Ctrl Pts',(1.89436577771388,-1.,-0.765913193856978));
#28980=CARTESIAN_POINT('Ctrl Pts',(1.89436577771388,1.,-0.765913193856978));
#28981=CARTESIAN_POINT('Ctrl Pts',(1.88820926433409,-1.,-0.766004837062091));
#28982=CARTESIAN_POINT('Ctrl Pts',(1.88820926433409,1.,-0.766004837062091));
#28983=CARTESIAN_POINT('Ctrl Pts',(1.88206215302561,-1.,-0.766047794851865));
#28984=CARTESIAN_POINT('Ctrl Pts',(1.88206215302561,1.,-0.766047794851865));
#28985=CARTESIAN_POINT('Ctrl Pts',(1.87592888967883,-1.,-0.766042837036744));
#28986=CARTESIAN_POINT('Ctrl Pts',(1.87592888967883,1.,-0.766042837036744));
#28987=CARTESIAN_POINT('Ctrl Pts',(1.86981398314341,-1.,-0.765990708546091));
#28988=CARTESIAN_POINT('Ctrl Pts',(1.86981398314341,1.,-0.765990708546091));
#28989=CARTESIAN_POINT('Ctrl Pts',(1.86372027063312,-1.,-0.765891519092547));
#28990=CARTESIAN_POINT('Ctrl Pts',(1.86372027063312,1.,-0.765891519092547));
#28991=CARTESIAN_POINT('Ctrl Pts',(1.85764741390394,-1.,-0.765744212909319));
#28992=CARTESIAN_POINT('Ctrl Pts',(1.85764741390394,1.,-0.765744212909319));
#28993=CARTESIAN_POINT('Ctrl Pts',(1.85158945130063,-1.,-0.765545710619063));
#28994=CARTESIAN_POINT('Ctrl Pts',(1.85158945130063,1.,-0.765545710619063));
#28995=CARTESIAN_POINT('Ctrl Pts',(1.84553698875924,-1.,-0.765291664862029));
#28996=CARTESIAN_POINT('Ctrl Pts',(1.84553698875924,1.,-0.765291664862029));
#28997=CARTESIAN_POINT('Ctrl Pts',(1.83948181064835,-1.,-0.764978057881738));
#28998=CARTESIAN_POINT('Ctrl Pts',(1.83948181064835,1.,-0.764978057881738));
#28999=CARTESIAN_POINT('Ctrl Pts',(1.83342077227142,-1.,-0.764602549687853));
#29000=CARTESIAN_POINT('Ctrl Pts',(1.83342077227142,1.,-0.764602549687853));
#29001=CARTESIAN_POINT('Ctrl Pts',(1.82735991200065,-1.,-0.764165902605995));
#29002=CARTESIAN_POINT('Ctrl Pts',(1.82735991200065,1.,-0.764165902605995));
#29003=CARTESIAN_POINT('Ctrl Pts',(1.82131873145266,-1.,-0.763673465462727));
#29004=CARTESIAN_POINT('Ctrl Pts',(1.82131873145266,1.,-0.763673465462727));
#29005=CARTESIAN_POINT('Ctrl Pts',(1.8153211840553,-1.,-0.763132003836634));
#29006=CARTESIAN_POINT('Ctrl Pts',(1.8153211840553,1.,-0.763132003836634));
#29007=CARTESIAN_POINT('Ctrl Pts',(1.80938551463965,-1.,-0.762546129463938));
#29008=CARTESIAN_POINT('Ctrl Pts',(1.80938551463965,1.,-0.762546129463938));
#29009=CARTESIAN_POINT('Ctrl Pts',(1.80351583877342,-1.,-0.761915336443547));
#29010=CARTESIAN_POINT('Ctrl Pts',(1.80351583877342,1.,-0.761915336443547));
#29011=CARTESIAN_POINT('Ctrl Pts',(1.79768986997783,-1.,-0.761229695230558));
#29012=CARTESIAN_POINT('Ctrl Pts',(1.79768986997783,1.,-0.761229695230558));
#29013=CARTESIAN_POINT('Ctrl Pts',(1.7918581561088,-1.,-0.760469555880749));
#29014=CARTESIAN_POINT('Ctrl Pts',(1.7918581561088,1.,-0.760469555880749));
#29015=CARTESIAN_POINT('Ctrl Pts',(1.78596964884604,-1.,-0.75961440111019));
#29016=CARTESIAN_POINT('Ctrl Pts',(1.78596964884604,1.,-0.75961440111019));
#29017=CARTESIAN_POINT('Ctrl Pts',(1.77999411220945,-1.,-0.758650626677519));
#29018=CARTESIAN_POINT('Ctrl Pts',(1.77999411220945,1.,-0.758650626677519));
#29019=CARTESIAN_POINT('Ctrl Pts',(1.77394167108292,-1.,-0.757578264077029));
#29020=CARTESIAN_POINT('Ctrl Pts',(1.77394167108292,1.,-0.757578264077029));
#29021=CARTESIAN_POINT('Ctrl Pts',(1.76789396002998,-1.,-0.75642189602781));
#29022=CARTESIAN_POINT('Ctrl Pts',(1.76789396002998,1.,-0.75642189602781));
#29023=CARTESIAN_POINT('Ctrl Pts',(1.76197817240128,-1.,-0.755220979974462));
#29024=CARTESIAN_POINT('Ctrl Pts',(1.76197817240128,1.,-0.755220979974462));
#29025=CARTESIAN_POINT('Ctrl Pts',(1.75631083600019,-1.,-0.754009254027829));
#29026=CARTESIAN_POINT('Ctrl Pts',(1.75631083600019,1.,-0.754009254027829));
#29027=CARTESIAN_POINT('Ctrl Pts',(1.75095139468794,-1.,-0.752797683531314));
#29028=CARTESIAN_POINT('Ctrl Pts',(1.75095139468794,1.,-0.752797683531314));
#29029=CARTESIAN_POINT('Ctrl Pts',(1.74585086852502,-1.,-0.751555614164483));
#29030=CARTESIAN_POINT('Ctrl Pts',(1.74585086852502,1.,-0.751555614164483));
#29031=CARTESIAN_POINT('Ctrl Pts',(1.74080458267114,-1.,-0.75019343598125));
#29032=CARTESIAN_POINT('Ctrl Pts',(1.74080458267114,1.,-0.75019343598125));
#29033=CARTESIAN_POINT('Ctrl Pts',(1.7355035168033,-1.,-0.74858246295687));
#29034=CARTESIAN_POINT('Ctrl Pts',(1.7355035168033,1.,-0.74858246295687));
#29035=CARTESIAN_POINT('Ctrl Pts',(1.72958533647714,-1.,-0.746574710097752));
#29036=CARTESIAN_POINT('Ctrl Pts',(1.72958533647714,1.,-0.746574710097752));
#29037=CARTESIAN_POINT('Ctrl Pts',(1.72268229916769,-1.,-0.744021445433094));
#29038=CARTESIAN_POINT('Ctrl Pts',(1.72268229916769,1.,-0.744021445433094));
#29039=CARTESIAN_POINT('Ctrl Pts',(1.71447789751001,-1.,-0.74079516202821));
#29040=CARTESIAN_POINT('Ctrl Pts',(1.71447789751001,1.,-0.74079516202821));
#29041=CARTESIAN_POINT('Ctrl Pts',(1.70473309004249,-1.,-0.736799665716932));
#29042=CARTESIAN_POINT('Ctrl Pts',(1.70473309004249,1.,-0.736799665716932));
#29043=CARTESIAN_POINT('Ctrl Pts',(1.69326921972915,-1.,-0.731963238685357));
#29044=CARTESIAN_POINT('Ctrl Pts',(1.69326921972915,1.,-0.731963238685357));
#29045=CARTESIAN_POINT('Ctrl Pts',(1.67996158451922,-1.,-0.726235967982445));
#29046=CARTESIAN_POINT('Ctrl Pts',(1.67996158451922,1.,-0.726235967982445));
#29047=CARTESIAN_POINT('Ctrl Pts',(1.66472880551777,-1.,-0.71958543378795));
#29048=CARTESIAN_POINT('Ctrl Pts',(1.66472880551777,1.,-0.71958543378795));
#29049=CARTESIAN_POINT('Ctrl Pts',(1.64752408828442,-1.,-0.711993139340448));
#29050=CARTESIAN_POINT('Ctrl Pts',(1.64752408828442,1.,-0.711993139340448));
#29051=CARTESIAN_POINT('Ctrl Pts',(1.6321654166204,-1.,-0.705159151977294));
#29052=CARTESIAN_POINT('Ctrl Pts',(1.6321654166204,1.,-0.705159151977294));
#29053=CARTESIAN_POINT('Ctrl Pts',(1.61974673471117,-1.,-0.699605146398837));
#29054=CARTESIAN_POINT('Ctrl Pts',(1.61974673471117,1.,-0.699605146398837));
#29055=CARTESIAN_POINT('Ctrl Pts',(1.61106790957619,-1.,-0.69571209787897));
#29056=CARTESIAN_POINT('Ctrl Pts',(1.61106790957619,1.,-0.69571209787897));
#29057=CARTESIAN_POINT('Ctrl Pts',(1.60662857109684,-1.,-0.693717979106306));
#29058=CARTESIAN_POINT('Ctrl Pts',(1.60662857109684,1.,-0.693717979106306));
#29059=CARTESIAN_POINT('',(2.0698113262342,1.,-0.745574324794401));
#29060=CARTESIAN_POINT('Ctrl Pts',(2.0698113262342,1.,-0.745574324794401));
#29061=CARTESIAN_POINT('Ctrl Pts',(2.06854248895728,1.,-0.745832791378367));
#29062=CARTESIAN_POINT('Ctrl Pts',(2.06600523016815,1.,-0.746345871544201));
#29063=CARTESIAN_POINT('Ctrl Pts',(2.06220058927826,1.,-0.74710393278792));
#29064=CARTESIAN_POINT('Ctrl Pts',(2.05713023031006,1.,-0.748091554183803));
#29065=CARTESIAN_POINT('Ctrl Pts',(2.05079645592154,1.,-0.749287468665046));
#29066=CARTESIAN_POINT('Ctrl Pts',(2.04446689147979,1.,-0.750444657875576));
#29067=CARTESIAN_POINT('Ctrl Pts',(2.03814160092099,1.,-0.751562963361115));
#29068=CARTESIAN_POINT('Ctrl Pts',(2.03182068456221,1.,-0.752642180487211));
#29069=CARTESIAN_POINT('Ctrl Pts',(2.02550428623313,1.,-0.753682061112768));
#29070=CARTESIAN_POINT('Ctrl Pts',(2.01919259405809,1.,-0.754682330722816));
#29071=CARTESIAN_POINT('Ctrl Pts',(2.01288584328084,1.,-0.755642704957865));
#29072=CARTESIAN_POINT('Ctrl Pts',(2.0065843158773,1.,-0.756562904646671));
#29073=CARTESIAN_POINT('Ctrl Pts',(2.00028834739178,1.,-0.757442676862724));
#29074=CARTESIAN_POINT('Ctrl Pts',(1.99399831098817,1.,-0.758281796766761));
#29075=CARTESIAN_POINT('Ctrl Pts',(1.98771456680874,1.,-0.759080037802488));
#29076=CARTESIAN_POINT('Ctrl Pts',(1.98143741418172,1.,-0.75983714745219));
#29077=CARTESIAN_POINT('Ctrl Pts',(1.97516705321494,1.,-0.760552825409757));
#29078=CARTESIAN_POINT('Ctrl Pts',(1.96890351582499,1.,-0.761226690483821));
#29079=CARTESIAN_POINT('Ctrl Pts',(1.96264672744186,1.,-0.761858300014424));
#29080=CARTESIAN_POINT('Ctrl Pts',(1.95639665309869,1.,-0.762447203806179));
#29081=CARTESIAN_POINT('Ctrl Pts',(1.95015342590024,1.,-0.762992990878769));
#29082=CARTESIAN_POINT('Ctrl Pts',(1.9439174661764,1.,-0.763495333538629));
#29083=CARTESIAN_POINT('Ctrl Pts',(1.93768964875886,1.,-0.763954049121459));
#29084=CARTESIAN_POINT('Ctrl Pts',(1.93147105496382,1.,-0.764369010673941));
#29085=CARTESIAN_POINT('Ctrl Pts',(1.92526263537048,1.,-0.764740025488212));
#29086=CARTESIAN_POINT('Ctrl Pts',(1.91906491634196,1.,-0.765066729667089));
#29087=CARTESIAN_POINT('Ctrl Pts',(1.91287765805169,1.,-0.765348465884722));
#29088=CARTESIAN_POINT('Ctrl Pts',(1.90669961402356,1.,-0.765584196937919));
#29089=CARTESIAN_POINT('Ctrl Pts',(1.90052930393596,1.,-0.765772772593386));
#29090=CARTESIAN_POINT('Ctrl Pts',(1.89436577771388,1.,-0.765913193856978));
#29091=CARTESIAN_POINT('Ctrl Pts',(1.88820926433409,1.,-0.766004837062091));
#29092=CARTESIAN_POINT('Ctrl Pts',(1.88206215302561,1.,-0.766047794851865));
#29093=CARTESIAN_POINT('Ctrl Pts',(1.87592888967883,1.,-0.766042837036744));
#29094=CARTESIAN_POINT('Ctrl Pts',(1.86981398314341,1.,-0.765990708546091));
#29095=CARTESIAN_POINT('Ctrl Pts',(1.86372027063312,1.,-0.765891519092547));
#29096=CARTESIAN_POINT('Ctrl Pts',(1.85764741390394,1.,-0.765744212909319));
#29097=CARTESIAN_POINT('Ctrl Pts',(1.85158945130063,1.,-0.765545710619063));
#29098=CARTESIAN_POINT('Ctrl Pts',(1.84553698875924,1.,-0.765291664862029));
#29099=CARTESIAN_POINT('Ctrl Pts',(1.83948181064835,1.,-0.764978057881738));
#29100=CARTESIAN_POINT('Ctrl Pts',(1.83342077227142,1.,-0.764602549687853));
#29101=CARTESIAN_POINT('Ctrl Pts',(1.82735991200065,1.,-0.764165902605995));
#29102=CARTESIAN_POINT('Ctrl Pts',(1.82131873145266,1.,-0.763673465462727));
#29103=CARTESIAN_POINT('Ctrl Pts',(1.8153211840553,1.,-0.763132003836634));
#29104=CARTESIAN_POINT('Ctrl Pts',(1.80938551463965,1.,-0.762546129463938));
#29105=CARTESIAN_POINT('Ctrl Pts',(1.80351583877342,1.,-0.761915336443547));
#29106=CARTESIAN_POINT('Ctrl Pts',(1.79768986997783,1.,-0.761229695230558));
#29107=CARTESIAN_POINT('Ctrl Pts',(1.7918581561088,1.,-0.760469555880749));
#29108=CARTESIAN_POINT('Ctrl Pts',(1.78596964884604,1.,-0.75961440111019));
#29109=CARTESIAN_POINT('Ctrl Pts',(1.77999411220945,1.,-0.758650626677519));
#29110=CARTESIAN_POINT('Ctrl Pts',(1.77394167108292,1.,-0.757578264077029));
#29111=CARTESIAN_POINT('Ctrl Pts',(1.76789396002998,1.,-0.75642189602781));
#29112=CARTESIAN_POINT('Ctrl Pts',(1.76197817240128,1.,-0.755220979974462));
#29113=CARTESIAN_POINT('Ctrl Pts',(1.75631083600019,1.,-0.754009254027829));
#29114=CARTESIAN_POINT('Ctrl Pts',(1.75095139468794,1.,-0.752797683531314));
#29115=CARTESIAN_POINT('Ctrl Pts',(1.74585086852502,1.,-0.751555614164483));
#29116=CARTESIAN_POINT('Ctrl Pts',(1.74080458267114,1.,-0.75019343598125));
#29117=CARTESIAN_POINT('Ctrl Pts',(1.7355035168033,1.,-0.74858246295687));
#29118=CARTESIAN_POINT('Ctrl Pts',(1.72958533647714,1.,-0.746574710097752));
#29119=CARTESIAN_POINT('Ctrl Pts',(1.72268229916769,1.,-0.744021445433094));
#29120=CARTESIAN_POINT('Ctrl Pts',(1.71447789751001,1.,-0.74079516202821));
#29121=CARTESIAN_POINT('Ctrl Pts',(1.70473309004249,1.,-0.736799665716932));
#29122=CARTESIAN_POINT('Ctrl Pts',(1.69326921972915,1.,-0.731963238685357));
#29123=CARTESIAN_POINT('Ctrl Pts',(1.67996158451922,1.,-0.726235967982445));
#29124=CARTESIAN_POINT('Ctrl Pts',(1.66472880551777,1.,-0.71958543378795));
#29125=CARTESIAN_POINT('Ctrl Pts',(1.64752408828442,1.,-0.711993139340448));
#29126=CARTESIAN_POINT('Ctrl Pts',(1.6321654166204,1.,-0.705159151977294));
#29127=CARTESIAN_POINT('Ctrl Pts',(1.61974673471117,1.,-0.699605146398837));
#29128=CARTESIAN_POINT('Ctrl Pts',(1.61106790957619,1.,-0.69571209787897));
#29129=CARTESIAN_POINT('Ctrl Pts',(1.60662857109684,1.,-0.693717979106306));
#29130=CARTESIAN_POINT('',(2.0698113262342,0.,-0.745574324794401));
#29131=CARTESIAN_POINT('Origin',(2.11275013067528,0.,-0.61342227326009));
#29132=CARTESIAN_POINT('',(2.11275013067528,1.,-0.61342227326009));
#29133=CARTESIAN_POINT('',(2.0698113262342,1.,-0.745574324794401));
#29134=CARTESIAN_POINT('',(2.11275013067528,0.,-0.61342227326009));
#29135=CARTESIAN_POINT('Ctrl Pts',(1.7075470150345,-1.,-0.383122945602004));
#29136=CARTESIAN_POINT('Ctrl Pts',(1.7075470150345,1.,-0.383122945602004));
#29137=CARTESIAN_POINT('Ctrl Pts',(1.71231062891958,-1.,-0.384119047315542));
#29138=CARTESIAN_POINT('Ctrl Pts',(1.71231062891958,1.,-0.384119047315542));
#29139=CARTESIAN_POINT('Ctrl Pts',(1.72162022246158,-1.,-0.38607079032701));
#29140=CARTESIAN_POINT('Ctrl Pts',(1.72162022246158,1.,-0.38607079032701));
#29141=CARTESIAN_POINT('Ctrl Pts',(1.7349317097561,-1.,-0.388877023509192));
#29142=CARTESIAN_POINT('Ctrl Pts',(1.7349317097561,1.,-0.388877023509192));
#29143=CARTESIAN_POINT('Ctrl Pts',(1.75137405313962,-1.,-0.392375812294307));
#29144=CARTESIAN_POINT('Ctrl Pts',(1.75137405313962,1.,-0.392375812294307));
#29145=CARTESIAN_POINT('Ctrl Pts',(1.7697556004756,-1.,-0.39634619612042));
#29146=CARTESIAN_POINT('Ctrl Pts',(1.7697556004756,1.,-0.39634619612042));
#29147=CARTESIAN_POINT('Ctrl Pts',(1.78598826347533,-1.,-0.399919403783081));
#29148=CARTESIAN_POINT('Ctrl Pts',(1.78598826347533,1.,-0.399919403783081));
#29149=CARTESIAN_POINT('Ctrl Pts',(1.80012077176221,-1.,-0.403107976170441));
#29150=CARTESIAN_POINT('Ctrl Pts',(1.80012077176221,1.,-0.403107976170441));
#29151=CARTESIAN_POINT('Ctrl Pts',(1.81223801813988,-1.,-0.405933518411838));
#29152=CARTESIAN_POINT('Ctrl Pts',(1.81223801813988,1.,-0.405933518411838));
#29153=CARTESIAN_POINT('Ctrl Pts',(1.8224702267854,-1.,-0.408428948108534));
#29154=CARTESIAN_POINT('Ctrl Pts',(1.8224702267854,1.,-0.408428948108534));
#29155=CARTESIAN_POINT('Ctrl Pts',(1.83100408895216,-1.,-0.410641256301675));
#29156=CARTESIAN_POINT('Ctrl Pts',(1.83100408895216,1.,-0.410641256301675));
#29157=CARTESIAN_POINT('Ctrl Pts',(1.83808953475839,-1.,-0.412633125322162));
#29158=CARTESIAN_POINT('Ctrl Pts',(1.83808953475839,1.,-0.412633125322162));
#29159=CARTESIAN_POINT('Ctrl Pts',(1.8440575707371,-1.,-0.41448743825434));
#29160=CARTESIAN_POINT('Ctrl Pts',(1.8440575707371,1.,-0.41448743825434));
#29161=CARTESIAN_POINT('Ctrl Pts',(1.84929312929882,-1.,-0.416300022038864));
#29162=CARTESIAN_POINT('Ctrl Pts',(1.84929312929882,1.,-0.416300022038864));
#29163=CARTESIAN_POINT('Ctrl Pts',(1.85417632856234,-1.,-0.418164129143534));
#29164=CARTESIAN_POINT('Ctrl Pts',(1.85417632856234,1.,-0.418164129143534));
#29165=CARTESIAN_POINT('Ctrl Pts',(1.85903281096686,-1.,-0.42015728797562));
#29166=CARTESIAN_POINT('Ctrl Pts',(1.85903281096686,1.,-0.42015728797562));
#29167=CARTESIAN_POINT('Ctrl Pts',(1.86408083334028,-1.,-0.422327307418275));
#29168=CARTESIAN_POINT('Ctrl Pts',(1.86408083334028,1.,-0.422327307418275));
#29169=CARTESIAN_POINT('Ctrl Pts',(1.86937803944323,-1.,-0.424678177291359));
#29170=CARTESIAN_POINT('Ctrl Pts',(1.86937803944323,1.,-0.424678177291359));
#29171=CARTESIAN_POINT('Ctrl Pts',(1.87486989291484,-1.,-0.427183828519102));
#29172=CARTESIAN_POINT('Ctrl Pts',(1.87486989291484,1.,-0.427183828519102));
#29173=CARTESIAN_POINT('Ctrl Pts',(1.88044229001832,-1.,-0.429803062482345));
#29174=CARTESIAN_POINT('Ctrl Pts',(1.88044229001832,1.,-0.429803062482345));
#29175=CARTESIAN_POINT('Ctrl Pts',(1.88596913666793,-1.,-0.432493038548748));
#29176=CARTESIAN_POINT('Ctrl Pts',(1.88596913666793,1.,-0.432493038548748));
#29177=CARTESIAN_POINT('Ctrl Pts',(1.89136993975504,-1.,-0.435225660963383));
#29178=CARTESIAN_POINT('Ctrl Pts',(1.89136993975504,1.,-0.435225660963383));
#29179=CARTESIAN_POINT('Ctrl Pts',(1.89663648956466,-1.,-0.437995003948244));
#29180=CARTESIAN_POINT('Ctrl Pts',(1.89663648956466,1.,-0.437995003948244));
#29181=CARTESIAN_POINT('Ctrl Pts',(1.90180124389086,-1.,-0.440807833704038));
#29182=CARTESIAN_POINT('Ctrl Pts',(1.90180124389086,1.,-0.440807833704038));
#29183=CARTESIAN_POINT('Ctrl Pts',(1.90691756144898,-1.,-0.443677556849151));
#29184=CARTESIAN_POINT('Ctrl Pts',(1.90691756144898,1.,-0.443677556849151));
#29185=CARTESIAN_POINT('Ctrl Pts',(1.9120369998112,-1.,-0.446617343485711));
#29186=CARTESIAN_POINT('Ctrl Pts',(1.9120369998112,1.,-0.446617343485711));
#29187=CARTESIAN_POINT('Ctrl Pts',(1.91718342555755,-1.,-0.449632260106662));
#29188=CARTESIAN_POINT('Ctrl Pts',(1.91718342555755,1.,-0.449632260106662));
#29189=CARTESIAN_POINT('Ctrl Pts',(1.92235380648502,-1.,-0.452719478359433));
#29190=CARTESIAN_POINT('Ctrl Pts',(1.92235380648502,1.,-0.452719478359433));
#29191=CARTESIAN_POINT('Ctrl Pts',(1.92753067150476,-1.,-0.455872005174371));
#29192=CARTESIAN_POINT('Ctrl Pts',(1.92753067150476,1.,-0.455872005174371));
#29193=CARTESIAN_POINT('Ctrl Pts',(1.93269066517934,-1.,-0.459081234547926));
#29194=CARTESIAN_POINT('Ctrl Pts',(1.93269066517934,1.,-0.459081234547926));
#29195=CARTESIAN_POINT('Ctrl Pts',(1.93781486640821,-1.,-0.462340031009057));
#29196=CARTESIAN_POINT('Ctrl Pts',(1.93781486640821,1.,-0.462340031009057));
#29197=CARTESIAN_POINT('Ctrl Pts',(1.9428979419619,-1.,-0.46564546202603));
#29198=CARTESIAN_POINT('Ctrl Pts',(1.9428979419619,1.,-0.46564546202603));
#29199=CARTESIAN_POINT('Ctrl Pts',(1.94794381136514,-1.,-0.468997482913135));
#29200=CARTESIAN_POINT('Ctrl Pts',(1.94794381136514,1.,-0.468997482913135));
#29201=CARTESIAN_POINT('Ctrl Pts',(1.95296148278133,-1.,-0.472397672264072));
#29202=CARTESIAN_POINT('Ctrl Pts',(1.95296148278133,1.,-0.472397672264072));
#29203=CARTESIAN_POINT('Ctrl Pts',(1.95796111148177,-1.,-0.475848034683176));
#29204=CARTESIAN_POINT('Ctrl Pts',(1.95796111148177,1.,-0.475848034683176));
#29205=CARTESIAN_POINT('Ctrl Pts',(1.96294933055943,-1.,-0.479349583074855));
#29206=CARTESIAN_POINT('Ctrl Pts',(1.96294933055943,1.,-0.479349583074855));
#29207=CARTESIAN_POINT('Ctrl Pts',(1.96792703422362,-1.,-0.482901662120691));
#29208=CARTESIAN_POINT('Ctrl Pts',(1.96792703422362,1.,-0.482901662120691));
#29209=CARTESIAN_POINT('Ctrl Pts',(1.97289186263272,-1.,-0.486502692907659));
#29210=CARTESIAN_POINT('Ctrl Pts',(1.97289186263272,1.,-0.486502692907659));
#29211=CARTESIAN_POINT('Ctrl Pts',(1.97783973019229,-1.,-0.490150627860953));
#29212=CARTESIAN_POINT('Ctrl Pts',(1.97783973019229,1.,-0.490150627860953));
#29213=CARTESIAN_POINT('Ctrl Pts',(1.98276658761821,-1.,-0.493843476541495));
#29214=CARTESIAN_POINT('Ctrl Pts',(1.98276658761821,1.,-0.493843476541495));
#29215=CARTESIAN_POINT('Ctrl Pts',(1.98767044752932,-1.,-0.497579909545574));
#29216=CARTESIAN_POINT('Ctrl Pts',(1.98767044752932,1.,-0.497579909545574));
#29217=CARTESIAN_POINT('Ctrl Pts',(1.99255149126155,-1.,-0.501359287727146));
#29218=CARTESIAN_POINT('Ctrl Pts',(1.99255149126155,1.,-0.501359287727146));
#29219=CARTESIAN_POINT('Ctrl Pts',(1.99741107463572,-1.,-0.505181361323026));
#29220=CARTESIAN_POINT('Ctrl Pts',(1.99741107463572,1.,-0.505181361323026));
#29221=CARTESIAN_POINT('Ctrl Pts',(2.00225107134734,-1.,-0.509046069886157));
#29222=CARTESIAN_POINT('Ctrl Pts',(2.00225107134734,1.,-0.509046069886157));
#29223=CARTESIAN_POINT('Ctrl Pts',(2.00707309946949,-1.,-0.512953306961793));
#29224=CARTESIAN_POINT('Ctrl Pts',(2.00707309946949,1.,-0.512953306961793));
#29225=CARTESIAN_POINT('Ctrl Pts',(2.01187773939242,-1.,-0.516902681728687));
#29226=CARTESIAN_POINT('Ctrl Pts',(2.01187773939242,1.,-0.516902681728687));
#29227=CARTESIAN_POINT('Ctrl Pts',(2.01666477917286,-1.,-0.520893590399371));
#29228=CARTESIAN_POINT('Ctrl Pts',(2.01666477917286,1.,-0.520893590399371));
#29229=CARTESIAN_POINT('Ctrl Pts',(2.02143356304698,-1.,-0.524925318333476));
#29230=CARTESIAN_POINT('Ctrl Pts',(2.02143356304698,1.,-0.524925318333476));
#29231=CARTESIAN_POINT('Ctrl Pts',(2.0261832908329,-1.,-0.528997127241914));
#29232=CARTESIAN_POINT('Ctrl Pts',(2.0261832908329,1.,-0.528997127241914));
#29233=CARTESIAN_POINT('Ctrl Pts',(2.03091336214426,-1.,-0.533108355132977));
#29234=CARTESIAN_POINT('Ctrl Pts',(2.03091336214426,1.,-0.533108355132977));
#29235=CARTESIAN_POINT('Ctrl Pts',(2.03562362954037,-1.,-0.537258489833262));
#29236=CARTESIAN_POINT('Ctrl Pts',(2.03562362954037,1.,-0.537258489833262));
#29237=CARTESIAN_POINT('Ctrl Pts',(2.04031422690527,-1.,-0.541447120615659));
#29238=CARTESIAN_POINT('Ctrl Pts',(2.04031422690527,1.,-0.541447120615659));
#29239=CARTESIAN_POINT('Ctrl Pts',(2.04498544714588,-1.,-0.54567390381743));
#29240=CARTESIAN_POINT('Ctrl Pts',(2.04498544714588,1.,-0.54567390381743));
#29241=CARTESIAN_POINT('Ctrl Pts',(2.04963761077958,-1.,-0.549938525150295));
#29242=CARTESIAN_POINT('Ctrl Pts',(2.04963761077958,1.,-0.549938525150295));
#29243=CARTESIAN_POINT('Ctrl Pts',(2.05427091604413,-1.,-0.554240657463906));
#29244=CARTESIAN_POINT('Ctrl Pts',(2.05427091604413,1.,-0.554240657463906));
#29245=CARTESIAN_POINT('Ctrl Pts',(2.05888537756462,-1.,-0.558579940185152));
#29246=CARTESIAN_POINT('Ctrl Pts',(2.05888537756462,1.,-0.558579940185152));
#29247=CARTESIAN_POINT('Ctrl Pts',(2.06348090160589,-1.,-0.562955993082262));
#29248=CARTESIAN_POINT('Ctrl Pts',(2.06348090160589,1.,-0.562955993082262));
#29249=CARTESIAN_POINT('Ctrl Pts',(2.06805732997334,-1.,-0.567368421181087));
#29250=CARTESIAN_POINT('Ctrl Pts',(2.06805732997334,1.,-0.567368421181087));
#29251=CARTESIAN_POINT('Ctrl Pts',(2.07261449292824,-1.,-0.571816823242603));
#29252=CARTESIAN_POINT('Ctrl Pts',(2.07261449292824,1.,-0.571816823242603));
#29253=CARTESIAN_POINT('Ctrl Pts',(2.07715226767559,-1.,-0.576300797416845));
#29254=CARTESIAN_POINT('Ctrl Pts',(2.07715226767559,1.,-0.576300797416845));
#29255=CARTESIAN_POINT('Ctrl Pts',(2.08167059018418,-1.,-0.580819952108064));
#29256=CARTESIAN_POINT('Ctrl Pts',(2.08167059018418,1.,-0.580819952108064));
#29257=CARTESIAN_POINT('Ctrl Pts',(2.08616943727951,-1.,-0.585373918991617));
#29258=CARTESIAN_POINT('Ctrl Pts',(2.08616943727951,1.,-0.585373918991617));
#29259=CARTESIAN_POINT('Ctrl Pts',(2.09064881812129,-1.,-0.589962365403406));
#29260=CARTESIAN_POINT('Ctrl Pts',(2.09064881812129,1.,-0.589962365403406));
#29261=CARTESIAN_POINT('Ctrl Pts',(2.0951087622027,-1.,-0.594585006052162));
#29262=CARTESIAN_POINT('Ctrl Pts',(2.0951087622027,1.,-0.594585006052162));
#29263=CARTESIAN_POINT('Ctrl Pts',(2.0995493086477,-1.,-0.599241616420534));
#29264=CARTESIAN_POINT('Ctrl Pts',(2.0995493086477,1.,-0.599241616420534));
#29265=CARTESIAN_POINT('Ctrl Pts',(2.10397049886949,-1.,-0.60393203073603));
#29266=CARTESIAN_POINT('Ctrl Pts',(2.10397049886949,1.,-0.60393203073603));
#29267=CARTESIAN_POINT('Ctrl Pts',(2.1074919961518,-1.,-0.607711315454876));
#29268=CARTESIAN_POINT('Ctrl Pts',(2.1074919961518,1.,-0.607711315454876));
#29269=CARTESIAN_POINT('Ctrl Pts',(2.11012443807238,-1.,-0.610560911689899));
#29270=CARTESIAN_POINT('Ctrl Pts',(2.11012443807238,1.,-0.610560911689899));
#29271=CARTESIAN_POINT('Ctrl Pts',(2.11187554259986,-1.,-0.6124673655618));
#29272=CARTESIAN_POINT('Ctrl Pts',(2.11187554259986,1.,-0.6124673655618));
#29273=CARTESIAN_POINT('Ctrl Pts',(2.11275013067528,-1.,-0.61342227326009));
#29274=CARTESIAN_POINT('Ctrl Pts',(2.11275013067528,1.,-0.61342227326009));
#29275=CARTESIAN_POINT('',(1.7075470150345,1.,-0.383122945602004));
#29276=CARTESIAN_POINT('Ctrl Pts',(1.7075470150345,1.,-0.383122945602004));
#29277=CARTESIAN_POINT('Ctrl Pts',(1.71231062891958,1.,-0.384119047315542));
#29278=CARTESIAN_POINT('Ctrl Pts',(1.72162022246158,1.,-0.38607079032701));
#29279=CARTESIAN_POINT('Ctrl Pts',(1.7349317097561,1.,-0.388877023509192));
#29280=CARTESIAN_POINT('Ctrl Pts',(1.75137405313962,1.,-0.392375812294307));
#29281=CARTESIAN_POINT('Ctrl Pts',(1.7697556004756,1.,-0.39634619612042));
#29282=CARTESIAN_POINT('Ctrl Pts',(1.78598826347533,1.,-0.399919403783081));
#29283=CARTESIAN_POINT('Ctrl Pts',(1.80012077176221,1.,-0.403107976170441));
#29284=CARTESIAN_POINT('Ctrl Pts',(1.81223801813988,1.,-0.405933518411838));
#29285=CARTESIAN_POINT('Ctrl Pts',(1.8224702267854,1.,-0.408428948108534));
#29286=CARTESIAN_POINT('Ctrl Pts',(1.83100408895216,1.,-0.410641256301675));
#29287=CARTESIAN_POINT('Ctrl Pts',(1.83808953475839,1.,-0.412633125322162));
#29288=CARTESIAN_POINT('Ctrl Pts',(1.8440575707371,1.,-0.41448743825434));
#29289=CARTESIAN_POINT('Ctrl Pts',(1.84929312929882,1.,-0.416300022038864));
#29290=CARTESIAN_POINT('Ctrl Pts',(1.85417632856234,1.,-0.418164129143534));
#29291=CARTESIAN_POINT('Ctrl Pts',(1.85903281096686,1.,-0.42015728797562));
#29292=CARTESIAN_POINT('Ctrl Pts',(1.86408083334028,1.,-0.422327307418275));
#29293=CARTESIAN_POINT('Ctrl Pts',(1.86937803944323,1.,-0.424678177291359));
#29294=CARTESIAN_POINT('Ctrl Pts',(1.87486989291484,1.,-0.427183828519102));
#29295=CARTESIAN_POINT('Ctrl Pts',(1.88044229001832,1.,-0.429803062482345));
#29296=CARTESIAN_POINT('Ctrl Pts',(1.88596913666793,1.,-0.432493038548748));
#29297=CARTESIAN_POINT('Ctrl Pts',(1.89136993975504,1.,-0.435225660963383));
#29298=CARTESIAN_POINT('Ctrl Pts',(1.89663648956466,1.,-0.437995003948244));
#29299=CARTESIAN_POINT('Ctrl Pts',(1.90180124389086,1.,-0.440807833704038));
#29300=CARTESIAN_POINT('Ctrl Pts',(1.90691756144898,1.,-0.443677556849151));
#29301=CARTESIAN_POINT('Ctrl Pts',(1.9120369998112,1.,-0.446617343485711));
#29302=CARTESIAN_POINT('Ctrl Pts',(1.91718342555755,1.,-0.449632260106662));
#29303=CARTESIAN_POINT('Ctrl Pts',(1.92235380648502,1.,-0.452719478359433));
#29304=CARTESIAN_POINT('Ctrl Pts',(1.92753067150476,1.,-0.455872005174371));
#29305=CARTESIAN_POINT('Ctrl Pts',(1.93269066517934,1.,-0.459081234547926));
#29306=CARTESIAN_POINT('Ctrl Pts',(1.93781486640821,1.,-0.462340031009057));
#29307=CARTESIAN_POINT('Ctrl Pts',(1.9428979419619,1.,-0.46564546202603));
#29308=CARTESIAN_POINT('Ctrl Pts',(1.94794381136514,1.,-0.468997482913135));
#29309=CARTESIAN_POINT('Ctrl Pts',(1.95296148278133,1.,-0.472397672264072));
#29310=CARTESIAN_POINT('Ctrl Pts',(1.95796111148177,1.,-0.475848034683176));
#29311=CARTESIAN_POINT('Ctrl Pts',(1.96294933055943,1.,-0.479349583074855));
#29312=CARTESIAN_POINT('Ctrl Pts',(1.96792703422362,1.,-0.482901662120691));
#29313=CARTESIAN_POINT('Ctrl Pts',(1.97289186263272,1.,-0.486502692907659));
#29314=CARTESIAN_POINT('Ctrl Pts',(1.97783973019229,1.,-0.490150627860953));
#29315=CARTESIAN_POINT('Ctrl Pts',(1.98276658761821,1.,-0.493843476541495));
#29316=CARTESIAN_POINT('Ctrl Pts',(1.98767044752932,1.,-0.497579909545574));
#29317=CARTESIAN_POINT('Ctrl Pts',(1.99255149126155,1.,-0.501359287727146));
#29318=CARTESIAN_POINT('Ctrl Pts',(1.99741107463572,1.,-0.505181361323026));
#29319=CARTESIAN_POINT('Ctrl Pts',(2.00225107134734,1.,-0.509046069886157));
#29320=CARTESIAN_POINT('Ctrl Pts',(2.00707309946949,1.,-0.512953306961793));
#29321=CARTESIAN_POINT('Ctrl Pts',(2.01187773939242,1.,-0.516902681728687));
#29322=CARTESIAN_POINT('Ctrl Pts',(2.01666477917286,1.,-0.520893590399371));
#29323=CARTESIAN_POINT('Ctrl Pts',(2.02143356304698,1.,-0.524925318333476));
#29324=CARTESIAN_POINT('Ctrl Pts',(2.0261832908329,1.,-0.528997127241914));
#29325=CARTESIAN_POINT('Ctrl Pts',(2.03091336214426,1.,-0.533108355132977));
#29326=CARTESIAN_POINT('Ctrl Pts',(2.03562362954037,1.,-0.537258489833262));
#29327=CARTESIAN_POINT('Ctrl Pts',(2.04031422690527,1.,-0.541447120615659));
#29328=CARTESIAN_POINT('Ctrl Pts',(2.04498544714588,1.,-0.54567390381743));
#29329=CARTESIAN_POINT('Ctrl Pts',(2.04963761077958,1.,-0.549938525150295));
#29330=CARTESIAN_POINT('Ctrl Pts',(2.05427091604413,1.,-0.554240657463906));
#29331=CARTESIAN_POINT('Ctrl Pts',(2.05888537756462,1.,-0.558579940185152));
#29332=CARTESIAN_POINT('Ctrl Pts',(2.06348090160589,1.,-0.562955993082262));
#29333=CARTESIAN_POINT('Ctrl Pts',(2.06805732997334,1.,-0.567368421181087));
#29334=CARTESIAN_POINT('Ctrl Pts',(2.07261449292824,1.,-0.571816823242603));
#29335=CARTESIAN_POINT('Ctrl Pts',(2.07715226767559,1.,-0.576300797416845));
#29336=CARTESIAN_POINT('Ctrl Pts',(2.08167059018418,1.,-0.580819952108064));
#29337=CARTESIAN_POINT('Ctrl Pts',(2.08616943727951,1.,-0.585373918991617));
#29338=CARTESIAN_POINT('Ctrl Pts',(2.09064881812129,1.,-0.589962365403406));
#29339=CARTESIAN_POINT('Ctrl Pts',(2.0951087622027,1.,-0.594585006052162));
#29340=CARTESIAN_POINT('Ctrl Pts',(2.0995493086477,1.,-0.599241616420534));
#29341=CARTESIAN_POINT('Ctrl Pts',(2.10397049886949,1.,-0.60393203073603));
#29342=CARTESIAN_POINT('Ctrl Pts',(2.1074919961518,1.,-0.607711315454876));
#29343=CARTESIAN_POINT('Ctrl Pts',(2.11012443807238,1.,-0.610560911689899));
#29344=CARTESIAN_POINT('Ctrl Pts',(2.11187554259986,1.,-0.6124673655618));
#29345=CARTESIAN_POINT('Ctrl Pts',(2.11275013067528,1.,-0.61342227326009));
#29346=CARTESIAN_POINT('',(1.7075470150345,0.,-0.383122945602001));
#29347=CARTESIAN_POINT('Origin',(0.,0.,0.));
#29348=CARTESIAN_POINT('',(1.74236521665491,1.,-0.163289472382896));
#29349=CARTESIAN_POINT('Origin',(0.,1.,0.));
#29350=CARTESIAN_POINT('',(1.74236521665491,0.,-0.163289472382896));
#29351=CARTESIAN_POINT('Ctrl Pts',(2.19890268624765,-1.,-0.0694764450219582));
#29352=CARTESIAN_POINT('Ctrl Pts',(2.19890268624765,1.,-0.0694764450219582));
#29353=CARTESIAN_POINT('Ctrl Pts',(2.19777582085423,-1.,-0.0701143536325491));
#29354=CARTESIAN_POINT('Ctrl Pts',(2.19777582085423,1.,-0.0701143536325491));
#29355=CARTESIAN_POINT('Ctrl Pts',(2.19552129484002,-1.,-0.0713863779526155));
#29356=CARTESIAN_POINT('Ctrl Pts',(2.19552129484002,1.,-0.0713863779526155));
#29357=CARTESIAN_POINT('Ctrl Pts',(2.19213712013662,-1.,-0.0732830357306726));
#29358=CARTESIAN_POINT('Ctrl Pts',(2.19213712013662,1.,-0.0732830357306726));
#29359=CARTESIAN_POINT('Ctrl Pts',(2.1876201139953,-1.,-0.0757891465836149));
#29360=CARTESIAN_POINT('Ctrl Pts',(2.1876201139953,1.,-0.0757891465836149));
#29361=CARTESIAN_POINT('Ctrl Pts',(2.18196589448887,-1.,-0.0788837727685244));
#29362=CARTESIAN_POINT('Ctrl Pts',(2.18196589448887,1.,-0.0788837727685244));
#29363=CARTESIAN_POINT('Ctrl Pts',(2.176303712113,-1.,-0.0819402680872767));
#29364=CARTESIAN_POINT('Ctrl Pts',(2.176303712113,1.,-0.0819402680872767));
#29365=CARTESIAN_POINT('Ctrl Pts',(2.17063357870952,-1.,-0.0849584620835374));
#29366=CARTESIAN_POINT('Ctrl Pts',(2.17063357870952,1.,-0.0849584620835374));
#29367=CARTESIAN_POINT('Ctrl Pts',(2.16495552645014,-1.,-0.0879381291386924));
#29368=CARTESIAN_POINT('Ctrl Pts',(2.16495552645014,1.,-0.0879381291386924));
#29369=CARTESIAN_POINT('Ctrl Pts',(2.15926961544516,-1.,-0.0908789888107267));
#29370=CARTESIAN_POINT('Ctrl Pts',(2.15926961544516,1.,-0.0908789888107267));
#29371=CARTESIAN_POINT('Ctrl Pts',(2.1535759397817,-1.,-0.0937807218867645));
#29372=CARTESIAN_POINT('Ctrl Pts',(2.1535759397817,1.,-0.0937807218867645));
#29373=CARTESIAN_POINT('Ctrl Pts',(2.14787463531795,-1.,-0.096642985230546));
#29374=CARTESIAN_POINT('Ctrl Pts',(2.14787463531795,1.,-0.096642985230546));
#29375=CARTESIAN_POINT('Ctrl Pts',(2.14216588396025,-1.,-0.0994654261990917));
#29376=CARTESIAN_POINT('Ctrl Pts',(2.14216588396025,1.,-0.0994654261990917));
#29377=CARTESIAN_POINT('Ctrl Pts',(2.13644992667165,-1.,-0.102247700556101));
#29378=CARTESIAN_POINT('Ctrl Pts',(2.13644992667165,1.,-0.102247700556101));
#29379=CARTESIAN_POINT('Ctrl Pts',(2.13072704887293,-1.,-0.10498947915274));
#29380=CARTESIAN_POINT('Ctrl Pts',(2.13072704887293,1.,-0.10498947915274));
#29381=CARTESIAN_POINT('Ctrl Pts',(2.12499752307,-1.,-0.10769043523109));
#29382=CARTESIAN_POINT('Ctrl Pts',(2.12499752307,1.,-0.10769043523109));
#29383=CARTESIAN_POINT('Ctrl Pts',(2.11926155590865,-1.,-0.110350236135025));
#29384=CARTESIAN_POINT('Ctrl Pts',(2.11926155590865,1.,-0.110350236135025));
#29385=CARTESIAN_POINT('Ctrl Pts',(2.11351924490306,-1.,-0.112968534419737));
#29386=CARTESIAN_POINT('Ctrl Pts',(2.11351924490306,1.,-0.112968534419737));
#29387=CARTESIAN_POINT('Ctrl Pts',(2.10777050261309,-1.,-0.115544957687927));
#29388=CARTESIAN_POINT('Ctrl Pts',(2.10777050261309,1.,-0.115544957687927));
#29389=CARTESIAN_POINT('Ctrl Pts',(2.102015121329,-1.,-0.118079107988356));
#29390=CARTESIAN_POINT('Ctrl Pts',(2.102015121329,1.,-0.118079107988356));
#29391=CARTESIAN_POINT('Ctrl Pts',(2.0962529286773,-1.,-0.120570567965122));
#29392=CARTESIAN_POINT('Ctrl Pts',(2.0962529286773,1.,-0.120570567965122));
#29393=CARTESIAN_POINT('Ctrl Pts',(2.09048392424825,-1.,-0.123018905621083));
#29394=CARTESIAN_POINT('Ctrl Pts',(2.09048392424825,1.,-0.123018905621083));
#29395=CARTESIAN_POINT('Ctrl Pts',(2.08470840653643,-1.,-0.125423679412062));
#29396=CARTESIAN_POINT('Ctrl Pts',(2.08470840653643,1.,-0.125423679412062));
#29397=CARTESIAN_POINT('Ctrl Pts',(2.07892715110987,-1.,-0.12778444527612));
#29398=CARTESIAN_POINT('Ctrl Pts',(2.07892715110987,1.,-0.12778444527612));
#29399=CARTESIAN_POINT('Ctrl Pts',(2.07314114713063,-1.,-0.130100748328404));
#29400=CARTESIAN_POINT('Ctrl Pts',(2.07314114713063,1.,-0.130100748328404));
#29401=CARTESIAN_POINT('Ctrl Pts',(2.06735123910326,-1.,-0.132372111547711));
#29402=CARTESIAN_POINT('Ctrl Pts',(2.06735123910326,1.,-0.132372111547711));
#29403=CARTESIAN_POINT('Ctrl Pts',(2.06155781517842,-1.,-0.134598026192106));
#29404=CARTESIAN_POINT('Ctrl Pts',(2.06155781517842,1.,-0.134598026192106));
#29405=CARTESIAN_POINT('Ctrl Pts',(2.05576044414264,-1.,-0.136777941218044));
#29406=CARTESIAN_POINT('Ctrl Pts',(2.05576044414264,1.,-0.136777941218044));
#29407=CARTESIAN_POINT('Ctrl Pts',(2.04995762001328,-1.,-0.138911255368966));
#29408=CARTESIAN_POINT('Ctrl Pts',(2.04995762001328,1.,-0.138911255368966));
#29409=CARTESIAN_POINT('Ctrl Pts',(2.04414757947916,-1.,-0.140997332152546));
#29410=CARTESIAN_POINT('Ctrl Pts',(2.04414757947916,1.,-0.140997332152546));
#29411=CARTESIAN_POINT('Ctrl Pts',(2.03832911025912,-1.,-0.143035515058209));
#29412=CARTESIAN_POINT('Ctrl Pts',(2.03832911025912,1.,-0.143035515058209));
#29413=CARTESIAN_POINT('Ctrl Pts',(2.03250223739942,-1.,-0.145025140186058));
#29414=CARTESIAN_POINT('Ctrl Pts',(2.03250223739942,1.,-0.145025140186058));
#29415=CARTESIAN_POINT('Ctrl Pts',(2.02666926182017,-1.,-0.146965557332583));
#29416=CARTESIAN_POINT('Ctrl Pts',(2.02666926182017,1.,-0.146965557332583));
#29417=CARTESIAN_POINT('Ctrl Pts',(2.02083464969894,-1.,-0.148856124775337));
#29418=CARTESIAN_POINT('Ctrl Pts',(2.02083464969894,1.,-0.148856124775337));
#29419=CARTESIAN_POINT('Ctrl Pts',(2.01500291940238,-1.,-0.150696157673078));
#29420=CARTESIAN_POINT('Ctrl Pts',(2.01500291940238,1.,-0.150696157673078));
#29421=CARTESIAN_POINT('Ctrl Pts',(2.00917680318424,-1.,-0.15248488362145));
#29422=CARTESIAN_POINT('Ctrl Pts',(2.00917680318424,1.,-0.15248488362145));
#29423=CARTESIAN_POINT('Ctrl Pts',(2.00335565310543,-1.,-0.154221403049722));
#29424=CARTESIAN_POINT('Ctrl Pts',(2.00335565310543,1.,-0.154221403049722));
#29425=CARTESIAN_POINT('Ctrl Pts',(1.99753284771497,-1.,-0.155904629548784));
#29426=CARTESIAN_POINT('Ctrl Pts',(1.99753284771497,1.,-0.155904629548784));
#29427=CARTESIAN_POINT('Ctrl Pts',(1.99169810931908,-1.,-0.157533331459227));
#29428=CARTESIAN_POINT('Ctrl Pts',(1.99169810931908,1.,-0.157533331459227));
#29429=CARTESIAN_POINT('Ctrl Pts',(1.98584238283292,-1.,-0.159106226437299));
#29430=CARTESIAN_POINT('Ctrl Pts',(1.98584238283292,1.,-0.159106226437299));
#29431=CARTESIAN_POINT('Ctrl Pts',(1.97996195437559,-1.,-0.160622060784611));
#29432=CARTESIAN_POINT('Ctrl Pts',(1.97996195437559,1.,-0.160622060784611));
#29433=CARTESIAN_POINT('Ctrl Pts',(1.97406280235188,-1.,-0.162079693556289));
#29434=CARTESIAN_POINT('Ctrl Pts',(1.97406280235188,1.,-0.162079693556289));
#29435=CARTESIAN_POINT('Ctrl Pts',(1.96816512677967,-1.,-0.163478185457734));
#29436=CARTESIAN_POINT('Ctrl Pts',(1.96816512677967,1.,-0.163478185457734));
#29437=CARTESIAN_POINT('Ctrl Pts',(1.96229379940136,-1.,-0.164816568920269));
#29438=CARTESIAN_POINT('Ctrl Pts',(1.96229379940136,1.,-0.164816568920269));
#29439=CARTESIAN_POINT('Ctrl Pts',(1.9564675971873,-1.,-0.166093592002813));
#29440=CARTESIAN_POINT('Ctrl Pts',(1.9564675971873,1.,-0.166093592002813));
#29441=CARTESIAN_POINT('Ctrl Pts',(1.95069027794294,-1.,-0.167307501784476));
#29442=CARTESIAN_POINT('Ctrl Pts',(1.95069027794294,1.,-0.167307501784476));
#29443=CARTESIAN_POINT('Ctrl Pts',(1.94493757756931,-1.,-0.168455741607556));
#29444=CARTESIAN_POINT('Ctrl Pts',(1.94493757756931,1.,-0.168455741607556));
#29445=CARTESIAN_POINT('Ctrl Pts',(1.93915639211581,-1.,-0.169534904817491));
#29446=CARTESIAN_POINT('Ctrl Pts',(1.93915639211581,1.,-0.169534904817491));
#29447=CARTESIAN_POINT('Ctrl Pts',(1.93329183155539,-1.,-0.170541253116202));
#29448=CARTESIAN_POINT('Ctrl Pts',(1.93329183155539,1.,-0.170541253116202));
#29449=CARTESIAN_POINT('Ctrl Pts',(1.92731093582036,-1.,-0.171471191532988));
#29450=CARTESIAN_POINT('Ctrl Pts',(1.92731093582036,1.,-0.171471191532988));
#29451=CARTESIAN_POINT('Ctrl Pts',(1.9212233439798,-1.,-0.172321621259514));
#29452=CARTESIAN_POINT('Ctrl Pts',(1.9212233439798,1.,-0.172321621259514));
#29453=CARTESIAN_POINT('Ctrl Pts',(1.91511429159527,-1.,-0.173090695383496));
#29454=CARTESIAN_POINT('Ctrl Pts',(1.91511429159527,1.,-0.173090695383496));
#29455=CARTESIAN_POINT('Ctrl Pts',(1.90911693975267,-1.,-0.173776635257817));
#29456=CARTESIAN_POINT('Ctrl Pts',(1.90911693975267,1.,-0.173776635257817));
#29457=CARTESIAN_POINT('Ctrl Pts',(1.90335253862834,-1.,-0.174375518661085));
#29458=CARTESIAN_POINT('Ctrl Pts',(1.90335253862834,1.,-0.174375518661085));
#29459=CARTESIAN_POINT('Ctrl Pts',(1.89788101117132,-1.,-0.174879405091263));
#29460=CARTESIAN_POINT('Ctrl Pts',(1.89788101117132,1.,-0.174879405091263));
#29461=CARTESIAN_POINT('Ctrl Pts',(1.892646301985,-1.,-0.175274276190844));
#29462=CARTESIAN_POINT('Ctrl Pts',(1.892646301985,1.,-0.175274276190844));
#29463=CARTESIAN_POINT('Ctrl Pts',(1.88742606273259,-1.,-0.175538155840648));
#29464=CARTESIAN_POINT('Ctrl Pts',(1.88742606273259,1.,-0.175538155840648));
#29465=CARTESIAN_POINT('Ctrl Pts',(1.88188663145367,-1.,-0.175644148889699));
#29466=CARTESIAN_POINT('Ctrl Pts',(1.88188663145367,1.,-0.175644148889699));
#29467=CARTESIAN_POINT('Ctrl Pts',(1.87563767773588,-1.,-0.175563480746485));
#29468=CARTESIAN_POINT('Ctrl Pts',(1.87563767773588,1.,-0.175563480746485));
#29469=CARTESIAN_POINT('Ctrl Pts',(1.86828349694799,-1.,-0.175268337590758));
#29470=CARTESIAN_POINT('Ctrl Pts',(1.86828349694799,1.,-0.175268337590758));
#29471=CARTESIAN_POINT('Ctrl Pts',(1.85948367088837,-1.,-0.17473525927603));
#29472=CARTESIAN_POINT('Ctrl Pts',(1.85948367088837,1.,-0.17473525927603));
#29473=CARTESIAN_POINT('Ctrl Pts',(1.8489811319852,-1.,-0.173946627587732));
#29474=CARTESIAN_POINT('Ctrl Pts',(1.8489811319852,1.,-0.173946627587732));
#29475=CARTESIAN_POINT('Ctrl Pts',(1.83658380527692,-1.,-0.1728894428919));
#29476=CARTESIAN_POINT('Ctrl Pts',(1.83658380527692,1.,-0.1728894428919));
#29477=CARTESIAN_POINT('Ctrl Pts',(1.82215766811545,-1.,-0.171554770204119));
#29478=CARTESIAN_POINT('Ctrl Pts',(1.82215766811545,1.,-0.171554770204119));
#29479=CARTESIAN_POINT('Ctrl Pts',(1.80561530629706,-1.,-0.169936923904608));
#29480=CARTESIAN_POINT('Ctrl Pts',(1.80561530629706,1.,-0.169936923904608));
#29481=CARTESIAN_POINT('Ctrl Pts',(1.7869064998507,-1.,-0.168032772805197));
#29482=CARTESIAN_POINT('Ctrl Pts',(1.7869064998507,1.,-0.168032772805197));
#29483=CARTESIAN_POINT('Ctrl Pts',(1.77018771684844,-1.,-0.1662793551464));
#29484=CARTESIAN_POINT('Ctrl Pts',(1.77018771684844,1.,-0.1662793551464));
#29485=CARTESIAN_POINT('Ctrl Pts',(1.75666056638427,-1.,-0.164834765707159));
#29486=CARTESIAN_POINT('Ctrl Pts',(1.75666056638427,1.,-0.164834765707159));
#29487=CARTESIAN_POINT('Ctrl Pts',(1.7472034950333,-1.,-0.163814161002002));
#29488=CARTESIAN_POINT('Ctrl Pts',(1.7472034950333,1.,-0.163814161002002));
#29489=CARTESIAN_POINT('Ctrl Pts',(1.74236521665491,-1.,-0.163289472382896));
#29490=CARTESIAN_POINT('Ctrl Pts',(1.74236521665491,1.,-0.163289472382896));
#29491=CARTESIAN_POINT('',(2.19890268624765,1.,-0.0694764450219582));
#29492=CARTESIAN_POINT('Ctrl Pts',(2.19890268624765,1.,-0.0694764450219582));
#29493=CARTESIAN_POINT('Ctrl Pts',(2.19777582085423,1.,-0.0701143536325491));
#29494=CARTESIAN_POINT('Ctrl Pts',(2.19552129484002,1.,-0.0713863779526155));
#29495=CARTESIAN_POINT('Ctrl Pts',(2.19213712013662,1.,-0.0732830357306726));
#29496=CARTESIAN_POINT('Ctrl Pts',(2.1876201139953,1.,-0.0757891465836149));
#29497=CARTESIAN_POINT('Ctrl Pts',(2.18196589448887,1.,-0.0788837727685244));
#29498=CARTESIAN_POINT('Ctrl Pts',(2.176303712113,1.,-0.0819402680872767));
#29499=CARTESIAN_POINT('Ctrl Pts',(2.17063357870952,1.,-0.0849584620835374));
#29500=CARTESIAN_POINT('Ctrl Pts',(2.16495552645014,1.,-0.0879381291386924));
#29501=CARTESIAN_POINT('Ctrl Pts',(2.15926961544516,1.,-0.0908789888107267));
#29502=CARTESIAN_POINT('Ctrl Pts',(2.1535759397817,1.,-0.0937807218867645));
#29503=CARTESIAN_POINT('Ctrl Pts',(2.14787463531795,1.,-0.096642985230546));
#29504=CARTESIAN_POINT('Ctrl Pts',(2.14216588396025,1.,-0.0994654261990917));
#29505=CARTESIAN_POINT('Ctrl Pts',(2.13644992667165,1.,-0.102247700556101));
#29506=CARTESIAN_POINT('Ctrl Pts',(2.13072704887293,1.,-0.10498947915274));
#29507=CARTESIAN_POINT('Ctrl Pts',(2.12499752307,1.,-0.10769043523109));
#29508=CARTESIAN_POINT('Ctrl Pts',(2.11926155590865,1.,-0.110350236135025));
#29509=CARTESIAN_POINT('Ctrl Pts',(2.11351924490306,1.,-0.112968534419737));
#29510=CARTESIAN_POINT('Ctrl Pts',(2.10777050261309,1.,-0.115544957687927));
#29511=CARTESIAN_POINT('Ctrl Pts',(2.102015121329,1.,-0.118079107988356));
#29512=CARTESIAN_POINT('Ctrl Pts',(2.0962529286773,1.,-0.120570567965122));
#29513=CARTESIAN_POINT('Ctrl Pts',(2.09048392424825,1.,-0.123018905621083));
#29514=CARTESIAN_POINT('Ctrl Pts',(2.08470840653643,1.,-0.125423679412062));
#29515=CARTESIAN_POINT('Ctrl Pts',(2.07892715110987,1.,-0.12778444527612));
#29516=CARTESIAN_POINT('Ctrl Pts',(2.07314114713063,1.,-0.130100748328404));
#29517=CARTESIAN_POINT('Ctrl Pts',(2.06735123910326,1.,-0.132372111547711));
#29518=CARTESIAN_POINT('Ctrl Pts',(2.06155781517842,1.,-0.134598026192106));
#29519=CARTESIAN_POINT('Ctrl Pts',(2.05576044414264,1.,-0.136777941218044));
#29520=CARTESIAN_POINT('Ctrl Pts',(2.04995762001328,1.,-0.138911255368966));
#29521=CARTESIAN_POINT('Ctrl Pts',(2.04414757947916,1.,-0.140997332152546));
#29522=CARTESIAN_POINT('Ctrl Pts',(2.03832911025912,1.,-0.143035515058209));
#29523=CARTESIAN_POINT('Ctrl Pts',(2.03250223739942,1.,-0.145025140186058));
#29524=CARTESIAN_POINT('Ctrl Pts',(2.02666926182017,1.,-0.146965557332583));
#29525=CARTESIAN_POINT('Ctrl Pts',(2.02083464969894,1.,-0.148856124775337));
#29526=CARTESIAN_POINT('Ctrl Pts',(2.01500291940238,1.,-0.150696157673078));
#29527=CARTESIAN_POINT('Ctrl Pts',(2.00917680318424,1.,-0.15248488362145));
#29528=CARTESIAN_POINT('Ctrl Pts',(2.00335565310543,1.,-0.154221403049722));
#29529=CARTESIAN_POINT('Ctrl Pts',(1.99753284771497,1.,-0.155904629548784));
#29530=CARTESIAN_POINT('Ctrl Pts',(1.99169810931908,1.,-0.157533331459227));
#29531=CARTESIAN_POINT('Ctrl Pts',(1.98584238283292,1.,-0.159106226437299));
#29532=CARTESIAN_POINT('Ctrl Pts',(1.97996195437559,1.,-0.160622060784611));
#29533=CARTESIAN_POINT('Ctrl Pts',(1.97406280235188,1.,-0.162079693556289));
#29534=CARTESIAN_POINT('Ctrl Pts',(1.96816512677967,1.,-0.163478185457734));
#29535=CARTESIAN_POINT('Ctrl Pts',(1.96229379940136,1.,-0.164816568920269));
#29536=CARTESIAN_POINT('Ctrl Pts',(1.9564675971873,1.,-0.166093592002813));
#29537=CARTESIAN_POINT('Ctrl Pts',(1.95069027794294,1.,-0.167307501784476));
#29538=CARTESIAN_POINT('Ctrl Pts',(1.94493757756931,1.,-0.168455741607556));
#29539=CARTESIAN_POINT('Ctrl Pts',(1.93915639211581,1.,-0.169534904817491));
#29540=CARTESIAN_POINT('Ctrl Pts',(1.93329183155539,1.,-0.170541253116202));
#29541=CARTESIAN_POINT('Ctrl Pts',(1.92731093582036,1.,-0.171471191532988));
#29542=CARTESIAN_POINT('Ctrl Pts',(1.9212233439798,1.,-0.172321621259514));
#29543=CARTESIAN_POINT('Ctrl Pts',(1.91511429159527,1.,-0.173090695383496));
#29544=CARTESIAN_POINT('Ctrl Pts',(1.90911693975267,1.,-0.173776635257817));
#29545=CARTESIAN_POINT('Ctrl Pts',(1.90335253862834,1.,-0.174375518661085));
#29546=CARTESIAN_POINT('Ctrl Pts',(1.89788101117132,1.,-0.174879405091263));
#29547=CARTESIAN_POINT('Ctrl Pts',(1.892646301985,1.,-0.175274276190844));
#29548=CARTESIAN_POINT('Ctrl Pts',(1.88742606273259,1.,-0.175538155840648));
#29549=CARTESIAN_POINT('Ctrl Pts',(1.88188663145367,1.,-0.175644148889699));
#29550=CARTESIAN_POINT('Ctrl Pts',(1.87563767773588,1.,-0.175563480746485));
#29551=CARTESIAN_POINT('Ctrl Pts',(1.86828349694799,1.,-0.175268337590758));
#29552=CARTESIAN_POINT('Ctrl Pts',(1.85948367088837,1.,-0.17473525927603));
#29553=CARTESIAN_POINT('Ctrl Pts',(1.8489811319852,1.,-0.173946627587732));
#29554=CARTESIAN_POINT('Ctrl Pts',(1.83658380527692,1.,-0.1728894428919));
#29555=CARTESIAN_POINT('Ctrl Pts',(1.82215766811545,1.,-0.171554770204119));
#29556=CARTESIAN_POINT('Ctrl Pts',(1.80561530629706,1.,-0.169936923904608));
#29557=CARTESIAN_POINT('Ctrl Pts',(1.7869064998507,1.,-0.168032772805197));
#29558=CARTESIAN_POINT('Ctrl Pts',(1.77018771684844,1.,-0.1662793551464));
#29559=CARTESIAN_POINT('Ctrl Pts',(1.75666056638427,1.,-0.164834765707159));
#29560=CARTESIAN_POINT('Ctrl Pts',(1.7472034950333,1.,-0.163814161002002));
#29561=CARTESIAN_POINT('Ctrl Pts',(1.74236521665491,1.,-0.163289472382896));
#29562=CARTESIAN_POINT('',(2.19890268624765,0.,-0.0694764450219582));
#29563=CARTESIAN_POINT('Origin',(2.19890268624765,0.,0.0694764450219582));
#29564=CARTESIAN_POINT('',(2.19890268624765,1.,0.0694764450219582));
#29565=CARTESIAN_POINT('',(2.19890268624765,1.,-0.0694764450219582));
#29566=CARTESIAN_POINT('',(2.19890268624765,0.,0.0694764450219582));
#29567=CARTESIAN_POINT('Ctrl Pts',(1.74236521665491,-1.,0.163289472382896));
#29568=CARTESIAN_POINT('Ctrl Pts',(1.74236521665491,1.,0.163289472382896));
#29569=CARTESIAN_POINT('Ctrl Pts',(1.74720349503904,-1.,0.163814161002474));
#29570=CARTESIAN_POINT('Ctrl Pts',(1.74720349503904,1.,0.163814161002474));
#29571=CARTESIAN_POINT('Ctrl Pts',(1.75666056640041,-1.,0.164834765708484));
#29572=CARTESIAN_POINT('Ctrl Pts',(1.75666056640041,1.,0.164834765708484));
#29573=CARTESIAN_POINT('Ctrl Pts',(1.77018771687692,-1.,0.166279355148738));
#29574=CARTESIAN_POINT('Ctrl Pts',(1.77018771687692,1.,0.166279355148738));
#29575=CARTESIAN_POINT('Ctrl Pts',(1.78690649988931,-1.,0.16803277280837));
#29576=CARTESIAN_POINT('Ctrl Pts',(1.78690649988931,1.,0.16803277280837));
#29577=CARTESIAN_POINT('Ctrl Pts',(1.80561530633924,-1.,0.169936923908078));
#29578=CARTESIAN_POINT('Ctrl Pts',(1.80561530633924,1.,0.169936923908078));
#29579=CARTESIAN_POINT('Ctrl Pts',(1.82215766815414,-1.,0.171554770207306));
#29580=CARTESIAN_POINT('Ctrl Pts',(1.82215766815414,1.,0.171554770207306));
#29581=CARTESIAN_POINT('Ctrl Pts',(1.83658380530747,-1.,0.17288944289442));
#29582=CARTESIAN_POINT('Ctrl Pts',(1.83658380530747,1.,0.17288944289442));
#29583=CARTESIAN_POINT('Ctrl Pts',(1.84898113200543,-1.,0.173946627589401));
#29584=CARTESIAN_POINT('Ctrl Pts',(1.84898113200543,1.,0.173946627589401));
#29585=CARTESIAN_POINT('Ctrl Pts',(1.85948367089838,-1.,0.174735259276856));
#29586=CARTESIAN_POINT('Ctrl Pts',(1.85948367089838,1.,0.174735259276856));
#29587=CARTESIAN_POINT('Ctrl Pts',(1.86828349694972,-1.,0.1752683375909));
#29588=CARTESIAN_POINT('Ctrl Pts',(1.86828349694972,1.,0.1752683375909));
#29589=CARTESIAN_POINT('Ctrl Pts',(1.87563767773249,-1.,0.175563480746205));
#29590=CARTESIAN_POINT('Ctrl Pts',(1.87563767773249,1.,0.175563480746205));
#29591=CARTESIAN_POINT('Ctrl Pts',(1.88188663144846,-1.,0.175644148889271));
#29592=CARTESIAN_POINT('Ctrl Pts',(1.88188663144846,1.,0.175644148889271));
#29593=CARTESIAN_POINT('Ctrl Pts',(1.88742606272818,-1.,0.175538155840286));
#29594=CARTESIAN_POINT('Ctrl Pts',(1.88742606272818,1.,0.175538155840286));
#29595=CARTESIAN_POINT('Ctrl Pts',(1.89264630198279,-1.,0.175274276190664));
#29596=CARTESIAN_POINT('Ctrl Pts',(1.89264630198279,1.,0.175274276190664));
#29597=CARTESIAN_POINT('Ctrl Pts',(1.89788101117148,-1.,0.174879405091277));
#29598=CARTESIAN_POINT('Ctrl Pts',(1.89788101117148,1.,0.174879405091277));
#29599=CARTESIAN_POINT('Ctrl Pts',(1.90335253863003,-1.,0.174375518661222));
#29600=CARTESIAN_POINT('Ctrl Pts',(1.90335253863003,1.,0.174375518661222));
#29601=CARTESIAN_POINT('Ctrl Pts',(1.90911693975475,-1.,0.173776635257983));
#29602=CARTESIAN_POINT('Ctrl Pts',(1.90911693975475,1.,0.173776635257983));
#29603=CARTESIAN_POINT('Ctrl Pts',(1.91511429159681,-1.,0.173090695383619));
#29604=CARTESIAN_POINT('Ctrl Pts',(1.91511429159681,1.,0.173090695383619));
#29605=CARTESIAN_POINT('Ctrl Pts',(1.92122334398034,-1.,0.172321621259556));
#29606=CARTESIAN_POINT('Ctrl Pts',(1.92122334398034,1.,0.172321621259556));
#29607=CARTESIAN_POINT('Ctrl Pts',(1.92731093582,-1.,0.17147119153296));
#29608=CARTESIAN_POINT('Ctrl Pts',(1.92731093582,1.,0.17147119153296));
#29609=CARTESIAN_POINT('Ctrl Pts',(1.93329183155455,-1.,0.170541253116136));
#29610=CARTESIAN_POINT('Ctrl Pts',(1.93329183155455,1.,0.170541253116136));
#29611=CARTESIAN_POINT('Ctrl Pts',(1.93915639211497,-1.,0.169534904817425));
#29612=CARTESIAN_POINT('Ctrl Pts',(1.93915639211497,1.,0.169534904817425));
#29613=CARTESIAN_POINT('Ctrl Pts',(1.94493757756879,-1.,0.168455741607515));
#29614=CARTESIAN_POINT('Ctrl Pts',(1.94493757756879,1.,0.168455741607515));
#29615=CARTESIAN_POINT('Ctrl Pts',(1.95069027794286,-1.,0.167307501784469));
#29616=CARTESIAN_POINT('Ctrl Pts',(1.95069027794286,1.,0.167307501784469));
#29617=CARTESIAN_POINT('Ctrl Pts',(1.95646759718755,-1.,0.166093592002832));
#29618=CARTESIAN_POINT('Ctrl Pts',(1.95646759718755,1.,0.166093592002832));
#29619=CARTESIAN_POINT('Ctrl Pts',(1.96229379940174,-1.,0.1648165689203));
#29620=CARTESIAN_POINT('Ctrl Pts',(1.96229379940174,1.,0.1648165689203));
#29621=CARTESIAN_POINT('Ctrl Pts',(1.96816512678,-1.,0.16347818545776));
#29622=CARTESIAN_POINT('Ctrl Pts',(1.96816512678,1.,0.16347818545776));
#29623=CARTESIAN_POINT('Ctrl Pts',(1.97406280235204,-1.,0.162079693556302));
#29624=CARTESIAN_POINT('Ctrl Pts',(1.97406280235204,1.,0.162079693556302));
#29625=CARTESIAN_POINT('Ctrl Pts',(1.97996195437557,-1.,0.16062206078461));
#29626=CARTESIAN_POINT('Ctrl Pts',(1.97996195437557,1.,0.16062206078461));
#29627=CARTESIAN_POINT('Ctrl Pts',(1.98584238283279,-1.,0.159106226437288));
#29628=CARTESIAN_POINT('Ctrl Pts',(1.98584238283279,1.,0.159106226437288));
#29629=CARTESIAN_POINT('Ctrl Pts',(1.99169810931893,-1.,0.157533331459215));
#29630=CARTESIAN_POINT('Ctrl Pts',(1.99169810931893,1.,0.157533331459215));
#29631=CARTESIAN_POINT('Ctrl Pts',(1.99753284771487,-1.,0.155904629548774));
#29632=CARTESIAN_POINT('Ctrl Pts',(1.99753284771487,1.,0.155904629548774));
#29633=CARTESIAN_POINT('Ctrl Pts',(2.00335565310539,-1.,0.154221403049719));
#29634=CARTESIAN_POINT('Ctrl Pts',(2.00335565310539,1.,0.154221403049719));
#29635=CARTESIAN_POINT('Ctrl Pts',(2.00917680318426,-1.,0.152484883621452));
#29636=CARTESIAN_POINT('Ctrl Pts',(2.00917680318426,1.,0.152484883621452));
#29637=CARTESIAN_POINT('Ctrl Pts',(2.01500291940243,-1.,0.150696157673084));
#29638=CARTESIAN_POINT('Ctrl Pts',(2.01500291940243,1.,0.150696157673084));
#29639=CARTESIAN_POINT('Ctrl Pts',(2.02083464969897,-1.,0.148856124775342));
#29640=CARTESIAN_POINT('Ctrl Pts',(2.02083464969897,1.,0.148856124775342));
#29641=CARTESIAN_POINT('Ctrl Pts',(2.02666926182017,-1.,0.146965557332586));
#29642=CARTESIAN_POINT('Ctrl Pts',(2.02666926182017,1.,0.146965557332586));
#29643=CARTESIAN_POINT('Ctrl Pts',(2.03250223739941,-1.,0.145025140186058));
#29644=CARTESIAN_POINT('Ctrl Pts',(2.03250223739941,1.,0.145025140186058));
#29645=CARTESIAN_POINT('Ctrl Pts',(2.03832911025913,-1.,0.143035515058208));
#29646=CARTESIAN_POINT('Ctrl Pts',(2.03832911025913,1.,0.143035515058208));
#29647=CARTESIAN_POINT('Ctrl Pts',(2.04414757947919,-1.,0.140997332152545));
#29648=CARTESIAN_POINT('Ctrl Pts',(2.04414757947919,1.,0.140997332152545));
#29649=CARTESIAN_POINT('Ctrl Pts',(2.04995762001333,-1.,0.138911255368966));
#29650=CARTESIAN_POINT('Ctrl Pts',(2.04995762001333,1.,0.138911255368966));
#29651=CARTESIAN_POINT('Ctrl Pts',(2.0557604441427,-1.,0.136777941218044));
#29652=CARTESIAN_POINT('Ctrl Pts',(2.0557604441427,1.,0.136777941218044));
#29653=CARTESIAN_POINT('Ctrl Pts',(2.06155781517844,-1.,0.134598026192107));
#29654=CARTESIAN_POINT('Ctrl Pts',(2.06155781517844,1.,0.134598026192107));
#29655=CARTESIAN_POINT('Ctrl Pts',(2.06735123910319,-1.,0.132372111547709));
#29656=CARTESIAN_POINT('Ctrl Pts',(2.06735123910319,1.,0.132372111547709));
#29657=CARTESIAN_POINT('Ctrl Pts',(2.07314114713047,-1.,0.1301007483284));
#29658=CARTESIAN_POINT('Ctrl Pts',(2.07314114713047,1.,0.1301007483284));
#29659=CARTESIAN_POINT('Ctrl Pts',(2.07892715110967,-1.,0.127784445276116));
#29660=CARTESIAN_POINT('Ctrl Pts',(2.07892715110967,1.,0.127784445276116));
#29661=CARTESIAN_POINT('Ctrl Pts',(2.08470840653628,-1.,0.125423679412058));
#29662=CARTESIAN_POINT('Ctrl Pts',(2.08470840653628,1.,0.125423679412058));
#29663=CARTESIAN_POINT('Ctrl Pts',(2.09048392424826,-1.,0.123018905621083));
#29664=CARTESIAN_POINT('Ctrl Pts',(2.09048392424826,1.,0.123018905621083));
#29665=CARTESIAN_POINT('Ctrl Pts',(2.09625292867756,-1.,0.120570567965129));
#29666=CARTESIAN_POINT('Ctrl Pts',(2.09625292867756,1.,0.120570567965129));
#29667=CARTESIAN_POINT('Ctrl Pts',(2.10201512132945,-1.,0.118079107988368));
#29668=CARTESIAN_POINT('Ctrl Pts',(2.10201512132945,1.,0.118079107988368));
#29669=CARTESIAN_POINT('Ctrl Pts',(2.10777050261359,-1.,0.11554495768794));
#29670=CARTESIAN_POINT('Ctrl Pts',(2.10777050261359,1.,0.11554495768794));
#29671=CARTESIAN_POINT('Ctrl Pts',(2.11351924490335,-1.,0.112968534419746));
#29672=CARTESIAN_POINT('Ctrl Pts',(2.11351924490335,1.,0.112968534419746));
#29673=CARTESIAN_POINT('Ctrl Pts',(2.11926155590849,-1.,0.11035023613502));
#29674=CARTESIAN_POINT('Ctrl Pts',(2.11926155590849,1.,0.11035023613502));
#29675=CARTESIAN_POINT('Ctrl Pts',(2.12499752306927,-1.,0.107690435231068));
#29676=CARTESIAN_POINT('Ctrl Pts',(2.12499752306927,1.,0.107690435231068));
#29677=CARTESIAN_POINT('Ctrl Pts',(2.1307270488718,-1.,0.104989479152703));
#29678=CARTESIAN_POINT('Ctrl Pts',(2.1307270488718,1.,0.104989479152703));
#29679=CARTESIAN_POINT('Ctrl Pts',(2.13644992667052,-1.,0.102247700556063));
#29680=CARTESIAN_POINT('Ctrl Pts',(2.13644992667052,1.,0.102247700556063));
#29681=CARTESIAN_POINT('Ctrl Pts',(2.14216588395974,-1.,0.0994654261990741));
#29682=CARTESIAN_POINT('Ctrl Pts',(2.14216588395974,1.,0.0994654261990741));
#29683=CARTESIAN_POINT('Ctrl Pts',(2.14787463531864,-1.,0.0966429852305688));
#29684=CARTESIAN_POINT('Ctrl Pts',(2.14787463531864,1.,0.0966429852305688));
#29685=CARTESIAN_POINT('Ctrl Pts',(2.15357593978377,-1.,0.0937807218868344));
#29686=CARTESIAN_POINT('Ctrl Pts',(2.15357593978377,1.,0.0937807218868344));
#29687=CARTESIAN_POINT('Ctrl Pts',(2.15926961544808,-1.,0.0908789888108265));
#29688=CARTESIAN_POINT('Ctrl Pts',(2.15926961544808,1.,0.0908789888108265));
#29689=CARTESIAN_POINT('Ctrl Pts',(2.16495552645275,-1.,0.0879381291387821));
#29690=CARTESIAN_POINT('Ctrl Pts',(2.16495552645275,1.,0.0879381291387821));
#29691=CARTESIAN_POINT('Ctrl Pts',(2.17063357871031,-1.,0.0849584620835642));
#29692=CARTESIAN_POINT('Ctrl Pts',(2.17063357871031,1.,0.0849584620835642));
#29693=CARTESIAN_POINT('Ctrl Pts',(2.1763037121106,-1.,0.0819402680871938));
#29694=CARTESIAN_POINT('Ctrl Pts',(2.1763037121106,1.,0.0819402680871938));
#29695=CARTESIAN_POINT('Ctrl Pts',(2.18196589448304,-1.,0.0788837727683226));
#29696=CARTESIAN_POINT('Ctrl Pts',(2.18196589448304,1.,0.0788837727683226));
#29697=CARTESIAN_POINT('Ctrl Pts',(2.1876201139874,-1.,0.075789146583341));
#29698=CARTESIAN_POINT('Ctrl Pts',(2.1876201139874,1.,0.075789146583341));
#29699=CARTESIAN_POINT('Ctrl Pts',(2.19213712012956,-1.,0.0732830357304275));
#29700=CARTESIAN_POINT('Ctrl Pts',(2.19213712012956,1.,0.0732830357304275));
#29701=CARTESIAN_POINT('Ctrl Pts',(2.19552129483562,-1.,0.0713863779524626));
#29702=CARTESIAN_POINT('Ctrl Pts',(2.19552129483562,1.,0.0713863779524626));
#29703=CARTESIAN_POINT('Ctrl Pts',(2.19777582085261,-1.,0.0701143536324925));
#29704=CARTESIAN_POINT('Ctrl Pts',(2.19777582085261,1.,0.0701143536324925));
#29705=CARTESIAN_POINT('Ctrl Pts',(2.19890268624765,-1.,0.0694764450219582));
#29706=CARTESIAN_POINT('Ctrl Pts',(2.19890268624765,1.,0.0694764450219582));
#29707=CARTESIAN_POINT('',(1.74236521665491,1.,0.163289472382896));
#29708=CARTESIAN_POINT('Ctrl Pts',(1.74236521665491,1.,0.163289472382896));
#29709=CARTESIAN_POINT('Ctrl Pts',(1.74720349503904,1.,0.163814161002474));
#29710=CARTESIAN_POINT('Ctrl Pts',(1.75666056640041,1.,0.164834765708484));
#29711=CARTESIAN_POINT('Ctrl Pts',(1.77018771687692,1.,0.166279355148738));
#29712=CARTESIAN_POINT('Ctrl Pts',(1.78690649988931,1.,0.16803277280837));
#29713=CARTESIAN_POINT('Ctrl Pts',(1.80561530633924,1.,0.169936923908078));
#29714=CARTESIAN_POINT('Ctrl Pts',(1.82215766815414,1.,0.171554770207306));
#29715=CARTESIAN_POINT('Ctrl Pts',(1.83658380530747,1.,0.17288944289442));
#29716=CARTESIAN_POINT('Ctrl Pts',(1.84898113200543,1.,0.173946627589401));
#29717=CARTESIAN_POINT('Ctrl Pts',(1.85948367089838,1.,0.174735259276856));
#29718=CARTESIAN_POINT('Ctrl Pts',(1.86828349694972,1.,0.1752683375909));
#29719=CARTESIAN_POINT('Ctrl Pts',(1.87563767773249,1.,0.175563480746205));
#29720=CARTESIAN_POINT('Ctrl Pts',(1.88188663144846,1.,0.175644148889271));
#29721=CARTESIAN_POINT('Ctrl Pts',(1.88742606272818,1.,0.175538155840286));
#29722=CARTESIAN_POINT('Ctrl Pts',(1.89264630198279,1.,0.175274276190664));
#29723=CARTESIAN_POINT('Ctrl Pts',(1.89788101117148,1.,0.174879405091277));
#29724=CARTESIAN_POINT('Ctrl Pts',(1.90335253863003,1.,0.174375518661222));
#29725=CARTESIAN_POINT('Ctrl Pts',(1.90911693975475,1.,0.173776635257983));
#29726=CARTESIAN_POINT('Ctrl Pts',(1.91511429159681,1.,0.173090695383619));
#29727=CARTESIAN_POINT('Ctrl Pts',(1.92122334398034,1.,0.172321621259556));
#29728=CARTESIAN_POINT('Ctrl Pts',(1.92731093582,1.,0.17147119153296));
#29729=CARTESIAN_POINT('Ctrl Pts',(1.93329183155455,1.,0.170541253116136));
#29730=CARTESIAN_POINT('Ctrl Pts',(1.93915639211497,1.,0.169534904817425));
#29731=CARTESIAN_POINT('Ctrl Pts',(1.94493757756879,1.,0.168455741607515));
#29732=CARTESIAN_POINT('Ctrl Pts',(1.95069027794286,1.,0.167307501784469));
#29733=CARTESIAN_POINT('Ctrl Pts',(1.95646759718755,1.,0.166093592002832));
#29734=CARTESIAN_POINT('Ctrl Pts',(1.96229379940174,1.,0.1648165689203));
#29735=CARTESIAN_POINT('Ctrl Pts',(1.96816512678,1.,0.16347818545776));
#29736=CARTESIAN_POINT('Ctrl Pts',(1.97406280235204,1.,0.162079693556302));
#29737=CARTESIAN_POINT('Ctrl Pts',(1.97996195437557,1.,0.16062206078461));
#29738=CARTESIAN_POINT('Ctrl Pts',(1.98584238283279,1.,0.159106226437288));
#29739=CARTESIAN_POINT('Ctrl Pts',(1.99169810931893,1.,0.157533331459215));
#29740=CARTESIAN_POINT('Ctrl Pts',(1.99753284771487,1.,0.155904629548774));
#29741=CARTESIAN_POINT('Ctrl Pts',(2.00335565310539,1.,0.154221403049719));
#29742=CARTESIAN_POINT('Ctrl Pts',(2.00917680318426,1.,0.152484883621452));
#29743=CARTESIAN_POINT('Ctrl Pts',(2.01500291940243,1.,0.150696157673084));
#29744=CARTESIAN_POINT('Ctrl Pts',(2.02083464969897,1.,0.148856124775342));
#29745=CARTESIAN_POINT('Ctrl Pts',(2.02666926182017,1.,0.146965557332586));
#29746=CARTESIAN_POINT('Ctrl Pts',(2.03250223739941,1.,0.145025140186058));
#29747=CARTESIAN_POINT('Ctrl Pts',(2.03832911025913,1.,0.143035515058208));
#29748=CARTESIAN_POINT('Ctrl Pts',(2.04414757947919,1.,0.140997332152545));
#29749=CARTESIAN_POINT('Ctrl Pts',(2.04995762001333,1.,0.138911255368966));
#29750=CARTESIAN_POINT('Ctrl Pts',(2.0557604441427,1.,0.136777941218044));
#29751=CARTESIAN_POINT('Ctrl Pts',(2.06155781517844,1.,0.134598026192107));
#29752=CARTESIAN_POINT('Ctrl Pts',(2.06735123910319,1.,0.132372111547709));
#29753=CARTESIAN_POINT('Ctrl Pts',(2.07314114713047,1.,0.1301007483284));
#29754=CARTESIAN_POINT('Ctrl Pts',(2.07892715110967,1.,0.127784445276116));
#29755=CARTESIAN_POINT('Ctrl Pts',(2.08470840653628,1.,0.125423679412058));
#29756=CARTESIAN_POINT('Ctrl Pts',(2.09048392424826,1.,0.123018905621083));
#29757=CARTESIAN_POINT('Ctrl Pts',(2.09625292867756,1.,0.120570567965129));
#29758=CARTESIAN_POINT('Ctrl Pts',(2.10201512132945,1.,0.118079107988368));
#29759=CARTESIAN_POINT('Ctrl Pts',(2.10777050261359,1.,0.11554495768794));
#29760=CARTESIAN_POINT('Ctrl Pts',(2.11351924490335,1.,0.112968534419746));
#29761=CARTESIAN_POINT('Ctrl Pts',(2.11926155590849,1.,0.11035023613502));
#29762=CARTESIAN_POINT('Ctrl Pts',(2.12499752306927,1.,0.107690435231068));
#29763=CARTESIAN_POINT('Ctrl Pts',(2.1307270488718,1.,0.104989479152703));
#29764=CARTESIAN_POINT('Ctrl Pts',(2.13644992667052,1.,0.102247700556063));
#29765=CARTESIAN_POINT('Ctrl Pts',(2.14216588395974,1.,0.0994654261990741));
#29766=CARTESIAN_POINT('Ctrl Pts',(2.14787463531864,1.,0.0966429852305688));
#29767=CARTESIAN_POINT('Ctrl Pts',(2.15357593978377,1.,0.0937807218868344));
#29768=CARTESIAN_POINT('Ctrl Pts',(2.15926961544808,1.,0.0908789888108265));
#29769=CARTESIAN_POINT('Ctrl Pts',(2.16495552645275,1.,0.0879381291387821));
#29770=CARTESIAN_POINT('Ctrl Pts',(2.17063357871031,1.,0.0849584620835642));
#29771=CARTESIAN_POINT('Ctrl Pts',(2.1763037121106,1.,0.0819402680871938));
#29772=CARTESIAN_POINT('Ctrl Pts',(2.18196589448304,1.,0.0788837727683226));
#29773=CARTESIAN_POINT('Ctrl Pts',(2.1876201139874,1.,0.075789146583341));
#29774=CARTESIAN_POINT('Ctrl Pts',(2.19213712012956,1.,0.0732830357304275));
#29775=CARTESIAN_POINT('Ctrl Pts',(2.19552129483562,1.,0.0713863779524626));
#29776=CARTESIAN_POINT('Ctrl Pts',(2.19777582085261,1.,0.0701143536324925));
#29777=CARTESIAN_POINT('Ctrl Pts',(2.19890268624765,1.,0.0694764450219582));
#29778=CARTESIAN_POINT('',(1.74236521665491,0.,0.163289472382896));
#29779=CARTESIAN_POINT('Origin',(0.,1.,0.));
#29780=CARTESIAN_POINT('Origin',(0.,1.,0.));
#29781=CARTESIAN_POINT('Origin',(0.,0.,0.));
#29782=CARTESIAN_POINT('',(0.,0.,0.));
#29783=CARTESIAN_POINT('Origin',(0.525,0.18,0.38));
#29784=CARTESIAN_POINT('',(-1.05,0.2,0.36));
#29785=CARTESIAN_POINT('',(-1.05,0.16,0.4));
#29786=CARTESIAN_POINT('',(-1.05,0.2,0.36));
#29787=CARTESIAN_POINT('',(1.05,0.16,0.4));
#29788=CARTESIAN_POINT('',(0.525,0.16,0.4));
#29789=CARTESIAN_POINT('',(1.05,0.2,0.36));
#29790=CARTESIAN_POINT('',(1.05,0.16,0.4));
#29791=CARTESIAN_POINT('',(0.525,0.2,0.36));
#29792=CARTESIAN_POINT('Origin',(-1.05,0.,0.38));
#29793=CARTESIAN_POINT('',(-1.05,-0.2,0.36));
#29794=CARTESIAN_POINT('',(-1.05,-0.16,0.4));
#29795=CARTESIAN_POINT('',(-1.05,-0.2,0.36));
#29796=CARTESIAN_POINT('Origin',(-1.05,0.,0.4));
#29797=CARTESIAN_POINT('Origin',(-1.05,0.,0.36));
#29798=CARTESIAN_POINT('Origin',(-0.525,-0.18,0.38));
#29799=CARTESIAN_POINT('',(1.05,-0.2,0.36));
#29800=CARTESIAN_POINT('',(1.05,-0.16,0.4));
#29801=CARTESIAN_POINT('',(1.05,-0.2,0.36));
#29802=CARTESIAN_POINT('',(-0.525,-0.16,0.4));
#29803=CARTESIAN_POINT('',(-0.525,-0.2,0.36));
#29804=CARTESIAN_POINT('Origin',(1.05,0.,0.38));
#29805=CARTESIAN_POINT('Origin',(1.05,0.,0.4));
#29806=CARTESIAN_POINT('Origin',(1.05,0.,0.36));
#29807=CARTESIAN_POINT('Origin',(-1.05,0.,0.));
#29808=CARTESIAN_POINT('',(-1.05,0.2,0.04));
#29809=CARTESIAN_POINT('',(-1.05,0.2,0.));
#29810=CARTESIAN_POINT('',(-1.05,-0.2,0.04));
#29811=CARTESIAN_POINT('Origin',(-1.05,0.,0.04));
#29812=CARTESIAN_POINT('',(-1.05,-0.2,0.));
#29813=CARTESIAN_POINT('Origin',(1.05,0.2,0.));
#29814=CARTESIAN_POINT('',(1.05,0.2,0.04));
#29815=CARTESIAN_POINT('',(1.05,0.2,0.));
#29816=CARTESIAN_POINT('',(0.525,0.2,0.04));
#29817=CARTESIAN_POINT('Origin',(0.,0.,0.4));
#29818=CARTESIAN_POINT('Origin',(0.525,0.18,0.02));
#29819=CARTESIAN_POINT('',(-1.05,0.16,0.));
#29820=CARTESIAN_POINT('',(-1.05,0.16,0.));
#29821=CARTESIAN_POINT('',(1.05,0.16,0.));
#29822=CARTESIAN_POINT('',(1.05,0.2,0.04));
#29823=CARTESIAN_POINT('',(0.525,0.16,0.));
#29824=CARTESIAN_POINT('Origin',(-1.05,0.,0.02));
#29825=CARTESIAN_POINT('',(-1.05,-0.16,0.));
#29826=CARTESIAN_POINT('',(-1.05,-0.16,0.));
#29827=CARTESIAN_POINT('Origin',(-1.05,0.,0.));
#29828=CARTESIAN_POINT('Origin',(-0.525,-0.18,0.02));
#29829=CARTESIAN_POINT('',(1.05,-0.16,0.));
#29830=CARTESIAN_POINT('',(1.05,-0.2,0.04));
#29831=CARTESIAN_POINT('',(1.05,-0.16,0.));
#29832=CARTESIAN_POINT('',(-0.525,-0.2,0.04));
#29833=CARTESIAN_POINT('',(-0.525,-0.16,0.));
#29834=CARTESIAN_POINT('Origin',(1.05,0.,0.02));
#29835=CARTESIAN_POINT('Origin',(1.05,0.,0.04));
#29836=CARTESIAN_POINT('Origin',(1.05,0.,0.));
#29837=CARTESIAN_POINT('Origin',(1.05,0.,0.));
#29838=CARTESIAN_POINT('',(1.05,-0.2,0.));
#29839=CARTESIAN_POINT('Origin',(0.,0.,0.));
#29840=CARTESIAN_POINT('Origin',(-1.05,-0.2,0.));
#29841=CARTESIAN_POINT('',(0.,0.,0.));
#29842=CARTESIAN_POINT('',(0.,0.,0.));
#29843=CARTESIAN_POINT('Origin',(-0.3,-0.9,-1.1));
#29844=CARTESIAN_POINT('',(-0.3,2.1,-0.953939201416946));
#29845=CARTESIAN_POINT('',(-0.3,-0.9,-0.953939201416946));
#29846=CARTESIAN_POINT('',(-0.3,-6.,-0.953939201416946));
#29847=CARTESIAN_POINT('',(-0.3,2.1,-0.65));
#29848=CARTESIAN_POINT('',(-0.3,2.1,-0.65));
#29849=CARTESIAN_POINT('',(-0.3,-0.9,-0.65));
#29850=CARTESIAN_POINT('',(-0.3,-0.9,-0.65));
#29851=CARTESIAN_POINT('',(-0.3,-0.9,-0.65));
#29852=CARTESIAN_POINT('Origin',(0.,-0.9,-0.875));
#29853=CARTESIAN_POINT('',(0.3,-0.9,-0.953939201416946));
#29854=CARTESIAN_POINT('Origin',(0.,-0.9,0.));
#29855=CARTESIAN_POINT('',(0.3,-0.9,-0.65));
#29856=CARTESIAN_POINT('',(0.3,-0.9,-0.65));
#29857=CARTESIAN_POINT('',(0.3,-0.9,-1.1));
#29858=CARTESIAN_POINT('Origin',(0.3,-0.9,-0.65));
#29859=CARTESIAN_POINT('',(0.3,2.1,-0.953939201416946));
#29860=CARTESIAN_POINT('',(0.3,-6.,-0.953939201416946));
#29861=CARTESIAN_POINT('',(0.3,2.1,-0.65));
#29862=CARTESIAN_POINT('',(0.3,-0.9,-0.65));
#29863=CARTESIAN_POINT('',(0.3,2.1,-1.1));
#29864=CARTESIAN_POINT('Origin',(-0.3,-0.9,-0.65));
#29865=CARTESIAN_POINT('',(0.3,2.1,-0.65));
#29866=CARTESIAN_POINT('Origin',(0.,2.1,-0.875));
#29867=CARTESIAN_POINT('Origin',(0.,2.1,0.));
#29868=CARTESIAN_POINT('Origin',(0.,-6.,0.));
#29869=CARTESIAN_POINT('',(-1.,6.5,1.22464679914735E-16));
#29870=CARTESIAN_POINT('Origin',(0.,6.5,0.));
#29871=CARTESIAN_POINT('',(-1.,-6.,1.22464679914735E-16));
#29872=CARTESIAN_POINT('',(-1.,-6.,1.22464679914735E-16));
#29873=CARTESIAN_POINT('Origin',(0.,-6.,0.));
#29874=CARTESIAN_POINT('Origin',(0.,6.5,0.));
#29875=CARTESIAN_POINT('Origin',(0.,-6.,0.));
#29876=CARTESIAN_POINT('',(0.,0.,0.));
#29877=CARTESIAN_POINT('Origin',(0.,-2.8,0.));
#29878=CARTESIAN_POINT('',(-1.01,-1.,1.23689326713883E-16));
#29879=CARTESIAN_POINT('Origin',(0.,-1.,0.));
#29880=CARTESIAN_POINT('',(-1.01,-2.8,1.23689326713883E-16));
#29881=CARTESIAN_POINT('',(-1.01,-2.8,1.23689326713883E-16));
#29882=CARTESIAN_POINT('Origin',(0.,-2.8,0.));
#29883=CARTESIAN_POINT('Origin',(0.,-2.8,0.));
#29884=CARTESIAN_POINT('',(-1.35,-1.,1.65327317884893E-16));
#29885=CARTESIAN_POINT('Origin',(0.,-1.,0.));
#29886=CARTESIAN_POINT('',(-1.35,-2.8,1.65327317884893E-16));
#29887=CARTESIAN_POINT('',(-1.35,-2.8,1.65327317884893E-16));
#29888=CARTESIAN_POINT('Origin',(0.,-2.8,0.));
#29889=CARTESIAN_POINT('Origin',(0.,-1.,0.));
#29890=CARTESIAN_POINT('Origin',(0.,-2.8,0.));
#29891=CARTESIAN_POINT('',(0.,0.,0.));
#29892=CARTESIAN_POINT('Origin',(0.,2.2,0.));
#29893=CARTESIAN_POINT('',(-1.01,2.8,1.23689326713883E-16));
#29894=CARTESIAN_POINT('Origin',(0.,2.8,0.));
#29895=CARTESIAN_POINT('',(-1.01,2.2,1.23689326713883E-16));
#29896=CARTESIAN_POINT('',(-1.01,2.2,1.23689326713883E-16));
#29897=CARTESIAN_POINT('Origin',(0.,2.2,0.));
#29898=CARTESIAN_POINT('Origin',(0.,2.2,0.));
#29899=CARTESIAN_POINT('',(-1.35,2.8,1.65327317884893E-16));
#29900=CARTESIAN_POINT('Origin',(0.,2.8,0.));
#29901=CARTESIAN_POINT('',(-1.35,2.2,1.65327317884893E-16));
#29902=CARTESIAN_POINT('',(-1.35,2.2,1.65327317884893E-16));
#29903=CARTESIAN_POINT('Origin',(0.,2.2,0.));
#29904=CARTESIAN_POINT('Origin',(0.,2.8,0.));
#29905=CARTESIAN_POINT('Origin',(0.,2.2,0.));
#29906=CARTESIAN_POINT('',(0.,0.,0.));
#29907=CARTESIAN_POINT('Origin',(0.,-5.1,0.99));
#29908=CARTESIAN_POINT('',(0.172988438920062,-5.21905880899791,0.99));
#29909=CARTESIAN_POINT('',(0.172988438920062,-4.98094119100209,0.99));
#29910=CARTESIAN_POINT('',(0.172988438920062,-5.5,0.99));
#29911=CARTESIAN_POINT('Origin',(0.,-5.1,0.99));
#29912=CARTESIAN_POINT('Origin',(0.,-5.1,0.99));
#29913=CARTESIAN_POINT('',(-0.172988438920062,-5.21905880899791,0.99));
#29914=CARTESIAN_POINT('Ctrl Pts',(-0.172988438920062,-5.21905880899791,
0.99));
#29915=CARTESIAN_POINT('Ctrl Pts',(-0.165594865311319,-5.22980142239529,
0.991291921976381));
#29916=CARTESIAN_POINT('Ctrl Pts',(-0.157297138725609,-5.23968770937274,
0.992653949439047));
#29917=CARTESIAN_POINT('Ctrl Pts',(-0.129892073845076,-5.26709277425327,
0.996748084390898));
#29918=CARTESIAN_POINT('Ctrl Pts',(-0.106330167759284,-5.28324205633295,
0.999695893276376));
#29919=CARTESIAN_POINT('Ctrl Pts',(-0.05461290463241,-5.30469779396491,
1.00385029472357));
#29920=CARTESIAN_POINT('Ctrl Pts',(-0.0264512308298516,-5.31,1.005));
#29921=CARTESIAN_POINT('Ctrl Pts',(0.0264512308298516,-5.31,1.005));
#29922=CARTESIAN_POINT('Ctrl Pts',(0.054612904632411,-5.30469779396491,
1.00385029472357));
#29923=CARTESIAN_POINT('Ctrl Pts',(0.106330167759285,-5.28324205633295,
0.999695893276376));
#29924=CARTESIAN_POINT('Ctrl Pts',(0.129892073845076,-5.26709277425327,
0.996748084390898));
#29925=CARTESIAN_POINT('Ctrl Pts',(0.157297138725609,-5.23968770937274,
0.992653949439047));
#29926=CARTESIAN_POINT('Ctrl Pts',(0.165594865311319,-5.22980142239529,
0.991291921976381));
#29927=CARTESIAN_POINT('Ctrl Pts',(0.172988438920062,-5.21905880899791,
0.99));
#29928=CARTESIAN_POINT('',(-0.21,-5.1,0.99));
#29929=CARTESIAN_POINT('Origin',(0.,-5.1,0.99));
#29930=CARTESIAN_POINT('',(-0.21,-5.1,1.58615888233178));
#29931=CARTESIAN_POINT('',(-0.21,-5.1,0.99));
#29932=CARTESIAN_POINT('',(0.21,-5.1,1.58615888233178));
#29933=CARTESIAN_POINT('Ctrl Pts',(0.21,-5.1,1.58615888233178));
#29934=CARTESIAN_POINT('Ctrl Pts',(0.21,-5.12640093420375,1.58615888233178));
#29935=CARTESIAN_POINT('Ctrl Pts',(0.20471752266132,-5.15454055536511,1.58688606295397));
#29936=CARTESIAN_POINT('Ctrl Pts',(0.183276841782292,-5.2062710523005,1.58950502964782));
#29937=CARTESIAN_POINT('Ctrl Pts',(0.167120287247804,-5.22986456085055,
1.59135816887013));
#29938=CARTESIAN_POINT('Ctrl Pts',(0.129864750292352,-5.267120097806,1.59483075953278));
#29939=CARTESIAN_POINT('Ctrl Pts',(0.106271159541076,-5.28327680083123,
1.59667690933009));
#29940=CARTESIAN_POINT('Ctrl Pts',(0.0545403836274689,-5.3047175903444,
1.59927985626981));
#29941=CARTESIAN_POINT('Ctrl Pts',(0.0264006657112964,-5.31,1.6));
#29942=CARTESIAN_POINT('Ctrl Pts',(-0.0264006657112964,-5.31,1.6));
#29943=CARTESIAN_POINT('Ctrl Pts',(-0.0545403836274682,-5.3047175903444,
1.59927985626981));
#29944=CARTESIAN_POINT('Ctrl Pts',(-0.106271159541075,-5.28327680083123,
1.59667690933009));
#29945=CARTESIAN_POINT('Ctrl Pts',(-0.129864750292352,-5.267120097806,1.59483075953278));
#29946=CARTESIAN_POINT('Ctrl Pts',(-0.167120287247804,-5.22986456085055,
1.59135816887013));
#29947=CARTESIAN_POINT('Ctrl Pts',(-0.183276841782292,-5.2062710523005,
1.58950502964782));
#29948=CARTESIAN_POINT('Ctrl Pts',(-0.20471752266132,-5.15454055536511,
1.58688606295397));
#29949=CARTESIAN_POINT('Ctrl Pts',(-0.21,-5.12640093420375,1.58615888233178));
#29950=CARTESIAN_POINT('Ctrl Pts',(-0.21,-5.1,1.58615888233178));
#29951=CARTESIAN_POINT('Ctrl Pts',(-0.21,-5.1,1.58615888233178));
#29952=CARTESIAN_POINT('Ctrl Pts',(-0.21,-5.07359906579625,1.58615888233178));
#29953=CARTESIAN_POINT('Ctrl Pts',(-0.20471752266132,-5.04545944463489,
1.58688606295397));
#29954=CARTESIAN_POINT('Ctrl Pts',(-0.183276841782292,-4.9937289476995,
1.58950502964782));
#29955=CARTESIAN_POINT('Ctrl Pts',(-0.167120287247804,-4.97013543914945,
1.59135816887013));
#29956=CARTESIAN_POINT('Ctrl Pts',(-0.129864750292352,-4.932879902194,1.59483075953278));
#29957=CARTESIAN_POINT('Ctrl Pts',(-0.106271159541076,-4.91672319916876,
1.59667690933009));
#29958=CARTESIAN_POINT('Ctrl Pts',(-0.0545403836274689,-4.8952824096556,
1.59927985626981));
#29959=CARTESIAN_POINT('Ctrl Pts',(-0.0264006657112965,-4.89,1.6));
#29960=CARTESIAN_POINT('Ctrl Pts',(0.0264006657112964,-4.89,1.6));
#29961=CARTESIAN_POINT('Ctrl Pts',(0.0545403836274682,-4.8952824096556,
1.59927985626981));
#29962=CARTESIAN_POINT('Ctrl Pts',(0.106271159541075,-4.91672319916876,
1.59667690933009));
#29963=CARTESIAN_POINT('Ctrl Pts',(0.129864750292352,-4.932879902194,1.59483075953278));
#29964=CARTESIAN_POINT('Ctrl Pts',(0.167120287247804,-4.97013543914945,
1.59135816887013));
#29965=CARTESIAN_POINT('Ctrl Pts',(0.183276841782292,-4.9937289476995,1.58950502964782));
#29966=CARTESIAN_POINT('Ctrl Pts',(0.20471752266132,-5.04545944463489,1.58688606295397));
#29967=CARTESIAN_POINT('Ctrl Pts',(0.21,-5.07359906579625,1.58615888233178));
#29968=CARTESIAN_POINT('Ctrl Pts',(0.21,-5.1,1.58615888233178));
#29969=CARTESIAN_POINT('',(-0.172988438920062,-4.98094119100209,0.99));
#29970=CARTESIAN_POINT('Origin',(0.,-5.1,0.99));
#29971=CARTESIAN_POINT('Ctrl Pts',(0.172988438920062,-4.98094119100209,
0.99));
#29972=CARTESIAN_POINT('Ctrl Pts',(0.165594865311318,-4.97019857760471,
0.991291921976381));
#29973=CARTESIAN_POINT('Ctrl Pts',(0.157297138725609,-4.96031229062726,
0.992653949439047));
#29974=CARTESIAN_POINT('Ctrl Pts',(0.129892073845076,-4.93290722574673,
0.996748084390898));
#29975=CARTESIAN_POINT('Ctrl Pts',(0.106330167759284,-4.91675794366705,
0.999695893276376));
#29976=CARTESIAN_POINT('Ctrl Pts',(0.05461290463241,-4.89530220603509,1.00385029472357));
#29977=CARTESIAN_POINT('Ctrl Pts',(0.0264512308298516,-4.89,1.005));
#29978=CARTESIAN_POINT('Ctrl Pts',(-0.0264512308298516,-4.89,1.005));
#29979=CARTESIAN_POINT('Ctrl Pts',(-0.05461290463241,-4.89530220603509,
1.00385029472357));
#29980=CARTESIAN_POINT('Ctrl Pts',(-0.106330167759284,-4.91675794366705,
0.999695893276376));
#29981=CARTESIAN_POINT('Ctrl Pts',(-0.129892073845076,-4.93290722574673,
0.996748084390898));
#29982=CARTESIAN_POINT('Ctrl Pts',(-0.157297138725609,-4.96031229062726,
0.992653949439047));
#29983=CARTESIAN_POINT('Ctrl Pts',(-0.165594865311318,-4.97019857760471,
0.991291921976381));
#29984=CARTESIAN_POINT('Ctrl Pts',(-0.172988438920062,-4.98094119100209,
0.99));
#29985=CARTESIAN_POINT('Origin',(0.,-5.1,0.99));
#29986=CARTESIAN_POINT('',(-0.172988438920062,-5.5,0.99));
#29987=CARTESIAN_POINT('Origin',(0.,-5.5,0.));
#29988=CARTESIAN_POINT('',(-1.005,-4.7,1.23077003314309E-16));
#29989=CARTESIAN_POINT('Origin',(0.,-4.7,0.));
#29990=CARTESIAN_POINT('',(-1.005,-5.5,1.23077003314309E-16));
#29991=CARTESIAN_POINT('',(-1.005,-5.5,1.23077003314309E-16));
#29992=CARTESIAN_POINT('Origin',(0.,-5.5,0.));
#29993=CARTESIAN_POINT('Origin',(0.,-5.5,0.));
#29994=CARTESIAN_POINT('',(-1.6,-4.7,1.95943487863577E-16));
#29995=CARTESIAN_POINT('Origin',(0.,-4.7,0.));
#29996=CARTESIAN_POINT('',(-1.6,-5.5,1.95943487863577E-16));
#29997=CARTESIAN_POINT('',(-1.6,-5.5,1.95943487863577E-16));
#29998=CARTESIAN_POINT('Origin',(0.,-5.5,0.));
#29999=CARTESIAN_POINT('Origin',(0.,-4.7,0.));
#30000=CARTESIAN_POINT('Origin',(0.,-5.5,0.));
#30001=CARTESIAN_POINT('',(0.,0.,0.));
#30002=CARTESIAN_POINT('Origin',(0.,-4.7,0.));
#30003=CARTESIAN_POINT('',(-1.01,-4.2,1.23689326713883E-16));
#30004=CARTESIAN_POINT('Origin',(0.,-4.2,0.));
#30005=CARTESIAN_POINT('',(-1.01,-4.7,1.23689326713883E-16));
#30006=CARTESIAN_POINT('',(-1.01,-4.7,1.23689326713883E-16));
#30007=CARTESIAN_POINT('Origin',(0.,-4.7,0.));
#30008=CARTESIAN_POINT('Origin',(0.,-4.7,0.));
#30009=CARTESIAN_POINT('',(-1.35,-4.2,1.65327317884893E-16));
#30010=CARTESIAN_POINT('Origin',(0.,-4.2,0.));
#30011=CARTESIAN_POINT('',(-1.35,-4.7,1.65327317884893E-16));
#30012=CARTESIAN_POINT('',(-1.35,-4.7,1.65327317884893E-16));
#30013=CARTESIAN_POINT('Origin',(0.,-4.7,0.));
#30014=CARTESIAN_POINT('Origin',(0.,-4.2,0.));
#30015=CARTESIAN_POINT('Origin',(0.,-4.7,0.));
#30016=CARTESIAN_POINT('',(0.,0.,0.));
#30017=CARTESIAN_POINT('Origin',(0.,5.1,0.99));
#30018=CARTESIAN_POINT('',(0.172988438920062,4.98094119100209,0.99));
#30019=CARTESIAN_POINT('',(0.172988438920062,5.21905880899791,0.99));
#30020=CARTESIAN_POINT('',(0.172988438920062,4.7,0.99));
#30021=CARTESIAN_POINT('Origin',(0.,5.1,0.99));
#30022=CARTESIAN_POINT('Origin',(0.,5.1,0.99));
#30023=CARTESIAN_POINT('',(-0.172988438920062,4.98094119100209,0.99));
#30024=CARTESIAN_POINT('Ctrl Pts',(-0.172988438920062,4.98094119100209,
0.99));
#30025=CARTESIAN_POINT('Ctrl Pts',(-0.165594865311318,4.97019857760471,
0.991291921976381));
#30026=CARTESIAN_POINT('Ctrl Pts',(-0.157297138725609,4.96031229062726,
0.992653949439047));
#30027=CARTESIAN_POINT('Ctrl Pts',(-0.129892073845076,4.93290722574673,
0.996748084390898));
#30028=CARTESIAN_POINT('Ctrl Pts',(-0.106330167759284,4.91675794366705,
0.999695893276376));
#30029=CARTESIAN_POINT('Ctrl Pts',(-0.05461290463241,4.89530220603509,1.00385029472357));
#30030=CARTESIAN_POINT('Ctrl Pts',(-0.0264512308298516,4.89,1.005));
#30031=CARTESIAN_POINT('Ctrl Pts',(0.0264512308298516,4.89,1.005));
#30032=CARTESIAN_POINT('Ctrl Pts',(0.0546129046324099,4.89530220603509,
1.00385029472357));
#30033=CARTESIAN_POINT('Ctrl Pts',(0.106330167759284,4.91675794366705,0.999695893276376));
#30034=CARTESIAN_POINT('Ctrl Pts',(0.129892073845076,4.93290722574673,0.996748084390898));
#30035=CARTESIAN_POINT('Ctrl Pts',(0.157297138725609,4.96031229062726,0.992653949439047));
#30036=CARTESIAN_POINT('Ctrl Pts',(0.165594865311318,4.97019857760471,0.991291921976381));
#30037=CARTESIAN_POINT('Ctrl Pts',(0.172988438920062,4.98094119100209,0.99));
#30038=CARTESIAN_POINT('',(-0.21,5.1,0.99));
#30039=CARTESIAN_POINT('Origin',(0.,5.1,0.99));
#30040=CARTESIAN_POINT('',(-0.21,5.1,1.58615888233178));
#30041=CARTESIAN_POINT('',(-0.21,5.1,0.99));
#30042=CARTESIAN_POINT('',(0.21,5.1,1.58615888233178));
#30043=CARTESIAN_POINT('Ctrl Pts',(0.21,5.1,1.58615888233178));
#30044=CARTESIAN_POINT('Ctrl Pts',(0.21,5.07359906579625,1.58615888233178));
#30045=CARTESIAN_POINT('Ctrl Pts',(0.20471752266132,5.04545944463489,1.58688606295397));
#30046=CARTESIAN_POINT('Ctrl Pts',(0.183276841782292,4.9937289476995,1.58950502964782));
#30047=CARTESIAN_POINT('Ctrl Pts',(0.167120287247804,4.97013543914945,1.59135816887013));
#30048=CARTESIAN_POINT('Ctrl Pts',(0.129864750292352,4.932879902194,1.59483075953278));
#30049=CARTESIAN_POINT('Ctrl Pts',(0.106271159541076,4.91672319916876,1.59667690933009));
#30050=CARTESIAN_POINT('Ctrl Pts',(0.0545403836274689,4.8952824096556,1.59927985626981));
#30051=CARTESIAN_POINT('Ctrl Pts',(0.0264006657112964,4.89,1.6));
#30052=CARTESIAN_POINT('Ctrl Pts',(-0.0264006657112964,4.89,1.6));
#30053=CARTESIAN_POINT('Ctrl Pts',(-0.0545403836274688,4.8952824096556,
1.59927985626981));
#30054=CARTESIAN_POINT('Ctrl Pts',(-0.106271159541076,4.91672319916876,
1.59667690933009));
#30055=CARTESIAN_POINT('Ctrl Pts',(-0.129864750292352,4.932879902194,1.59483075953278));
#30056=CARTESIAN_POINT('Ctrl Pts',(-0.167120287247804,4.97013543914945,
1.59135816887013));
#30057=CARTESIAN_POINT('Ctrl Pts',(-0.183276841782292,4.9937289476995,1.58950502964782));
#30058=CARTESIAN_POINT('Ctrl Pts',(-0.20471752266132,5.04545944463489,1.58688606295397));
#30059=CARTESIAN_POINT('Ctrl Pts',(-0.21,5.07359906579625,1.58615888233178));
#30060=CARTESIAN_POINT('Ctrl Pts',(-0.21,5.1,1.58615888233178));
#30061=CARTESIAN_POINT('Ctrl Pts',(-0.21,5.1,1.58615888233178));
#30062=CARTESIAN_POINT('Ctrl Pts',(-0.21,5.12640093420375,1.58615888233178));
#30063=CARTESIAN_POINT('Ctrl Pts',(-0.20471752266132,5.15454055536511,1.58688606295397));
#30064=CARTESIAN_POINT('Ctrl Pts',(-0.183276841782292,5.2062710523005,1.58950502964782));
#30065=CARTESIAN_POINT('Ctrl Pts',(-0.167120287247804,5.22986456085055,
1.59135816887013));
#30066=CARTESIAN_POINT('Ctrl Pts',(-0.129864750292352,5.267120097806,1.59483075953278));
#30067=CARTESIAN_POINT('Ctrl Pts',(-0.106271159541076,5.28327680083123,
1.59667690933009));
#30068=CARTESIAN_POINT('Ctrl Pts',(-0.0545403836274689,5.3047175903444,
1.59927985626981));
#30069=CARTESIAN_POINT('Ctrl Pts',(-0.0264006657112965,5.31,1.6));
#30070=CARTESIAN_POINT('Ctrl Pts',(0.0264006657112964,5.31,1.6));
#30071=CARTESIAN_POINT('Ctrl Pts',(0.0545403836274689,5.3047175903444,1.59927985626981));
#30072=CARTESIAN_POINT('Ctrl Pts',(0.106271159541076,5.28327680083123,1.59667690933009));
#30073=CARTESIAN_POINT('Ctrl Pts',(0.129864750292352,5.267120097806,1.59483075953278));
#30074=CARTESIAN_POINT('Ctrl Pts',(0.167120287247804,5.22986456085055,1.59135816887013));
#30075=CARTESIAN_POINT('Ctrl Pts',(0.183276841782292,5.2062710523005,1.58950502964782));
#30076=CARTESIAN_POINT('Ctrl Pts',(0.20471752266132,5.15454055536511,1.58688606295397));
#30077=CARTESIAN_POINT('Ctrl Pts',(0.21,5.12640093420375,1.58615888233178));
#30078=CARTESIAN_POINT('Ctrl Pts',(0.21,5.1,1.58615888233178));
#30079=CARTESIAN_POINT('',(-0.172988438920062,5.21905880899791,0.99));
#30080=CARTESIAN_POINT('Origin',(0.,5.1,0.99));
#30081=CARTESIAN_POINT('Ctrl Pts',(0.172988438920062,5.21905880899791,0.99));
#30082=CARTESIAN_POINT('Ctrl Pts',(0.165594865311319,5.22980142239529,0.991291921976381));
#30083=CARTESIAN_POINT('Ctrl Pts',(0.157297138725609,5.23968770937274,0.992653949439047));
#30084=CARTESIAN_POINT('Ctrl Pts',(0.129892073845076,5.26709277425327,0.996748084390898));
#30085=CARTESIAN_POINT('Ctrl Pts',(0.106330167759284,5.28324205633295,0.999695893276376));
#30086=CARTESIAN_POINT('Ctrl Pts',(0.05461290463241,5.30469779396491,1.00385029472357));
#30087=CARTESIAN_POINT('Ctrl Pts',(0.0264512308298516,5.31,1.005));
#30088=CARTESIAN_POINT('Ctrl Pts',(-0.0264512308298516,5.31,1.005));
#30089=CARTESIAN_POINT('Ctrl Pts',(-0.0546129046324098,5.30469779396491,
1.00385029472357));
#30090=CARTESIAN_POINT('Ctrl Pts',(-0.106330167759284,5.28324205633295,
0.999695893276376));
#30091=CARTESIAN_POINT('Ctrl Pts',(-0.129892073845076,5.26709277425327,
0.996748084390898));
#30092=CARTESIAN_POINT('Ctrl Pts',(-0.157297138725609,5.23968770937274,
0.992653949439047));
#30093=CARTESIAN_POINT('Ctrl Pts',(-0.165594865311318,5.22980142239529,
0.991291921976381));
#30094=CARTESIAN_POINT('Ctrl Pts',(-0.172988438920062,5.21905880899791,
0.99));
#30095=CARTESIAN_POINT('Origin',(0.,5.1,0.99));
#30096=CARTESIAN_POINT('',(-0.172988438920062,4.7,0.99));
#30097=CARTESIAN_POINT('Origin',(0.,4.7,0.));
#30098=CARTESIAN_POINT('',(-1.005,5.5,1.23077003314309E-16));
#30099=CARTESIAN_POINT('Origin',(0.,5.5,0.));
#30100=CARTESIAN_POINT('',(-1.005,4.7,1.23077003314309E-16));
#30101=CARTESIAN_POINT('',(-1.005,4.7,1.23077003314309E-16));
#30102=CARTESIAN_POINT('Origin',(0.,4.7,0.));
#30103=CARTESIAN_POINT('Origin',(0.,4.7,0.));
#30104=CARTESIAN_POINT('',(-1.6,5.5,1.95943487863577E-16));
#30105=CARTESIAN_POINT('Origin',(0.,5.5,0.));
#30106=CARTESIAN_POINT('',(-1.6,4.7,1.95943487863577E-16));
#30107=CARTESIAN_POINT('',(-1.6,4.7,1.95943487863577E-16));
#30108=CARTESIAN_POINT('Origin',(0.,4.7,0.));
#30109=CARTESIAN_POINT('Origin',(0.,5.5,0.));
#30110=CARTESIAN_POINT('Origin',(0.,4.7,0.));
#30111=CARTESIAN_POINT('',(0.,0.,0.));
#30112=CARTESIAN_POINT('Origin',(0.,4.2,0.));
#30113=CARTESIAN_POINT('',(-1.01,4.7,1.23689326713883E-16));
#30114=CARTESIAN_POINT('Origin',(0.,4.7,0.));
#30115=CARTESIAN_POINT('',(-1.01,4.2,1.23689326713883E-16));
#30116=CARTESIAN_POINT('',(-1.01,4.2,1.23689326713883E-16));
#30117=CARTESIAN_POINT('Origin',(0.,4.2,0.));
#30118=CARTESIAN_POINT('Origin',(0.,4.2,0.));
#30119=CARTESIAN_POINT('',(-1.35,4.7,1.65327317884893E-16));
#30120=CARTESIAN_POINT('Origin',(0.,4.7,0.));
#30121=CARTESIAN_POINT('',(-1.35,4.2,1.65327317884893E-16));
#30122=CARTESIAN_POINT('',(-1.35,4.2,1.65327317884893E-16));
#30123=CARTESIAN_POINT('Origin',(0.,4.2,0.));
#30124=CARTESIAN_POINT('Origin',(0.,4.7,0.));
#30125=CARTESIAN_POINT('Origin',(0.,4.2,0.));
#30126=CARTESIAN_POINT('',(0.,0.,0.));
#30127=CARTESIAN_POINT('Origin',(0.3,0.,0.));
#30128=CARTESIAN_POINT('',(0.3,2.2,-1.28));
#30129=CARTESIAN_POINT('',(0.3,2.2,-0.953939201416946));
#30130=CARTESIAN_POINT('',(0.3,2.2,0.));
#30131=CARTESIAN_POINT('',(0.3,-1.,-1.28));
#30132=CARTESIAN_POINT('',(0.3,0.,-1.28));
#30133=CARTESIAN_POINT('',(0.3,-1.,-0.953939201416946));
#30134=CARTESIAN_POINT('',(0.3,-1.,0.));
#30135=CARTESIAN_POINT('',(0.3,0.,-0.953939201416946));
#30136=CARTESIAN_POINT('Origin',(0.3,0.,-1.28));
#30137=CARTESIAN_POINT('',(-0.3,2.2,-1.28));
#30138=CARTESIAN_POINT('',(0.15,2.2,-1.28));
#30139=CARTESIAN_POINT('',(-0.3,-1.,-1.28));
#30140=CARTESIAN_POINT('',(-0.3,0.,-1.28));
#30141=CARTESIAN_POINT('',(0.15,-1.,-1.28));
#30142=CARTESIAN_POINT('Origin',(-0.3,0.,-1.28));
#30143=CARTESIAN_POINT('',(-0.3,2.2,-0.953939201416946));
#30144=CARTESIAN_POINT('',(-0.3,2.2,-0.64));
#30145=CARTESIAN_POINT('',(-0.3,-1.,-0.953939201416946));
#30146=CARTESIAN_POINT('',(-0.3,0.,-0.953939201416946));
#30147=CARTESIAN_POINT('',(-0.3,-1.,-0.64));
#30148=CARTESIAN_POINT('Origin',(0.,-1.,0.));
#30149=CARTESIAN_POINT('',(3.66661143271685,-1.,0.786422660831985));
#30150=CARTESIAN_POINT('',(3.62400312501245,-1.,0.963899035117249));
#30151=CARTESIAN_POINT('Origin',(0.,-1.,0.));
#30152=CARTESIAN_POINT('',(4.01728681790024,-1.,1.22531898815164));
#30153=CARTESIAN_POINT('Ctrl Pts',(3.62400312501245,-1.,0.963899035117249));
#30154=CARTESIAN_POINT('Ctrl Pts',(3.6240482887845,-1.,0.963880158555582));
#30155=CARTESIAN_POINT('Ctrl Pts',(3.62424461507588,-1.,0.963861297423241));
#30156=CARTESIAN_POINT('Ctrl Pts',(3.62489305727662,-1.,0.963957782642844));
#30157=CARTESIAN_POINT('Ctrl Pts',(3.62652618145335,-1.,0.964373850166458));
#30158=CARTESIAN_POINT('Ctrl Pts',(3.62988252139846,-1.,0.965395153165294));
#30159=CARTESIAN_POINT('Ctrl Pts',(3.63492122081143,-1.,0.967052554541386));
#30160=CARTESIAN_POINT('Ctrl Pts',(3.64113946505766,-1.,0.969195124675866));
#30161=CARTESIAN_POINT('Ctrl Pts',(3.64819756447455,-1.,0.971722122061341));
#30162=CARTESIAN_POINT('Ctrl Pts',(3.65571576735126,-1.,0.974519971354849));
#30163=CARTESIAN_POINT('Ctrl Pts',(3.66333049637475,-1.,0.977478312751618));
#30164=CARTESIAN_POINT('Ctrl Pts',(3.67074983340361,-1.,0.980505922458267));
#30165=CARTESIAN_POINT('Ctrl Pts',(3.67782408841715,-1.,0.98355079147042));
#30166=CARTESIAN_POINT('Ctrl Pts',(3.68455317926068,-1.,0.986602639863838));
#30167=CARTESIAN_POINT('Ctrl Pts',(3.69102682138846,-1.,0.989676715398559));
#30168=CARTESIAN_POINT('Ctrl Pts',(3.69738123415662,-1.,0.992802218332011));
#30169=CARTESIAN_POINT('Ctrl Pts',(3.70375282282138,-1.,0.996009819772518));
#30170=CARTESIAN_POINT('Ctrl Pts',(3.71022439713938,-1.,0.999317260756531));
#30171=CARTESIAN_POINT('Ctrl Pts',(3.71680667125118,-1.,1.00272423396822));
#30172=CARTESIAN_POINT('Ctrl Pts',(3.72346803750595,-1.,1.0062200073571));
#30173=CARTESIAN_POINT('Ctrl Pts',(3.73015276704426,-1.,1.00978798539496));
#30174=CARTESIAN_POINT('Ctrl Pts',(3.73680245055734,-1.,1.01341114319903));
#30175=CARTESIAN_POINT('Ctrl Pts',(3.74337942504959,-1.,1.01707794311079));
#30176=CARTESIAN_POINT('Ctrl Pts',(3.74987777155834,-1.,1.02078510487428));
#30177=CARTESIAN_POINT('Ctrl Pts',(3.75631037456194,-1.,1.0245342944466));
#30178=CARTESIAN_POINT('Ctrl Pts',(3.76270122291232,-1.,1.02833014458181));
#30179=CARTESIAN_POINT('Ctrl Pts',(3.76907609832522,-1.,1.0321778660492));
#30180=CARTESIAN_POINT('Ctrl Pts',(3.77545283140445,-1.,1.03608074678013));
#30181=CARTESIAN_POINT('Ctrl Pts',(3.78183535008192,-1.,1.04003862055804));
#30182=CARTESIAN_POINT('Ctrl Pts',(3.78821910787195,-1.,1.04404924374426));
#30183=CARTESIAN_POINT('Ctrl Pts',(3.79459440308793,-1.,1.04810913267641));
#30184=CARTESIAN_POINT('Ctrl Pts',(3.80095039790678,-1.,1.05221457990015));
#30185=CARTESIAN_POINT('Ctrl Pts',(3.80727913637784,-1.,1.05636266918643));
#30186=CARTESIAN_POINT('Ctrl Pts',(3.81357866117485,-1.,1.06055206187298));
#30187=CARTESIAN_POINT('Ctrl Pts',(3.81985083953012,-1.,1.06478244038931));
#30188=CARTESIAN_POINT('Ctrl Pts',(3.82609989967278,-1.,1.0690541318036));
#30189=CARTESIAN_POINT('Ctrl Pts',(3.83233071195145,-1.,1.0733676663346));
#30190=CARTESIAN_POINT('Ctrl Pts',(3.83854714117486,-1.,1.07772335353856));
#30191=CARTESIAN_POINT('Ctrl Pts',(3.84475048030615,-1.,1.08212087917986));
#30192=CARTESIAN_POINT('Ctrl Pts',(3.8509402522269,-1.,1.08655950846377));
#30193=CARTESIAN_POINT('Ctrl Pts',(3.85711487933911,-1.,1.09103825516288));
#30194=CARTESIAN_POINT('Ctrl Pts',(3.86327241021242,-1.,1.09555606505012));
#30195=CARTESIAN_POINT('Ctrl Pts',(3.86941120134872,-1.,1.10011198761203));
#30196=CARTESIAN_POINT('Ctrl Pts',(3.87553067187566,-1.,1.10470536603303));
#30197=CARTESIAN_POINT('Ctrl Pts',(3.88163105531791,-1.,1.10933577224029));
#30198=CARTESIAN_POINT('Ctrl Pts',(3.88771308285229,-1.,1.11400292434447));
#30199=CARTESIAN_POINT('Ctrl Pts',(3.89377768340362,-1.,1.11870660794609));
#30200=CARTESIAN_POINT('Ctrl Pts',(3.89982569749978,-1.,1.12344660099029));
#30201=CARTESIAN_POINT('Ctrl Pts',(3.90585753318622,-1.,1.12822258281518));
#30202=CARTESIAN_POINT('Ctrl Pts',(3.91187321145495,-1.,1.13303414693849));
#30203=CARTESIAN_POINT('Ctrl Pts',(3.91787251936688,-1.,1.13788084225511));
#30204=CARTESIAN_POINT('Ctrl Pts',(3.92385513133937,-1.,1.14276220561575));
#30205=CARTESIAN_POINT('Ctrl Pts',(3.92982073294334,-1.,1.14767779451147));
#30206=CARTESIAN_POINT('Ctrl Pts',(3.9357691705651,-1.,1.15262722716391));
#30207=CARTESIAN_POINT('Ctrl Pts',(3.94170046685542,-1.,1.15761018341061));
#30208=CARTESIAN_POINT('Ctrl Pts',(3.9476147478092,-1.,1.16262637999261));
#30209=CARTESIAN_POINT('Ctrl Pts',(3.95351219510062,-1.,1.16767555244495));
#30210=CARTESIAN_POINT('Ctrl Pts',(3.95939299213164,-1.,1.17275743590327));
#30211=CARTESIAN_POINT('Ctrl Pts',(3.96525726357682,-1.,1.17787174135446));
#30212=CARTESIAN_POINT('Ctrl Pts',(3.9711050516465,-1.,1.18301815039596));
#30213=CARTESIAN_POINT('Ctrl Pts',(3.97693634766926,-1.,1.18819633715285));
#30214=CARTESIAN_POINT('Ctrl Pts',(3.98275111052015,-1.,1.19340598349307));
#30215=CARTESIAN_POINT('Ctrl Pts',(3.98854928957287,-1.,1.19864679609596));
#30216=CARTESIAN_POINT('Ctrl Pts',(3.99433084800649,-1.,1.2039185237544));
#30217=CARTESIAN_POINT('Ctrl Pts',(4.00009577952534,-1.,1.20922097030107));
#30218=CARTESIAN_POINT('Ctrl Pts',(4.00584409524937,-1.,1.21455398918813));
#30219=CARTESIAN_POINT('Ctrl Pts',(4.01042947142681,-1.,1.21884478244983));
#30220=CARTESIAN_POINT('Ctrl Pts',(4.01386104434674,-1.,1.22207656456199));
#30221=CARTESIAN_POINT('Ctrl Pts',(4.0161454457032,-1.,1.22423716681447));
#30222=CARTESIAN_POINT('Ctrl Pts',(4.01728681790024,-1.,1.22531898815164));
#30223=CARTESIAN_POINT('',(3.97027773754922,-1.,1.36999806084573));
#30224=CARTESIAN_POINT('',(4.01728681790024,-1.,1.22531898815164));
#30225=CARTESIAN_POINT('',(3.4984457533445,-1.,1.35032489087101));
#30226=CARTESIAN_POINT('Ctrl Pts',(3.97027773754922,-1.,1.36999806084573));
#30227=CARTESIAN_POINT('Ctrl Pts',(3.9687184694131,-1.,1.37020239094614));
#30228=CARTESIAN_POINT('Ctrl Pts',(3.96560037974645,-1.,1.37060761745635));
#30229=CARTESIAN_POINT('Ctrl Pts',(3.96092458506535,-1.,1.3712051561502));
#30230=CARTESIAN_POINT('Ctrl Pts',(3.95469287280914,-1.,1.37198126432386));
#30231=CARTESIAN_POINT('Ctrl Pts',(3.94690771785133,-1.,1.37291699202807));
#30232=CARTESIAN_POINT('Ctrl Pts',(3.93912709040818,-1.,1.37381821967165));
#30233=CARTESIAN_POINT('Ctrl Pts',(3.93135106761844,-1.,1.37468482215751));
#30234=CARTESIAN_POINT('Ctrl Pts',(3.92357976987672,-1.,1.37551664448242));
#30235=CARTESIAN_POINT('Ctrl Pts',(3.91581337462644,-1.,1.37631350505797));
#30236=CARTESIAN_POINT('Ctrl Pts',(3.90805209523486,-1.,1.3770751963402));
#30237=CARTESIAN_POINT('Ctrl Pts',(3.90029615196727,-1.,1.37780148512792));
#30238=CARTESIAN_POINT('Ctrl Pts',(3.89254574338496,-1.,1.3784921128802));
#30239=CARTESIAN_POINT('Ctrl Pts',(3.88480102249277,-1.,1.37914679719383));
#30240=CARTESIAN_POINT('Ctrl Pts',(3.87706205830532,-1.,1.37976523097073));
#30241=CARTESIAN_POINT('Ctrl Pts',(3.86932885813068,-1.,1.38034709213014));
#30242=CARTESIAN_POINT('Ctrl Pts',(3.86160143043959,-1.,1.3808920599299));
#30243=CARTESIAN_POINT('Ctrl Pts',(3.85387983979481,-1.,1.3813998311505));
#30244=CARTESIAN_POINT('Ctrl Pts',(3.84616425605764,-1.,1.38187013346109));
#30245=CARTESIAN_POINT('Ctrl Pts',(3.83845502790746,-1.,1.38230274828822));
#30246=CARTESIAN_POINT('Ctrl Pts',(3.8307526698229,-1.,1.38269750245138));
#30247=CARTESIAN_POINT('Ctrl Pts',(3.82305771743829,-1.,1.38305421262763));
#30248=CARTESIAN_POINT('Ctrl Pts',(3.81537060817811,-1.,1.38337263902782));
#30249=CARTESIAN_POINT('Ctrl Pts',(3.80769156398411,-1.,1.3836524404622));
#30250=CARTESIAN_POINT('Ctrl Pts',(3.80002044322111,-1.,1.38389311766682));
#30251=CARTESIAN_POINT('Ctrl Pts',(3.79235669640841,-1.,1.38409399694566));
#30252=CARTESIAN_POINT('Ctrl Pts',(3.78469969805082,-1.,1.38425435883756));
#30253=CARTESIAN_POINT('Ctrl Pts',(3.77704902230418,-1.,1.38437354551428));
#30254=CARTESIAN_POINT('Ctrl Pts',(3.76940473185779,-1.,1.38445107339518));
#30255=CARTESIAN_POINT('Ctrl Pts',(3.76176768271367,-1.,1.3844867525335));
#30256=CARTESIAN_POINT('Ctrl Pts',(3.7541397631875,-1.,1.38448077997163));
#30257=CARTESIAN_POINT('Ctrl Pts',(3.74652317167876,-1.,1.38443344984394));
#30258=CARTESIAN_POINT('Ctrl Pts',(3.73891976418104,-1.,1.38434489156458));
#30259=CARTESIAN_POINT('Ctrl Pts',(3.73133035859282,-1.,1.38421479111531));
#30260=CARTESIAN_POINT('Ctrl Pts',(3.72375409358803,-1.,1.3840421342895));
#30261=CARTESIAN_POINT('Ctrl Pts',(3.7161876605181,-1.,1.38382489984586));
#30262=CARTESIAN_POINT('Ctrl Pts',(3.70862680753347,-1.,1.38356065402124));
#30263=CARTESIAN_POINT('Ctrl Pts',(3.701067921679,-1.,1.38324717612865));
#30264=CARTESIAN_POINT('Ctrl Pts',(3.69350967899526,-1.,1.38288311171651));
#30265=CARTESIAN_POINT('Ctrl Pts',(3.68595444983837,-1.,1.38246852827182));
#30266=CARTESIAN_POINT('Ctrl Pts',(3.67841038482414,-1.,1.3820057429062));
#30267=CARTESIAN_POINT('Ctrl Pts',(3.67088843112262,-1.,1.38149812653868));
#30268=CARTESIAN_POINT('Ctrl Pts',(3.66339848520857,-1.,1.38094856333552));
#30269=CARTESIAN_POINT('Ctrl Pts',(3.6559455440439,-1.,1.38035791051213));
#30270=CARTESIAN_POINT('Ctrl Pts',(3.64852652756456,-1.,1.37972372481603));
#30271=CARTESIAN_POINT('Ctrl Pts',(3.64112507791141,-1.,1.37903818567359));
#30272=CARTESIAN_POINT('Ctrl Pts',(3.63371727442486,-1.,1.37829035457339));
#30273=CARTESIAN_POINT('Ctrl Pts',(3.62628098665145,-1.,1.37746987919881));
#30274=CARTESIAN_POINT('Ctrl Pts',(3.6188048116042,-1.,1.37657053403107));
#30275=CARTESIAN_POINT('Ctrl Pts',(3.61129546591064,-1.,1.37559314436634));
#30276=CARTESIAN_POINT('Ctrl Pts',(3.60379020123988,-1.,1.37455051379623));
#30277=CARTESIAN_POINT('Ctrl Pts',(3.59634627869048,-1.,1.37346320103157));
#30278=CARTESIAN_POINT('Ctrl Pts',(3.58901853846365,-1.,1.37235053660976));
#30279=CARTESIAN_POINT('Ctrl Pts',(3.58183885982715,-1.,1.37122241663062));
#30280=CARTESIAN_POINT('Ctrl Pts',(3.57479875549486,-1.,1.37007229485659));
#30281=CARTESIAN_POINT('Ctrl Pts',(3.5678208030466,-1.,1.36886584973389));
#30282=CARTESIAN_POINT('Ctrl Pts',(3.56077662028649,-1.,1.36754771771233));
#30283=CARTESIAN_POINT('Ctrl Pts',(3.55353883995949,-1.,1.3660614545677));
#30284=CARTESIAN_POINT('Ctrl Pts',(3.54602591832973,-1.,1.36436666257598));
#30285=CARTESIAN_POINT('Ctrl Pts',(3.53824396424961,-1.,1.36245507339307));
#30286=CARTESIAN_POINT('Ctrl Pts',(3.530344649616,-1.,1.36037259643734));
#30287=CARTESIAN_POINT('Ctrl Pts',(3.52261776116748,-1.,1.35821701528836));
#30288=CARTESIAN_POINT('Ctrl Pts',(3.51542230699556,-1.,1.35611275237152));
#30289=CARTESIAN_POINT('Ctrl Pts',(3.50913227059999,-1.,1.35419113575956));
#30290=CARTESIAN_POINT('Ctrl Pts',(3.50408168106261,-1.,1.35257032843486));
#30291=CARTESIAN_POINT('Ctrl Pts',(3.5007660381649,-1.,1.35142377279517));
#30292=CARTESIAN_POINT('Ctrl Pts',(3.49920025459723,-1.,1.35080045218587));
#30293=CARTESIAN_POINT('Ctrl Pts',(3.49861894124827,-1.,1.35049736560527));
#30294=CARTESIAN_POINT('Ctrl Pts',(3.49847119623846,-1.,1.35036670892966));
#30295=CARTESIAN_POINT('Ctrl Pts',(3.4984457533445,-1.,1.35032489087101));
#30296=CARTESIAN_POINT('',(3.42859860294378,-1.,1.51895082866166));
#30297=CARTESIAN_POINT('Origin',(0.,-1.,0.));
#30298=CARTESIAN_POINT('',(3.77614523045147,-1.,1.83867539237861));
#30299=CARTESIAN_POINT('Ctrl Pts',(3.42859860294378,-1.,1.51895082866166));
#30300=CARTESIAN_POINT('Ctrl Pts',(3.42864616361967,-1.,1.51893924967231));
#30301=CARTESIAN_POINT('Ctrl Pts',(3.42884302333978,-1.,1.51895133295017));
#30302=CARTESIAN_POINT('Ctrl Pts',(3.42946838852728,-1.,1.51914806898539));
#30303=CARTESIAN_POINT('Ctrl Pts',(3.4310163189349,-1.,1.5198144909343));
#30304=CARTESIAN_POINT('Ctrl Pts',(3.43417156977749,-1.,1.52134826724227));
#30305=CARTESIAN_POINT('Ctrl Pts',(3.43888895974182,-1.,1.52377348950429));
#30306=CARTESIAN_POINT('Ctrl Pts',(3.44469547527,-1.,1.52686242875717));
#30307=CARTESIAN_POINT('Ctrl Pts',(3.45127136828667,-1.,1.530462444618));
#30308=CARTESIAN_POINT('Ctrl Pts',(3.45825932955273,-1.,1.53440195378902));
#30309=CARTESIAN_POINT('Ctrl Pts',(3.46531752207222,-1.,1.53851507915533));
#30310=CARTESIAN_POINT('Ctrl Pts',(3.47217189224576,-1.,1.54266605398152));
#30311=CARTESIAN_POINT('Ctrl Pts',(3.47868272898599,-1.,1.54678009290207));
#30312=CARTESIAN_POINT('Ctrl Pts',(3.48485155928414,-1.,1.55084702970382));
#30313=CARTESIAN_POINT('Ctrl Pts',(3.49076460877317,-1.,1.5548959590107));
#30314=CARTESIAN_POINT('Ctrl Pts',(3.49655185179623,-1.,1.55897703097859));
#30315=CARTESIAN_POINT('Ctrl Pts',(3.50234321621607,-1.,1.56314187758689));
#30316=CARTESIAN_POINT('Ctrl Pts',(3.50821771695427,-1.,1.56742097575041));
#30317=CARTESIAN_POINT('Ctrl Pts',(3.51418598431733,-1.,1.57181569799774));
#30318=CARTESIAN_POINT('Ctrl Pts',(3.52021847865961,-1.,1.5763104998818));
#30319=CARTESIAN_POINT('Ctrl Pts',(3.52626275334899,-1.,1.58088027227856));
#30320=CARTESIAN_POINT('Ctrl Pts',(3.53226378147068,-1.,1.58549906268083));
#30321=CARTESIAN_POINT('Ctrl Pts',(3.53818616861045,-1.,1.59014958368725));
#30322=CARTESIAN_POINT('Ctrl Pts',(3.544024581823,-1.,1.5948276694975));
#30323=CARTESIAN_POINT('Ctrl Pts',(3.54979148634426,-1.,1.59953698113444));
#30324=CARTESIAN_POINT('Ctrl Pts',(3.55550985096117,-1.,1.60428584699848));
#30325=CARTESIAN_POINT('Ctrl Pts',(3.56120432482986,-1.,1.60908344685459));
#30326=CARTESIAN_POINT('Ctrl Pts',(3.56689200468404,-1.,1.61393581747522));
#30327=CARTESIAN_POINT('Ctrl Pts',(3.57257679609826,-1.,1.61884340915412));
#30328=CARTESIAN_POINT('Ctrl Pts',(3.57825455954405,-1.,1.62380329464851));
#30329=CARTESIAN_POINT('Ctrl Pts',(3.5839162577435,-1.,1.62881051550748));
#30330=CARTESIAN_POINT('Ctrl Pts',(3.58955176627876,-1.,1.63385971451259));
#30331=CARTESIAN_POINT('Ctrl Pts',(3.59515368334887,-1.,1.63894676675349));
#30332=CARTESIAN_POINT('Ctrl Pts',(3.6007202851384,-1.,1.6440700438558));
#30333=CARTESIAN_POINT('Ctrl Pts',(3.60625346556992,-1.,1.64922952425833));
#30334=CARTESIAN_POINT('Ctrl Pts',(3.61175734965129,-1.,1.65442619244327));
#30335=CARTESIAN_POINT('Ctrl Pts',(3.61723666482457,-1.,1.65966133399186));
#30336=CARTESIAN_POINT('Ctrl Pts',(3.62269517989104,-1.,1.66493585923853));
#30337=CARTESIAN_POINT('Ctrl Pts',(3.62813422105257,-1.,1.67024966008037));
#30338=CARTESIAN_POINT('Ctrl Pts',(3.63355343201211,-1.,1.67560193613145));
#30339=CARTESIAN_POINT('Ctrl Pts',(3.63895140887443,-1.,1.68099146651577));
#30340=CARTESIAN_POINT('Ctrl Pts',(3.64432638915199,-1.,1.68641690471455));
#30341=CARTESIAN_POINT('Ctrl Pts',(3.64967689827393,-1.,1.691877054817));
#30342=CARTESIAN_POINT('Ctrl Pts',(3.65500246526798,-1.,1.69737117722559));
#30343=CARTESIAN_POINT('Ctrl Pts',(3.6603033877491,-1.,1.70289888566904));
#30344=CARTESIAN_POINT('Ctrl Pts',(3.6655804319893,-1.,1.70846001610983));
#30345=CARTESIAN_POINT('Ctrl Pts',(3.67083454901629,-1.,1.71405450210392));
#30346=CARTESIAN_POINT('Ctrl Pts',(3.67606660374665,-1.,1.71968225581787));
#30347=CARTESIAN_POINT('Ctrl Pts',(3.68127704936472,-1.,1.72534302437003));
#30348=CARTESIAN_POINT('Ctrl Pts',(3.68646597019188,-1.,1.73103640956647));
#30349=CARTESIAN_POINT('Ctrl Pts',(3.69163322647906,-1.,1.73676193254493));
#30350=CARTESIAN_POINT('Ctrl Pts',(3.6967785691046,-1.,1.74251908492589));
#30351=CARTESIAN_POINT('Ctrl Pts',(3.70190175673422,-1.,1.74830738046092));
#30352=CARTESIAN_POINT('Ctrl Pts',(3.70700269736876,-1.,1.75412641804148));
#30353=CARTESIAN_POINT('Ctrl Pts',(3.71208146346454,-1.,1.75997588499021));
#30354=CARTESIAN_POINT('Ctrl Pts',(3.71713822377675,-1.,1.76585552124549));
#30355=CARTESIAN_POINT('Ctrl Pts',(3.72217319911429,-1.,1.77176509401846));
#30356=CARTESIAN_POINT('Ctrl Pts',(3.72718661205504,-1.,1.77770437039606));
#30357=CARTESIAN_POINT('Ctrl Pts',(3.73217863095022,-1.,1.78367308442682));
#30358=CARTESIAN_POINT('Ctrl Pts',(3.73714934729962,-1.,1.78967092823139));
#30359=CARTESIAN_POINT('Ctrl Pts',(3.74209880351667,-1.,1.79569757859041));
#30360=CARTESIAN_POINT('Ctrl Pts',(3.74702700874954,-1.,1.80175271485519));
#30361=CARTESIAN_POINT('Ctrl Pts',(3.75193395888069,-1.,1.80783603939662));
#30362=CARTESIAN_POINT('Ctrl Pts',(3.75681965683995,-1.,1.81394729834032));
#30363=CARTESIAN_POINT('Ctrl Pts',(3.76168412709652,-1.,1.82008629694924));
#30364=CARTESIAN_POINT('Ctrl Pts',(3.76652740355856,-1.,1.82625289221933));
#30365=CARTESIAN_POINT('Ctrl Pts',(3.77038509819777,-1.,1.83120816956515));
#30366=CARTESIAN_POINT('Ctrl Pts',(3.77326886065484,-1.,1.83493697935064));
#30367=CARTESIAN_POINT('Ctrl Pts',(3.77518714458232,-1.,1.83742834010821));
#30368=CARTESIAN_POINT('Ctrl Pts',(3.77614523045147,-1.,1.83867539237861));
#30369=CARTESIAN_POINT('',(3.70708211654725,-1.,1.97421938526992));
#30370=CARTESIAN_POINT('',(3.77614523045147,-1.,1.83867539237861));
#30371=CARTESIAN_POINT('',(3.24413672884902,-1.,1.88097764062542));
#30372=CARTESIAN_POINT('Ctrl Pts',(3.70708211654725,-1.,1.97421938526992));
#30373=CARTESIAN_POINT('Ctrl Pts',(3.7055100813194,-1.,1.974177276451));
#30374=CARTESIAN_POINT('Ctrl Pts',(3.70236698911837,-1.,1.97408973726149));
#30375=CARTESIAN_POINT('Ctrl Pts',(3.69765528558292,-1.,1.97394846382289));
#30376=CARTESIAN_POINT('Ctrl Pts',(3.69137888597855,-1.,1.97374016224397));
#30377=CARTESIAN_POINT('Ctrl Pts',(3.68354319913416,-1.,1.97344650303631));
#30378=CARTESIAN_POINT('Ctrl Pts',(3.67571738106175,-1.,1.97311947678035));
#30379=CARTESIAN_POINT('Ctrl Pts',(3.66790152751984,-1.,1.9727589719863));
#30380=CARTESIAN_POINT('Ctrl Pts',(3.66009578166865,-1.,1.97236485439317));
#30381=CARTESIAN_POINT('Ctrl Pts',(3.65230034717364,-1.,1.97193697240645));
#30382=CARTESIAN_POINT('Ctrl Pts',(3.64451546724221,-1.,1.97147515441539));
#30383=CARTESIAN_POINT('Ctrl Pts',(3.63674139590853,-1.,1.97097920454698));
#30384=CARTESIAN_POINT('Ctrl Pts',(3.62897836973397,-1.,1.97044889850518));
#30385=CARTESIAN_POINT('Ctrl Pts',(3.62122658401722,-1.,1.96988398129888));
#30386=CARTESIAN_POINT('Ctrl Pts',(3.61348615496393,-1.,1.96928416040712));
#30387=CARTESIAN_POINT('Ctrl Pts',(3.60575714017676,-1.,1.96864911885775));
#30388=CARTESIAN_POINT('Ctrl Pts',(3.59803959819725,-1.,1.96797854118257));
#30389=CARTESIAN_POINT('Ctrl Pts',(3.5903336402273,-1.,1.96727213799507));
#30390=CARTESIAN_POINT('Ctrl Pts',(3.58263947663884,-1.,1.9665296668894));
#30391=CARTESIAN_POINT('Ctrl Pts',(3.57495748601088,-1.,1.96575096652857));
#30392=CARTESIAN_POINT('Ctrl Pts',(3.56728820357933,-1.,1.96493594634643));
#30393=CARTESIAN_POINT('Ctrl Pts',(3.55963218706201,-1.,1.96408450906868));
#30394=CARTESIAN_POINT('Ctrl Pts',(3.55198990600929,-1.,1.96319648628667));
#30395=CARTESIAN_POINT('Ctrl Pts',(3.54436163300425,-1.,1.96227157573058));
#30396=CARTESIAN_POINT('Ctrl Pts',(3.53674730625759,-1.,1.96130926212661));
#30397=CARTESIAN_POINT('Ctrl Pts',(3.52914648844289,-1.,1.96030879411534));
#30398=CARTESIAN_POINT('Ctrl Pts',(3.52155867431438,-1.,1.95926936324436));
#30399=CARTESIAN_POINT('Ctrl Pts',(3.51398354617772,-1.,1.95819025316768));
#30400=CARTESIAN_POINT('Ctrl Pts',(3.50642124159913,-1.,1.95707099606514));
#30401=CARTESIAN_POINT('Ctrl Pts',(3.49887263575602,-1.,1.9559115382367));
#30402=CARTESIAN_POINT('Ctrl Pts',(3.49133956289154,-1.,1.95471236969653));
#30403=CARTESIAN_POINT('Ctrl Pts',(3.48382414832648,-1.,1.95347412486316));
#30404=CARTESIAN_POINT('Ctrl Pts',(3.47632820495926,-1.,1.95219722189878));
#30405=CARTESIAN_POINT('Ctrl Pts',(3.4688525897419,-1.,1.95088147859876));
#30406=CARTESIAN_POINT('Ctrl Pts',(3.46139661060959,-1.,1.94952575850196));
#30407=CARTESIAN_POINT('Ctrl Pts',(3.45395731584051,-1.,1.94812754766524));
#30408=CARTESIAN_POINT('Ctrl Pts',(3.44653088665685,-1.,1.94668377715332));
#30409=CARTESIAN_POINT('Ctrl Pts',(3.43911410197693,-1.,1.94519168842883));
#30410=CARTESIAN_POINT('Ctrl Pts',(3.43170586602436,-1.,1.94364973660285));
#30411=CARTESIAN_POINT('Ctrl Pts',(3.42430850941497,-1.,1.94205835913692));
#30412=CARTESIAN_POINT('Ctrl Pts',(3.41692971994082,-1.,1.94042111965237));
#30413=CARTESIAN_POINT('Ctrl Pts',(3.40957978266622,-1.,1.93874306008132));
#30414=CARTESIAN_POINT('Ctrl Pts',(3.40226802104093,-1.,1.93702857723089));
#30415=CARTESIAN_POINT('Ctrl Pts',(3.39499923640789,-1.,1.93527929945982));
#30416=CARTESIAN_POINT('Ctrl Pts',(3.38777076883267,-1.,1.93349233176794));
#30417=CARTESIAN_POINT('Ctrl Pts',(3.38056768525577,-1.,1.93165739093292));
#30418=CARTESIAN_POINT('Ctrl Pts',(3.37336807068078,-1.,1.92975993109897));
#30419=CARTESIAN_POINT('Ctrl Pts',(3.36615168657597,-1.,1.92778626543803));
#30420=CARTESIAN_POINT('Ctrl Pts',(3.35890824422976,-1.,1.92572846125763));
#30421=CARTESIAN_POINT('Ctrl Pts',(3.35164424847206,-1.,1.92358838440518));
#30422=CARTESIAN_POINT('Ctrl Pts',(3.34439448941915,-1.,1.92138450828378));
#30423=CARTESIAN_POINT('Ctrl Pts',(3.33721230709948,-1.,1.91914609610173));
#30424=CARTESIAN_POINT('Ctrl Pts',(3.33014884257812,-1.,1.91690081930297));
#30425=CARTESIAN_POINT('Ctrl Pts',(3.32323403454507,-1.,1.91466343916612));
#30426=CARTESIAN_POINT('Ctrl Pts',(3.31646052426395,-1.,1.91242616234459));
#30427=CARTESIAN_POINT('Ctrl Pts',(3.30975721158694,-1.,1.91014297830502));
#30428=CARTESIAN_POINT('Ctrl Pts',(3.30300595568341,-1.,1.90773912171424));
#30429=CARTESIAN_POINT('Ctrl Pts',(3.29608978722258,-1.,1.9051389186417));
#30430=CARTESIAN_POINT('Ctrl Pts',(3.28893448600364,-1.,1.9022897124757));
#30431=CARTESIAN_POINT('Ctrl Pts',(3.28154737912287,-1.,1.89918429230425));
#30432=CARTESIAN_POINT('Ctrl Pts',(3.27407108932908,-1.,1.89589172903662));
#30433=CARTESIAN_POINT('Ctrl Pts',(3.2667765388833,-1.,1.89255393500769));
#30434=CARTESIAN_POINT('Ctrl Pts',(3.2599988519361,-1.,1.88934996203508));
#30435=CARTESIAN_POINT('Ctrl Pts',(3.25408686339298,-1.,1.88646802523372));
#30436=CARTESIAN_POINT('Ctrl Pts',(3.24935200512055,-1.,1.88407708646435));
#30437=CARTESIAN_POINT('Ctrl Pts',(3.24625654410705,-1.,1.88242596600422));
#30438=CARTESIAN_POINT('Ctrl Pts',(3.24480754675942,-1.,1.88156537699118));
#30439=CARTESIAN_POINT('Ctrl Pts',(3.24428080352952,-1.,1.88117508446657));
#30440=CARTESIAN_POINT('Ctrl Pts',(3.2441553167131,-1.,1.88102292397987));
#30441=CARTESIAN_POINT('Ctrl Pts',(3.24413672884902,-1.,1.88097764062542));
#30442=CARTESIAN_POINT('',(3.14877060440425,-1.,2.03660101169564));
#30443=CARTESIAN_POINT('Origin',(0.,-1.,0.));
#30444=CARTESIAN_POINT('',(3.44202241512147,-1.,2.40675750623143));
#30445=CARTESIAN_POINT('Ctrl Pts',(3.14877060440425,-1.,2.03660101169564));
#30446=CARTESIAN_POINT('Ctrl Pts',(3.1488193908823,-1.,2.03659701539175));
#30447=CARTESIAN_POINT('Ctrl Pts',(3.14901193669147,-1.,2.03663974554941));
#30448=CARTESIAN_POINT('Ctrl Pts',(3.14959882629936,-1.,2.03693188810614));
#30449=CARTESIAN_POINT('Ctrl Pts',(3.15102344775396,-1.,2.03783225496023));
#30450=CARTESIAN_POINT('Ctrl Pts',(3.1538999167466,-1.,2.03984073791432));
#30451=CARTESIAN_POINT('Ctrl Pts',(3.15817983946525,-1.,2.04297406404132));
#30452=CARTESIAN_POINT('Ctrl Pts',(3.16343165059235,-1.,2.0469333124766));
#30453=CARTESIAN_POINT('Ctrl Pts',(3.16936341689859,-1.,2.05151770247452));
#30454=CARTESIAN_POINT('Ctrl Pts',(3.17564906975592,-1.,2.05650186773279));
#30455=CARTESIAN_POINT('Ctrl Pts',(3.18197692964677,-1.,2.06166849827143));
#30456=CARTESIAN_POINT('Ctrl Pts',(3.18809755562297,-1.,2.06684062744065));
#30457=CARTESIAN_POINT('Ctrl Pts',(3.19388465568113,-1.,2.07192253497765));
#30458=CARTESIAN_POINT('Ctrl Pts',(3.19934132835879,-1.,2.0769044187063));
#30459=CARTESIAN_POINT('Ctrl Pts',(3.20454818630635,-1.,2.08182850370816));
#30460=CARTESIAN_POINT('Ctrl Pts',(3.20962575845433,-1.,2.08676465517435));
#30461=CARTESIAN_POINT('Ctrl Pts',(3.2146942960168,-1.,2.0917841946046));
#30462=CARTESIAN_POINT('Ctrl Pts',(3.21982707347067,-1.,2.09692958434933));
#30463=CARTESIAN_POINT('Ctrl Pts',(3.22503437553496,-1.,2.10220384298534));
#30464=CARTESIAN_POINT('Ctrl Pts',(3.23028945793334,-1.,2.1075869964248));
#30465=CARTESIAN_POINT('Ctrl Pts',(3.23554444767115,-1.,2.11304604021784));
#30466=CARTESIAN_POINT('Ctrl Pts',(3.24074905517282,-1.,2.11854673326972));
#30467=CARTESIAN_POINT('Ctrl Pts',(3.24587102613347,-1.,2.12406646410943));
#30468=CARTESIAN_POINT('Ctrl Pts',(3.25090574493994,-1.,2.1296002839681));
#30469=CARTESIAN_POINT('Ctrl Pts',(3.25586495065027,-1.,2.13515375878786));
#30470=CARTESIAN_POINT('Ctrl Pts',(3.26077002641868,-1.,2.14073870754258));
#30471=CARTESIAN_POINT('Ctrl Pts',(3.26564388189764,-1.,2.14636805295663));
#30472=CARTESIAN_POINT('Ctrl Pts',(3.27050245897244,-1.,2.15205043199818));
#30473=CARTESIAN_POINT('Ctrl Pts',(3.27534954469206,-1.,2.15778690038359));
#30474=CARTESIAN_POINT('Ctrl Pts',(3.28018150841414,-1.,2.16357391934434));
#30475=CARTESIAN_POINT('Ctrl Pts',(3.2849901997973,-1.,2.16940517773459));
#30476=CARTESIAN_POINT('Ctrl Pts',(3.28976645712566,-1.,2.17527380048422));
#30477=CARTESIAN_POINT('Ctrl Pts',(3.29450361500484,-1.,2.18117455557062));
#30478=CARTESIAN_POINT('Ctrl Pts',(3.29920022557635,-1.,2.18710556500325));
#30479=CARTESIAN_POINT('Ctrl Pts',(3.30385816281831,-1.,2.19306710376112));
#30480=CARTESIAN_POINT('Ctrl Pts',(3.30848134694596,-1.,2.19906078949925));
#30481=CARTESIAN_POINT('Ctrl Pts',(3.3130742460895,-1.,2.20508863150608));
#30482=CARTESIAN_POINT('Ctrl Pts',(3.31764044024231,-1.,2.21115211847872));
#30483=CARTESIAN_POINT('Ctrl Pts',(3.32218125618955,-1.,2.21725135110889));
#30484=CARTESIAN_POINT('Ctrl Pts',(3.32669646722871,-1.,2.22338548312759));
#30485=CARTESIAN_POINT('Ctrl Pts',(3.33118487773593,-1.,2.22955308907221));
#30486=CARTESIAN_POINT('Ctrl Pts',(3.33564495756478,-1.,2.2357525632881));
#30487=CARTESIAN_POINT('Ctrl Pts',(3.34007543738044,-1.,2.24198249391437));
#30488=CARTESIAN_POINT('Ctrl Pts',(3.34447596770768,-1.,2.24824207678288));
#30489=CARTESIAN_POINT('Ctrl Pts',(3.34884690292342,-1.,2.25453097693524));
#30490=CARTESIAN_POINT('Ctrl Pts',(3.35318902552676,-1.,2.26084915222484));
#30491=CARTESIAN_POINT('Ctrl Pts',(3.35750328523077,-1.,2.26719668579921));
#30492=CARTESIAN_POINT('Ctrl Pts',(3.36179055004369,-1.,2.27357362620902));
#30493=CARTESIAN_POINT('Ctrl Pts',(3.36605130712978,-1.,2.27997979457968));
#30494=CARTESIAN_POINT('Ctrl Pts',(3.37028570206357,-1.,2.28641481081045));
#30495=CARTESIAN_POINT('Ctrl Pts',(3.37449367172707,-1.,2.2928781800731));
#30496=CARTESIAN_POINT('Ctrl Pts',(3.37867504959382,-1.,2.29936936127588));
#30497=CARTESIAN_POINT('Ctrl Pts',(3.38282967336676,-1.,2.30588783640389));
#30498=CARTESIAN_POINT('Ctrl Pts',(3.38695751492659,-1.,2.31243319489505));
#30499=CARTESIAN_POINT('Ctrl Pts',(3.39105869475112,-1.,2.31900513925627));
#30500=CARTESIAN_POINT('Ctrl Pts',(3.39513342020045,-1.,2.32560343902683));
#30501=CARTESIAN_POINT('Ctrl Pts',(3.39918194578115,-1.,2.33222789882601));
#30502=CARTESIAN_POINT('Ctrl Pts',(3.40320452776646,-1.,2.33887832342715));
#30503=CARTESIAN_POINT('Ctrl Pts',(3.40720137403888,-1.,2.34555447648901));
#30504=CARTESIAN_POINT('Ctrl Pts',(3.41117262313464,-1.,2.35225606823649));
#30505=CARTESIAN_POINT('Ctrl Pts',(3.4151183675076,-1.,2.35898278606449));
#30506=CARTESIAN_POINT('Ctrl Pts',(3.41903866635384,-1.,2.36573431470314));
#30507=CARTESIAN_POINT('Ctrl Pts',(3.42293356216595,-1.,2.37251035954351));
#30508=CARTESIAN_POINT('Ctrl Pts',(3.42680309755241,-1.,2.37931067029517));
#30509=CARTESIAN_POINT('Ctrl Pts',(3.43064732714472,-1.,2.38613505844641));
#30510=CARTESIAN_POINT('Ctrl Pts',(3.43446630680436,-1.,2.39298338805823));
#30511=CARTESIAN_POINT('Ctrl Pts',(3.43750133066036,-1.,2.39848113411429));
#30512=CARTESIAN_POINT('Ctrl Pts',(3.43976627485223,-1.,2.40261515590099));
#30513=CARTESIAN_POINT('Ctrl Pts',(3.44127120683402,-1.,2.40537592959345));
#30514=CARTESIAN_POINT('Ctrl Pts',(3.44202241512147,-1.,2.40675750623143));
#30515=CARTESIAN_POINT('',(3.35260583073571,-1.,2.52982887637028));
#30516=CARTESIAN_POINT('',(3.44202241512147,-1.,2.40675750623143));
#30517=CARTESIAN_POINT('',(2.90994629141676,-1.,2.36531447826074));
#30518=CARTESIAN_POINT('Ctrl Pts',(3.35260583073571,-1.,2.52982887637028));
#30519=CARTESIAN_POINT('Ctrl Pts',(3.35105973714071,-1.,2.5295413654909));
#30520=CARTESIAN_POINT('Ctrl Pts',(3.34796903576663,-1.,2.52896321610703));
#30521=CARTESIAN_POINT('Ctrl Pts',(3.34333744115511,-1.,2.52808660915689));
#30522=CARTESIAN_POINT('Ctrl Pts',(3.33717089999103,-1.,2.52689902690158));
#30523=CARTESIAN_POINT('Ctrl Pts',(3.32947762187533,-1.,2.52538321164634));
#30524=CARTESIAN_POINT('Ctrl Pts',(3.32179931078699,-1.,2.5238359839626));
#30525=CARTESIAN_POINT('Ctrl Pts',(3.31413607874645,-1.,2.52225724871313));
#30526=CARTESIAN_POINT('Ctrl Pts',(3.30648808815442,-1.,2.52064689568511));
#30527=CARTESIAN_POINT('Ctrl Pts',(3.29885556388352,-1.,2.51900480701069));
#30528=CARTESIAN_POINT('Ctrl Pts',(3.2912387729927,-1.,2.51733085123797));
#30529=CARTESIAN_POINT('Ctrl Pts',(3.28363799702982,-1.,2.51562487464514));
#30530=CARTESIAN_POINT('Ctrl Pts',(3.27605350473142,-1.,2.513886692704));
#30531=CARTESIAN_POINT('Ctrl Pts',(3.26848552888115,-1.,2.51211608411423));
#30532=CARTESIAN_POINT('Ctrl Pts',(3.26093423001434,-1.,2.51031277813486));
#30533=CARTESIAN_POINT('Ctrl Pts',(3.25339971460982,-1.,2.50847647070723));
#30534=CARTESIAN_POINT('Ctrl Pts',(3.24588208983849,-1.,2.506606859405));
#30535=CARTESIAN_POINT('Ctrl Pts',(3.23838151080319,-1.,2.5047036758003));
#30536=CARTESIAN_POINT('Ctrl Pts',(3.23089822320646,-1.,2.50276671338111));
#30537=CARTESIAN_POINT('Ctrl Pts',(3.22343262620503,-1.,2.50079587201958));
#30538=CARTESIAN_POINT('Ctrl Pts',(3.21598526261286,-1.,2.4987911459939));
#30539=CARTESIAN_POINT('Ctrl Pts',(3.20855669849836,-1.,2.4967525264737));
#30540=CARTESIAN_POINT('Ctrl Pts',(3.20114742397588,-1.,2.49467992057755));
#30541=CARTESIAN_POINT('Ctrl Pts',(3.19375775555798,-1.,2.49257307239848));
#30542=CARTESIAN_POINT('Ctrl Pts',(3.18638771282266,-1.,2.49043146334059));
#30543=CARTESIAN_POINT('Ctrl Pts',(3.17903698136622,-1.,2.48825428288201));
#30544=CARTESIAN_POINT('Ctrl Pts',(3.17170518863313,-1.,2.48604065348587));
#30545=CARTESIAN_POINT('Ctrl Pts',(3.16439213290161,-1.,2.48378981792725));
#30546=CARTESIAN_POINT('Ctrl Pts',(3.15709802322739,-1.,2.48150133566571));
#30547=CARTESIAN_POINT('Ctrl Pts',(3.14982373241352,-1.,2.47917529057029));
#30548=CARTESIAN_POINT('Ctrl Pts',(3.1425709954655,-1.,2.47681245356109));
#30549=CARTESIAN_POINT('Ctrl Pts',(3.13534181229295,-1.,2.47441378371932));
#30550=CARTESIAN_POINT('Ctrl Pts',(3.12813790805952,-1.,2.47197997765871));
#30551=CARTESIAN_POINT('Ctrl Pts',(3.12096015766983,-1.,2.46951098947469));
#30552=CARTESIAN_POINT('Ctrl Pts',(3.11380805536122,-1.,2.46700558843506));
#30553=CARTESIAN_POINT('Ctrl Pts',(3.1066790790198,-1.,2.46446082979646));
#30554=CARTESIAN_POINT('Ctrl Pts',(3.09956993697052,-1.,2.46187308501884));
#30555=CARTESIAN_POINT('Ctrl Pts',(3.09247787931887,-1.,2.4592391256388));
#30556=CARTESIAN_POINT('Ctrl Pts',(3.08540206545315,-1.,2.45655725437039));
#30557=CARTESIAN_POINT('Ctrl Pts',(3.07834472886139,-1.,2.4538282678779));
#30558=CARTESIAN_POINT('Ctrl Pts',(3.07131290521297,-1.,2.45105688854422));
#30559=CARTESIAN_POINT('Ctrl Pts',(3.06431596421405,-1.,2.44824970516544));
#30560=CARTESIAN_POINT('Ctrl Pts',(3.05736242671506,-1.,2.44541251892556));
#30561=CARTESIAN_POINT('Ctrl Pts',(3.05045678021504,-1.,2.44254768923105));
#30562=CARTESIAN_POINT('Ctrl Pts',(3.04359685040555,-1.,2.43965194061857));
#30563=CARTESIAN_POINT('Ctrl Pts',(3.03676949672821,-1.,2.43671278042414));
#30564=CARTESIAN_POINT('Ctrl Pts',(3.02995534946978,-1.,2.43371241361488));
#30565=CARTESIAN_POINT('Ctrl Pts',(3.02313656036004,-1.,2.43063415586637));
#30566=CARTESIAN_POINT('Ctrl Pts',(3.01630420830504,-1.,2.42746856264168));
#30567=CARTESIAN_POINT('Ctrl Pts',(3.00946442616658,-1.,2.42421849439613));
#30568=CARTESIAN_POINT('Ctrl Pts',(3.00264868585996,-1.,2.42090763946779));
#30569=CARTESIAN_POINT('Ctrl Pts',(2.99590509293503,-1.,2.41757324500514));
#30570=CARTESIAN_POINT('Ctrl Pts',(2.98927983005796,-1.,2.41425064199586));
#30571=CARTESIAN_POINT('Ctrl Pts',(2.98280015815107,-1.,2.41095909342571));
#30572=CARTESIAN_POINT('Ctrl Pts',(2.97646002822422,-1.,2.40768975073713));
#30573=CARTESIAN_POINT('Ctrl Pts',(2.9701964131236,-1.,2.40438604734919));
#30574=CARTESIAN_POINT('Ctrl Pts',(2.96390432240312,-1.,2.4009556571164));
#30575=CARTESIAN_POINT('Ctrl Pts',(2.95748006482942,-1.,2.39730553974517));
#30576=CARTESIAN_POINT('Ctrl Pts',(2.95085857128439,-1.,2.39337207631667));
#30577=CARTESIAN_POINT('Ctrl Pts',(2.94404820669076,-1.,2.38914929090759));
#30578=CARTESIAN_POINT('Ctrl Pts',(2.93717903280391,-1.,2.38472771516311));
#30579=CARTESIAN_POINT('Ctrl Pts',(2.93049643640206,-1.,2.38028989582073));
#30580=CARTESIAN_POINT('Ctrl Pts',(2.92430340582608,-1.,2.3760651052403));
#30581=CARTESIAN_POINT('Ctrl Pts',(2.91891503791411,-1.,2.37229381109821));
#30582=CARTESIAN_POINT('Ctrl Pts',(2.9146124988314,-1.,2.36919161373173));
#30583=CARTESIAN_POINT('Ctrl Pts',(2.91181344022548,-1.,2.36707658451664));
#30584=CARTESIAN_POINT('Ctrl Pts',(2.91051690822156,-1.,2.36599991765749));
#30585=CARTESIAN_POINT('Ctrl Pts',(2.91005770527719,-1.,2.36553202948613));
#30586=CARTESIAN_POINT('Ctrl Pts',(2.90995756655606,-1.,2.36536211188453));
#30587=CARTESIAN_POINT('Ctrl Pts',(2.90994629141676,-1.,2.36531447826074));
#30588=CARTESIAN_POINT('',(2.79140942341378,-1.,2.50410331873042));
#30589=CARTESIAN_POINT('Origin',(0.,-1.,0.));
#30590=CARTESIAN_POINT('',(3.02314558451372,-1.,2.91557726271063));
#30591=CARTESIAN_POINT('Ctrl Pts',(2.79140942341378,-1.,2.50410331873043));
#30592=CARTESIAN_POINT('Ctrl Pts',(2.79145823440899,-1.,2.50410700351427));
#30593=CARTESIAN_POINT('Ctrl Pts',(2.79164172519039,-1.,2.50417932839343));
#30594=CARTESIAN_POINT('Ctrl Pts',(2.79217568804874,-1.,2.50455968395235));
#30595=CARTESIAN_POINT('Ctrl Pts',(2.79344192164204,-1.,2.50567182569153));
#30596=CARTESIAN_POINT('Ctrl Pts',(2.7959687805717,-1.,2.50810555977564));
#30597=CARTESIAN_POINT('Ctrl Pts',(2.79970585014308,-1.,2.51186983687947));
#30598=CARTESIAN_POINT('Ctrl Pts',(2.80427363984939,-1.,2.51660190466067));
#30599=CARTESIAN_POINT('Ctrl Pts',(2.80941521967234,-1.,2.52205778589922));
#30600=CARTESIAN_POINT('Ctrl Pts',(2.8148437904867,-1.,2.52796388055457));
#30601=CARTESIAN_POINT('Ctrl Pts',(2.82028550483744,-1.,2.53405679667463));
#30602=CARTESIAN_POINT('Ctrl Pts',(2.82552167649157,-1.,2.54012272520141));
#30603=CARTESIAN_POINT('Ctrl Pts',(2.83044254225794,-1.,2.54604736792542));
#30604=CARTESIAN_POINT('Ctrl Pts',(2.83505269592412,-1.,2.55182152806964));
#30605=CARTESIAN_POINT('Ctrl Pts',(2.83942515220699,-1.,2.55749952145165));
#30606=CARTESIAN_POINT('Ctrl Pts',(2.84366802680211,-1.,2.56316920798489));
#30607=CARTESIAN_POINT('Ctrl Pts',(2.84788893329091,-1.,2.56891984251743));
#30608=CARTESIAN_POINT('Ctrl Pts',(2.85215360144482,-1.,2.57480482727128));
#30609=CARTESIAN_POINT('Ctrl Pts',(2.85647171715147,-1.,2.58082875254407));
#30610=CARTESIAN_POINT('Ctrl Pts',(2.86081999003668,-1.,2.5869677064356));
#30611=CARTESIAN_POINT('Ctrl Pts',(2.86515629953528,-1.,2.59318160184921));
#30612=CARTESIAN_POINT('Ctrl Pts',(2.86943633170712,-1.,2.59942875223202));
#30613=CARTESIAN_POINT('Ctrl Pts',(2.87363176656475,-1.,2.6056817788128));
#30614=CARTESIAN_POINT('Ctrl Pts',(2.87773881947885,-1.,2.61193507170928));
#30615=CARTESIAN_POINT('Ctrl Pts',(2.88176821427502,-1.,2.61819596473087));
#30616=CARTESIAN_POINT('Ctrl Pts',(2.88573922195049,-1.,2.62447947640253));
#30617=CARTESIAN_POINT('Ctrl Pts',(2.88967244854243,-1.,2.63080195420771));
#30618=CARTESIAN_POINT('Ctrl Pts',(2.89358228854557,-1.,2.63717442263944));
#30619=CARTESIAN_POINT('Ctrl Pts',(2.89747231723361,-1.,2.64359851684146));
#30620=CARTESIAN_POINT('Ctrl Pts',(2.90133950224879,-1.,2.65007017365576));
#30621=CARTESIAN_POINT('Ctrl Pts',(2.90517678087467,-1.,2.65658188464287));
#30622=CARTESIAN_POINT('Ctrl Pts',(2.90897617968921,-1.,2.66312542616809));
#30623=CARTESIAN_POINT('Ctrl Pts',(2.91273193382876,-1.,2.66969458792627));
#30624=CARTESIAN_POINT('Ctrl Pts',(2.91644290704281,-1.,2.67628728855309));
#30625=CARTESIAN_POINT('Ctrl Pts',(2.92011090722152,-1.,2.68290409279689));
#30626=CARTESIAN_POINT('Ctrl Pts',(2.92373955325876,-1.,2.68954721165342));
#30627=CARTESIAN_POINT('Ctrl Pts',(2.92733294395268,-1.,2.69621932864302));
#30628=CARTESIAN_POINT('Ctrl Pts',(2.93089438233746,-1.,2.70292247416881));
#30629=CARTESIAN_POINT('Ctrl Pts',(2.93442516311167,-1.,2.70965695523776));
#30630=CARTESIAN_POINT('Ctrl Pts',(2.93792519474955,-1.,2.71642190053575));
#30631=CARTESIAN_POINT('Ctrl Pts',(2.94139351933882,-1.,2.72321571511322));
#30632=CARTESIAN_POINT('Ctrl Pts',(2.94482887675139,-1.,2.73003657371613));
#30633=CARTESIAN_POINT('Ctrl Pts',(2.94823023414381,-1.,2.73688288329825));
#30634=CARTESIAN_POINT('Ctrl Pts',(2.95159737214304,-1.,2.7437537949221));
#30635=CARTESIAN_POINT('Ctrl Pts',(2.95493069316211,-1.,2.75064903318996));
#30636=CARTESIAN_POINT('Ctrl Pts',(2.9582309766594,-1.,2.75756867888393));
#30637=CARTESIAN_POINT('Ctrl Pts',(2.96149914764832,-1.,2.76451296269571));
#30638=CARTESIAN_POINT('Ctrl Pts',(2.96473605585548,-1.,2.77148206836464));
#30639=CARTESIAN_POINT('Ctrl Pts',(2.9679422104295,-1.,2.77847589542767));
#30640=CARTESIAN_POINT('Ctrl Pts',(2.97111781461349,-1.,2.78549409123657));
#30641=CARTESIAN_POINT('Ctrl Pts',(2.97426288347475,-1.,2.79253615718147));
#30642=CARTESIAN_POINT('Ctrl Pts',(2.97737733718242,-1.,2.79960153278186));
#30643=CARTESIAN_POINT('Ctrl Pts',(2.98046109647299,-1.,2.80668968101162));
#30644=CARTESIAN_POINT('Ctrl Pts',(2.9835141977994,-1.,2.81380019196454));
#30645=CARTESIAN_POINT('Ctrl Pts',(2.98653680669434,-1.,2.82093279065704));
#30646=CARTESIAN_POINT('Ctrl Pts',(2.98952916401699,-1.,2.82808728190402));
#30647=CARTESIAN_POINT('Ctrl Pts',(2.99249155170479,-1.,2.83526351254383));
#30648=CARTESIAN_POINT('Ctrl Pts',(2.995424253416,-1.,2.84246132984334));
#30649=CARTESIAN_POINT('Ctrl Pts',(2.99832751144566,-1.,2.84968053289104));
#30650=CARTESIAN_POINT('Ctrl Pts',(3.0012015079552,-1.,2.85692085715129));
#30651=CARTESIAN_POINT('Ctrl Pts',(3.00404638316245,-1.,2.86418200833065));
#30652=CARTESIAN_POINT('Ctrl Pts',(3.00686224485374,-1.,2.87146368430104));
#30653=CARTESIAN_POINT('Ctrl Pts',(3.0096491810855,-1.,2.87876560072799));
#30654=CARTESIAN_POINT('Ctrl Pts',(3.01240727309568,-1.,2.88608751706796));
#30655=CARTESIAN_POINT('Ctrl Pts',(3.01513660433291,-1.,2.8934292556764));
#30656=CARTESIAN_POINT('Ctrl Pts',(3.01783725123646,-1.,2.90079069102661));
#30657=CARTESIAN_POINT('Ctrl Pts',(3.01997487194926,-1.,2.90669553303902));
#30658=CARTESIAN_POINT('Ctrl Pts',(3.02156522743299,-1.,2.91113297349052));
#30659=CARTESIAN_POINT('Ctrl Pts',(3.02261975104912,-1.,2.91409518070707));
#30660=CARTESIAN_POINT('Ctrl Pts',(3.02314558451372,-1.,2.91557726271063));
#30661=CARTESIAN_POINT('',(2.91557726271063,-1.,3.02314558451372));
#30662=CARTESIAN_POINT('',(3.02314558451372,-1.,2.91557726271063));
#30663=CARTESIAN_POINT('',(2.50410331873176,-1.,2.79140942341258));
#30664=CARTESIAN_POINT('Ctrl Pts',(2.91557726271063,-1.,3.02314558451372));
#30665=CARTESIAN_POINT('Ctrl Pts',(2.91409518070399,-1.,3.02261975104593));
#30666=CARTESIAN_POINT('Ctrl Pts',(2.91113297348212,-1.,3.02156522742431));
#30667=CARTESIAN_POINT('Ctrl Pts',(2.90669553302526,-1.,3.01997487193503));
#30668=CARTESIAN_POINT('Ctrl Pts',(2.9007906910105,-1.,3.01783725121981));
#30669=CARTESIAN_POINT('Ctrl Pts',(2.89342925566321,-1.,3.01513660431928));
#30670=CARTESIAN_POINT('Ctrl Pts',(2.8860875170608,-1.,3.01240727308829));
#30671=CARTESIAN_POINT('Ctrl Pts',(2.87876560072727,-1.,3.00964918108476));
#30672=CARTESIAN_POINT('Ctrl Pts',(2.87146368430501,-1.,3.00686224485784));
#30673=CARTESIAN_POINT('Ctrl Pts',(2.86418200833667,-1.,3.00404638316867));
#30674=CARTESIAN_POINT('Ctrl Pts',(2.85692085715685,-1.,3.00120150796095));
#30675=CARTESIAN_POINT('Ctrl Pts',(2.84968053289451,-1.,2.99832751144925));
#30676=CARTESIAN_POINT('Ctrl Pts',(2.84246132984415,-1.,2.99542425341685));
#30677=CARTESIAN_POINT('Ctrl Pts',(2.83526351254248,-1.,2.9924915517034));
#30678=CARTESIAN_POINT('Ctrl Pts',(2.82808728190157,-1.,2.98952916401446));
#30679=CARTESIAN_POINT('Ctrl Pts',(2.82093279065457,-1.,2.9865368066918));
#30680=CARTESIAN_POINT('Ctrl Pts',(2.81380019196286,-1.,2.98351419779767));
#30681=CARTESIAN_POINT('Ctrl Pts',(2.80668968101106,-1.,2.98046109647241));
#30682=CARTESIAN_POINT('Ctrl Pts',(2.7996015327823,-1.,2.97737733718287));
#30683=CARTESIAN_POINT('Ctrl Pts',(2.79253615718248,-1.,2.9742628834758));
#30684=CARTESIAN_POINT('Ctrl Pts',(2.78549409123769,-1.,2.97111781461465));
#30685=CARTESIAN_POINT('Ctrl Pts',(2.7784758954285,-1.,2.96794221043036));
#30686=CARTESIAN_POINT('Ctrl Pts',(2.77148206836498,-1.,2.96473605585583));
#30687=CARTESIAN_POINT('Ctrl Pts',(2.76451296269557,-1.,2.96149914764818));
#30688=CARTESIAN_POINT('Ctrl Pts',(2.7575686788835,-1.,2.95823097665896));
#30689=CARTESIAN_POINT('Ctrl Pts',(2.75064903318947,-1.,2.95493069316161));
#30690=CARTESIAN_POINT('Ctrl Pts',(2.74375379492172,-1.,2.95159737214266));
#30691=CARTESIAN_POINT('Ctrl Pts',(2.73688288329808,-1.,2.94823023414364));
#30692=CARTESIAN_POINT('Ctrl Pts',(2.73003657371616,-1.,2.94482887675143));
#30693=CARTESIAN_POINT('Ctrl Pts',(2.72321571511337,-1.,2.94139351933897));
#30694=CARTESIAN_POINT('Ctrl Pts',(2.71642190053592,-1.,2.93792519474972));
#30695=CARTESIAN_POINT('Ctrl Pts',(2.70965695523787,-1.,2.93442516311179));
#30696=CARTESIAN_POINT('Ctrl Pts',(2.70292247416885,-1.,2.9308943823375));
#30697=CARTESIAN_POINT('Ctrl Pts',(2.69621932864301,-1.,2.92733294395267));
#30698=CARTESIAN_POINT('Ctrl Pts',(2.68954721165339,-1.,2.92373955325875));
#30699=CARTESIAN_POINT('Ctrl Pts',(2.68290409279688,-1.,2.92011090722152));
#30700=CARTESIAN_POINT('Ctrl Pts',(2.67628728855312,-1.,2.91644290704285));
#30701=CARTESIAN_POINT('Ctrl Pts',(2.66969458792631,-1.,2.91273193382882));
#30702=CARTESIAN_POINT('Ctrl Pts',(2.6631254261681,-1.,2.90897617968923));
#30703=CARTESIAN_POINT('Ctrl Pts',(2.65658188464282,-1.,2.90517678087461));
#30704=CARTESIAN_POINT('Ctrl Pts',(2.65007017365564,-1.,2.90133950224867));
#30705=CARTESIAN_POINT('Ctrl Pts',(2.64359851684131,-1.,2.89747231723345));
#30706=CARTESIAN_POINT('Ctrl Pts',(2.63717442263932,-1.,2.89358228854544));
#30707=CARTESIAN_POINT('Ctrl Pts',(2.63080195420767,-1.,2.88967244854239));
#30708=CARTESIAN_POINT('Ctrl Pts',(2.62447947640262,-1.,2.88573922195059));
#30709=CARTESIAN_POINT('Ctrl Pts',(2.61819596473108,-1.,2.88176821427525));
#30710=CARTESIAN_POINT('Ctrl Pts',(2.61193507170955,-1.,2.87773881947916));
#30711=CARTESIAN_POINT('Ctrl Pts',(2.60568177881303,-1.,2.87363176656501));
#30712=CARTESIAN_POINT('Ctrl Pts',(2.5994287522321,-1.,2.86943633170722));
#30713=CARTESIAN_POINT('Ctrl Pts',(2.59318160184908,-1.,2.86515629953513));
#30714=CARTESIAN_POINT('Ctrl Pts',(2.58696770643524,-1.,2.86081999003629));
#30715=CARTESIAN_POINT('Ctrl Pts',(2.58082875254357,-1.,2.85647171715092));
#30716=CARTESIAN_POINT('Ctrl Pts',(2.57480482727081,-1.,2.85215360144431));
#30717=CARTESIAN_POINT('Ctrl Pts',(2.56891984251721,-1.,2.84788893329067));
#30718=CARTESIAN_POINT('Ctrl Pts',(2.56316920798513,-1.,2.84366802680237));
#30719=CARTESIAN_POINT('Ctrl Pts',(2.55749952145241,-1.,2.83942515220782));
#30720=CARTESIAN_POINT('Ctrl Pts',(2.55182152807077,-1.,2.83505269592536));
#30721=CARTESIAN_POINT('Ctrl Pts',(2.54604736792655,-1.,2.83044254225917));
#30722=CARTESIAN_POINT('Ctrl Pts',(2.54012272520199,-1.,2.8255216764922));
#30723=CARTESIAN_POINT('Ctrl Pts',(2.53405679667412,-1.,2.82028550483689));
#30724=CARTESIAN_POINT('Ctrl Pts',(2.52796388055278,-1.,2.81484379048475));
#30725=CARTESIAN_POINT('Ctrl Pts',(2.52205778589653,-1.,2.80941521966941));
#30726=CARTESIAN_POINT('Ctrl Pts',(2.51660190465805,-1.,2.80427363984653));
#30727=CARTESIAN_POINT('Ctrl Pts',(2.51186983687818,-1.,2.79970585014168));
#30728=CARTESIAN_POINT('Ctrl Pts',(2.5081055597767,-1.,2.79596878057287));
#30729=CARTESIAN_POINT('Ctrl Pts',(2.50567182569081,-1.,2.79344192164147));
#30730=CARTESIAN_POINT('Ctrl Pts',(2.50455968395146,-1.,2.79217568804755));
#30731=CARTESIAN_POINT('Ctrl Pts',(2.50417932839313,-1.,2.79164172518905));
#30732=CARTESIAN_POINT('Ctrl Pts',(2.50410700351493,-1.,2.79145823440781));
#30733=CARTESIAN_POINT('Ctrl Pts',(2.50410331873176,-1.,2.79140942341258));
#30734=CARTESIAN_POINT('',(2.36531447826213,-1.,2.90994629141563));
#30735=CARTESIAN_POINT('Origin',(0.,-1.,0.));
#30736=CARTESIAN_POINT('',(2.52982887637028,-1.,3.35260583073571));
#30737=CARTESIAN_POINT('Ctrl Pts',(2.36531447826213,-1.,2.90994629141563));
#30738=CARTESIAN_POINT('Ctrl Pts',(2.3653621118858,-1.,2.90995756655559));
#30739=CARTESIAN_POINT('Ctrl Pts',(2.36553202948741,-1.,2.9100577052777));
#30740=CARTESIAN_POINT('Ctrl Pts',(2.36599991765853,-1.,2.91051690822262));
#30741=CARTESIAN_POINT('Ctrl Pts',(2.36707658451709,-1.,2.91181344022628));
#30742=CARTESIAN_POINT('Ctrl Pts',(2.36919161373074,-1.,2.91461249883016));
#30743=CARTESIAN_POINT('Ctrl Pts',(2.37229381109939,-1.,2.9189150379156));
#30744=CARTESIAN_POINT('Ctrl Pts',(2.37606510524271,-1.,2.92430340582912));
#30745=CARTESIAN_POINT('Ctrl Pts',(2.3802898958232,-1.,2.93049643640517));
#30746=CARTESIAN_POINT('Ctrl Pts',(2.38472771516476,-1.,2.93717903280599));
#30747=CARTESIAN_POINT('Ctrl Pts',(2.38914929090806,-1.,2.94404820669135));
#30748=CARTESIAN_POINT('Ctrl Pts',(2.39337207631613,-1.,2.95085857128372));
#30749=CARTESIAN_POINT('Ctrl Pts',(2.39730553974412,-1.,2.95748006482811));
#30750=CARTESIAN_POINT('Ctrl Pts',(2.40095565711535,-1.,2.96390432240181));
#30751=CARTESIAN_POINT('Ctrl Pts',(2.40438604734848,-1.,2.97019641312272));
#30752=CARTESIAN_POINT('Ctrl Pts',(2.40768975073691,-1.,2.97646002822395));
#30753=CARTESIAN_POINT('Ctrl Pts',(2.41095909342591,-1.,2.98280015815132));
#30754=CARTESIAN_POINT('Ctrl Pts',(2.4142506419963,-1.,2.98927983005851));
#30755=CARTESIAN_POINT('Ctrl Pts',(2.4175732450056,-1.,2.99590509293561));
#30756=CARTESIAN_POINT('Ctrl Pts',(2.42090763946812,-1.,3.00264868586038));
#30757=CARTESIAN_POINT('Ctrl Pts',(2.42421849439625,-1.,3.00946442616674));
#30758=CARTESIAN_POINT('Ctrl Pts',(2.4274685626416,-1.,3.01630420830494));
#30759=CARTESIAN_POINT('Ctrl Pts',(2.43063415586615,-1.,3.02313656035977));
#30760=CARTESIAN_POINT('Ctrl Pts',(2.43371241361462,-1.,3.02995534946946));
#30761=CARTESIAN_POINT('Ctrl Pts',(2.43671278042394,-1.,3.03676949672797));
#30762=CARTESIAN_POINT('Ctrl Pts',(2.43965194061849,-1.,3.04359685040545));
#30763=CARTESIAN_POINT('Ctrl Pts',(2.44254768923109,-1.,3.05045678021509));
#30764=CARTESIAN_POINT('Ctrl Pts',(2.44541251892568,-1.,3.05736242671521));
#30765=CARTESIAN_POINT('Ctrl Pts',(2.44824970516557,-1.,3.06431596421422));
#30766=CARTESIAN_POINT('Ctrl Pts',(2.45105688854432,-1.,3.0713129052131));
#30767=CARTESIAN_POINT('Ctrl Pts',(2.45382826787795,-1.,3.07834472886145));
#30768=CARTESIAN_POINT('Ctrl Pts',(2.45655725437037,-1.,3.08540206545313));
#30769=CARTESIAN_POINT('Ctrl Pts',(2.45923912563875,-1.,3.09247787931881));
#30770=CARTESIAN_POINT('Ctrl Pts',(2.4618730850188,-1.,3.09956993697048));
#30771=CARTESIAN_POINT('Ctrl Pts',(2.46446082979645,-1.,3.10667907901981));
#30772=CARTESIAN_POINT('Ctrl Pts',(2.46700558843507,-1.,3.11380805536124));
#30773=CARTESIAN_POINT('Ctrl Pts',(2.4695109894747,-1.,3.12096015766984));
#30774=CARTESIAN_POINT('Ctrl Pts',(2.47197997765868,-1.,3.12813790805948));
#30775=CARTESIAN_POINT('Ctrl Pts',(2.47441378371923,-1.,3.13534181229282));
#30776=CARTESIAN_POINT('Ctrl Pts',(2.47681245356095,-1.,3.14257099546531));
#30777=CARTESIAN_POINT('Ctrl Pts',(2.47917529057016,-1.,3.14982373241335));
#30778=CARTESIAN_POINT('Ctrl Pts',(2.48150133566568,-1.,3.15709802322735));
#30779=CARTESIAN_POINT('Ctrl Pts',(2.48378981792739,-1.,3.16439213290181));
#30780=CARTESIAN_POINT('Ctrl Pts',(2.48604065348619,-1.,3.17170518863357));
#30781=CARTESIAN_POINT('Ctrl Pts',(2.48825428288242,-1.,3.17903698136679));
#30782=CARTESIAN_POINT('Ctrl Pts',(2.49043146334095,-1.,3.18638771282315));
#30783=CARTESIAN_POINT('Ctrl Pts',(2.4925730723986,-1.,3.19375775555814));
#30784=CARTESIAN_POINT('Ctrl Pts',(2.49467992057726,-1.,3.20114742397549));
#30785=CARTESIAN_POINT('Ctrl Pts',(2.49675252647298,-1.,3.2085566984974));
#30786=CARTESIAN_POINT('Ctrl Pts',(2.49879114599293,-1.,3.21598526261157));
#30787=CARTESIAN_POINT('Ctrl Pts',(2.5007958720187,-1.,3.22343262620387));
#30788=CARTESIAN_POINT('Ctrl Pts',(2.50276671338074,-1.,3.23089822320596));
#30789=CARTESIAN_POINT('Ctrl Pts',(2.50470367580078,-1.,3.23838151080383));
#30790=CARTESIAN_POINT('Ctrl Pts',(2.50660685940645,-1.,3.24588208984042));
#30791=CARTESIAN_POINT('Ctrl Pts',(2.50847647070936,-1.,3.25339971461265));
#30792=CARTESIAN_POINT('Ctrl Pts',(2.51031277813697,-1.,3.26093423001716));
#30793=CARTESIAN_POINT('Ctrl Pts',(2.51211608411539,-1.,3.26848552888271));
#30794=CARTESIAN_POINT('Ctrl Pts',(2.51388669270329,-1.,3.27605350473048));
#30795=CARTESIAN_POINT('Ctrl Pts',(2.51562487464214,-1.,3.28363799702583));
#30796=CARTESIAN_POINT('Ctrl Pts',(2.51733085123316,-1.,3.2912387729863));
#30797=CARTESIAN_POINT('Ctrl Pts',(2.51900480700548,-1.,3.29885556387661));
#30798=CARTESIAN_POINT('Ctrl Pts',(2.52064689568167,-1.,3.30648808814986));
#30799=CARTESIAN_POINT('Ctrl Pts',(2.52225724871375,-1.,3.31413607874727));
#30800=CARTESIAN_POINT('Ctrl Pts',(2.52383598396878,-1.,3.32179931079521));
#30801=CARTESIAN_POINT('Ctrl Pts',(2.52538321165774,-1.,3.32947762189049));
#30802=CARTESIAN_POINT('Ctrl Pts',(2.52689902691551,-1.,3.33717090000955));
#30803=CARTESIAN_POINT('Ctrl Pts',(2.52808660916879,-1.,3.34333744117093));
#30804=CARTESIAN_POINT('Ctrl Pts',(2.5289632161143,-1.,3.34796903577628));
#30805=CARTESIAN_POINT('Ctrl Pts',(2.52954136549357,-1.,3.35105973714426));
#30806=CARTESIAN_POINT('Ctrl Pts',(2.52982887637028,-1.,3.35260583073571));
#30807=CARTESIAN_POINT('',(2.40675750623143,-1.,3.44202241512147));
#30808=CARTESIAN_POINT('',(2.52982887637028,-1.,3.35260583073571));
#30809=CARTESIAN_POINT('',(2.03660101169714,-1.,3.14877060440328));
#30810=CARTESIAN_POINT('Ctrl Pts',(2.40675750623143,-1.,3.44202241512147));
#30811=CARTESIAN_POINT('Ctrl Pts',(2.4053759295909,-1.,3.44127120683039));
#30812=CARTESIAN_POINT('Ctrl Pts',(2.40261515589405,-1.,3.43976627484234));
#30813=CARTESIAN_POINT('Ctrl Pts',(2.39848113410292,-1.,3.43750133064416));
#30814=CARTESIAN_POINT('Ctrl Pts',(2.39298338804493,-1.,3.4344663067854));
#30815=CARTESIAN_POINT('Ctrl Pts',(2.38613505843552,-1.,3.4306473271292));
#30816=CARTESIAN_POINT('Ctrl Pts',(2.37931067028926,-1.,3.42680309754399));
#30817=CARTESIAN_POINT('Ctrl Pts',(2.37251035954292,-1.,3.42293356216511));
#30818=CARTESIAN_POINT('Ctrl Pts',(2.36573431470642,-1.,3.41903866635852));
#30819=CARTESIAN_POINT('Ctrl Pts',(2.35898278606946,-1.,3.41511836751469));
#30820=CARTESIAN_POINT('Ctrl Pts',(2.35225606824109,-1.,3.41117262314119));
#30821=CARTESIAN_POINT('Ctrl Pts',(2.34555447649188,-1.,3.40720137404297));
#30822=CARTESIAN_POINT('Ctrl Pts',(2.33887832342782,-1.,3.40320452776743));
#30823=CARTESIAN_POINT('Ctrl Pts',(2.33222789882489,-1.,3.39918194577956));
#30824=CARTESIAN_POINT('Ctrl Pts',(2.3256034390248,-1.,3.39513342019756));
#30825=CARTESIAN_POINT('Ctrl Pts',(2.31900513925424,-1.,3.39105869474822));
#30826=CARTESIAN_POINT('Ctrl Pts',(2.31243319489367,-1.,3.38695751492462));
#30827=CARTESIAN_POINT('Ctrl Pts',(2.30588783640343,-1.,3.3828296733661));
#30828=CARTESIAN_POINT('Ctrl Pts',(2.29936936127624,-1.,3.37867504959433));
#30829=CARTESIAN_POINT('Ctrl Pts',(2.29287818007393,-1.,3.37449367172826));
#30830=CARTESIAN_POINT('Ctrl Pts',(2.28641481081137,-1.,3.37028570206488));
#30831=CARTESIAN_POINT('Ctrl Pts',(2.27997979458037,-1.,3.36605130713076));
#30832=CARTESIAN_POINT('Ctrl Pts',(2.2735736262093,-1.,3.36179055004409));
#30833=CARTESIAN_POINT('Ctrl Pts',(2.26719668579909,-1.,3.35750328523061));
#30834=CARTESIAN_POINT('Ctrl Pts',(2.26084915222449,-1.,3.35318902552626));
#30835=CARTESIAN_POINT('Ctrl Pts',(2.25453097693483,-1.,3.34884690292285));
#30836=CARTESIAN_POINT('Ctrl Pts',(2.24824207678256,-1.,3.34447596770723));
#30837=CARTESIAN_POINT('Ctrl Pts',(2.24198249391422,-1.,3.34007543738025));
#30838=CARTESIAN_POINT('Ctrl Pts',(2.23575256328812,-1.,3.33564495756482));
#30839=CARTESIAN_POINT('Ctrl Pts',(2.22955308907233,-1.,3.33118487773611));
#30840=CARTESIAN_POINT('Ctrl Pts',(2.22338548312772,-1.,3.3266964672289));
#30841=CARTESIAN_POINT('Ctrl Pts',(2.21725135110898,-1.,3.32218125618968));
#30842=CARTESIAN_POINT('Ctrl Pts',(2.21115211847875,-1.,3.31764044024235));
#30843=CARTESIAN_POINT('Ctrl Pts',(2.20508863150607,-1.,3.31307424608949));
#30844=CARTESIAN_POINT('Ctrl Pts',(2.19906078949922,-1.,3.30848134694595));
#30845=CARTESIAN_POINT('Ctrl Pts',(2.19306710376111,-1.,3.30385816281831));
#30846=CARTESIAN_POINT('Ctrl Pts',(2.18710556500327,-1.,3.29920022557639));
#30847=CARTESIAN_POINT('Ctrl Pts',(2.18117455557065,-1.,3.2945036150049));
#30848=CARTESIAN_POINT('Ctrl Pts',(2.17527380048423,-1.,3.28976645712568));
#30849=CARTESIAN_POINT('Ctrl Pts',(2.16940517773455,-1.,3.28499019979724));
#30850=CARTESIAN_POINT('Ctrl Pts',(2.16357391934425,-1.,3.280181508414));
#30851=CARTESIAN_POINT('Ctrl Pts',(2.15778690038347,-1.,3.27534954469187));
#30852=CARTESIAN_POINT('Ctrl Pts',(2.15205043199808,-1.,3.27050245897228));
#30853=CARTESIAN_POINT('Ctrl Pts',(2.1463680529566,-1.,3.26564388189759));
#30854=CARTESIAN_POINT('Ctrl Pts',(2.14073870754264,-1.,3.26077002641879));
#30855=CARTESIAN_POINT('Ctrl Pts',(2.13515375878803,-1.,3.25586495065054));
#30856=CARTESIAN_POINT('Ctrl Pts',(2.12960028396832,-1.,3.25090574494028));
#30857=CARTESIAN_POINT('Ctrl Pts',(2.12406646410962,-1.,3.24587102613376));
#30858=CARTESIAN_POINT('Ctrl Pts',(2.11854673326979,-1.,3.24074905517293));
#30859=CARTESIAN_POINT('Ctrl Pts',(2.11304604021773,-1.,3.23554444767099));
#30860=CARTESIAN_POINT('Ctrl Pts',(2.10758699642451,-1.,3.23028945793289));
#30861=CARTESIAN_POINT('Ctrl Pts',(2.10220384298492,-1.,3.22503437553434));
#30862=CARTESIAN_POINT('Ctrl Pts',(2.09692958434895,-1.,3.21982707347009));
#30863=CARTESIAN_POINT('Ctrl Pts',(2.09178419460443,-1.,3.21469429601654));
#30864=CARTESIAN_POINT('Ctrl Pts',(2.08676465517455,-1.,3.20962575845463));
#30865=CARTESIAN_POINT('Ctrl Pts',(2.08182850370878,-1.,3.2045481863073));
#30866=CARTESIAN_POINT('Ctrl Pts',(2.07690441870722,-1.,3.19934132836019));
#30867=CARTESIAN_POINT('Ctrl Pts',(2.07192253497857,-1.,3.19388465568252));
#30868=CARTESIAN_POINT('Ctrl Pts',(2.06684062744112,-1.,3.18809755562368));
#30869=CARTESIAN_POINT('Ctrl Pts',(2.06166849827101,-1.,3.18197692964614));
#30870=CARTESIAN_POINT('Ctrl Pts',(2.05650186773132,-1.,3.17564906975371));
#30871=CARTESIAN_POINT('Ctrl Pts',(2.05151770247233,-1.,3.16936341689527));
#30872=CARTESIAN_POINT('Ctrl Pts',(2.04693331247446,-1.,3.16343165058912));
#30873=CARTESIAN_POINT('Ctrl Pts',(2.04297406404027,-1.,3.15817983946367));
#30874=CARTESIAN_POINT('Ctrl Pts',(2.03984073791519,-1.,3.15389991674792));
#30875=CARTESIAN_POINT('Ctrl Pts',(2.03783225495961,-1.,3.15102344775328));
#30876=CARTESIAN_POINT('Ctrl Pts',(2.03693188810544,-1.,3.14959882629805));
#30877=CARTESIAN_POINT('Ctrl Pts',(2.03663974554932,-1.,3.1490119366901));
#30878=CARTESIAN_POINT('Ctrl Pts',(2.03659701539259,-1.,3.14881939088124));
#30879=CARTESIAN_POINT('Ctrl Pts',(2.03660101169714,-1.,3.14877060440328));
#30880=CARTESIAN_POINT('',(1.88097764062697,-1.,3.24413672884812));
#30881=CARTESIAN_POINT('Origin',(0.,-1.,0.));
#30882=CARTESIAN_POINT('',(1.97421938526992,-1.,3.70708211654725));
#30883=CARTESIAN_POINT('Ctrl Pts',(1.88097764062697,-1.,3.24413672884812));
#30884=CARTESIAN_POINT('Ctrl Pts',(1.8810229239812,-1.,3.24415531671284));
#30885=CARTESIAN_POINT('Ctrl Pts',(1.88117508446775,-1.,3.24428080353022));
#30886=CARTESIAN_POINT('Ctrl Pts',(1.88156537699203,-1.,3.24480754676064));
#30887=CARTESIAN_POINT('Ctrl Pts',(1.88242596600454,-1.,3.2462565441079));
#30888=CARTESIAN_POINT('Ctrl Pts',(1.88407708646357,-1.,3.24935200511918));
#30889=CARTESIAN_POINT('Ctrl Pts',(1.88646802523466,-1.,3.25408686339463));
#30890=CARTESIAN_POINT('Ctrl Pts',(1.88934996203698,-1.,3.25999885193947));
#30891=CARTESIAN_POINT('Ctrl Pts',(1.89255393500965,-1.,3.26677653888676));
#30892=CARTESIAN_POINT('Ctrl Pts',(1.89589172903793,-1.,3.27407108933139));
#30893=CARTESIAN_POINT('Ctrl Pts',(1.89918429230462,-1.,3.28154737912352));
#30894=CARTESIAN_POINT('Ctrl Pts',(1.90228971247527,-1.,3.2889344860029));
#30895=CARTESIAN_POINT('Ctrl Pts',(1.90513891864087,-1.,3.29608978722113));
#30896=CARTESIAN_POINT('Ctrl Pts',(1.90773912171341,-1.,3.30300595568195));
#30897=CARTESIAN_POINT('Ctrl Pts',(1.91014297830446,-1.,3.30975721158596));
#30898=CARTESIAN_POINT('Ctrl Pts',(1.91242616234442,-1.,3.31646052426364));
#30899=CARTESIAN_POINT('Ctrl Pts',(1.91466343916627,-1.,3.32323403454535));
#30900=CARTESIAN_POINT('Ctrl Pts',(1.91690081930331,-1.,3.33014884257873));
#30901=CARTESIAN_POINT('Ctrl Pts',(1.9191460961021,-1.,3.33721230710012));
#30902=CARTESIAN_POINT('Ctrl Pts',(1.92138450828404,-1.,3.34439448941961));
#30903=CARTESIAN_POINT('Ctrl Pts',(1.92358838440528,-1.,3.35164424847223));
#30904=CARTESIAN_POINT('Ctrl Pts',(1.92572846125756,-1.,3.35890824422965));
#30905=CARTESIAN_POINT('Ctrl Pts',(1.92778626543786,-1.,3.36615168657567));
#30906=CARTESIAN_POINT('Ctrl Pts',(1.92975993109877,-1.,3.37336807068043));
#30907=CARTESIAN_POINT('Ctrl Pts',(1.93165739093276,-1.,3.3805676852555));
#30908=CARTESIAN_POINT('Ctrl Pts',(1.93349233176788,-1.,3.38777076883256));
#30909=CARTESIAN_POINT('Ctrl Pts',(1.93527929945985,-1.,3.39499923640795));
#30910=CARTESIAN_POINT('Ctrl Pts',(1.93702857723098,-1.,3.40226802104109));
#30911=CARTESIAN_POINT('Ctrl Pts',(1.93874306008143,-1.,3.40957978266642));
#30912=CARTESIAN_POINT('Ctrl Pts',(1.94042111965246,-1.,3.41692971994096));
#30913=CARTESIAN_POINT('Ctrl Pts',(1.94205835913696,-1.,3.42430850941503));
#30914=CARTESIAN_POINT('Ctrl Pts',(1.94364973660284,-1.,3.43170586602434));
#30915=CARTESIAN_POINT('Ctrl Pts',(1.94519168842879,-1.,3.43911410197687));
#30916=CARTESIAN_POINT('Ctrl Pts',(1.94668377715329,-1.,3.44653088665681));
#30917=CARTESIAN_POINT('Ctrl Pts',(1.94812754766524,-1.,3.45395731584051));
#30918=CARTESIAN_POINT('Ctrl Pts',(1.94952575850197,-1.,3.46139661060962));
#30919=CARTESIAN_POINT('Ctrl Pts',(1.95088147859876,-1.,3.46885258974191));
#30920=CARTESIAN_POINT('Ctrl Pts',(1.95219722189876,-1.,3.47632820495921));
#30921=CARTESIAN_POINT('Ctrl Pts',(1.95347412486308,-1.,3.48382414832634));
#30922=CARTESIAN_POINT('Ctrl Pts',(1.95471236969643,-1.,3.49133956289133));
#30923=CARTESIAN_POINT('Ctrl Pts',(1.95591153823661,-1.,3.49887263575583));
#30924=CARTESIAN_POINT('Ctrl Pts',(1.95707099606511,-1.,3.50642124159909));
#30925=CARTESIAN_POINT('Ctrl Pts',(1.95819025316779,-1.,3.51398354617794));
#30926=CARTESIAN_POINT('Ctrl Pts',(1.95926936324461,-1.,3.52155867431486));
#30927=CARTESIAN_POINT('Ctrl Pts',(1.96030879411566,-1.,3.52914648844351));
#30928=CARTESIAN_POINT('Ctrl Pts',(1.96130926212689,-1.,3.53674730625813));
#30929=CARTESIAN_POINT('Ctrl Pts',(1.96227157573067,-1.,3.54436163300443));
#30930=CARTESIAN_POINT('Ctrl Pts',(1.96319648628644,-1.,3.55198990600886));
#30931=CARTESIAN_POINT('Ctrl Pts',(1.96408450906812,-1.,3.55963218706096));
#30932=CARTESIAN_POINT('Ctrl Pts',(1.96493594634567,-1.,3.56728820357791));
#30933=CARTESIAN_POINT('Ctrl Pts',(1.96575096652789,-1.,3.57495748600959));
#30934=CARTESIAN_POINT('Ctrl Pts',(1.96652966688911,-1.,3.58263947663829));
#30935=CARTESIAN_POINT('Ctrl Pts',(1.96727213799544,-1.,3.59033364022801));
#30936=CARTESIAN_POINT('Ctrl Pts',(1.96797854118369,-1.,3.59803959819938));
#30937=CARTESIAN_POINT('Ctrl Pts',(1.9686491188594,-1.,3.60575714017989));
#30938=CARTESIAN_POINT('Ctrl Pts',(1.96928416040877,-1.,3.61348615496704));
#30939=CARTESIAN_POINT('Ctrl Pts',(1.96988398129978,-1.,3.62122658401893));
#30940=CARTESIAN_POINT('Ctrl Pts',(1.97044889850463,-1.,3.62897836973293));
#30941=CARTESIAN_POINT('Ctrl Pts',(1.97097920454464,-1.,3.63674139590412));
#30942=CARTESIAN_POINT('Ctrl Pts',(1.97147515441164,-1.,3.64451546723514));
#30943=CARTESIAN_POINT('Ctrl Pts',(1.97193697240239,-1.,3.652300347166));
#30944=CARTESIAN_POINT('Ctrl Pts',(1.9723648543905,-1.,3.6600957816636));
#30945=CARTESIAN_POINT('Ctrl Pts',(1.97275897198678,-1.,3.66790152752075));
#30946=CARTESIAN_POINT('Ctrl Pts',(1.97311947678516,-1.,3.67571738107084));
#30947=CARTESIAN_POINT('Ctrl Pts',(1.97344650304519,-1.,3.68354319915092));
#30948=CARTESIAN_POINT('Ctrl Pts',(1.97374016225483,-1.,3.69137888599902));
#30949=CARTESIAN_POINT('Ctrl Pts',(1.97394846383216,-1.,3.6976552856004));
#30950=CARTESIAN_POINT('Ctrl Pts',(1.97408973726715,-1.,3.70236698912904));
#30951=CARTESIAN_POINT('Ctrl Pts',(1.97417727645308,-1.,3.70551008132332));
#30952=CARTESIAN_POINT('Ctrl Pts',(1.97421938526992,-1.,3.70708211654725));
#30953=CARTESIAN_POINT('',(1.8386753923786,-1.,3.77614523045147));
#30954=CARTESIAN_POINT('',(1.97421938526992,-1.,3.70708211654725));
#30955=CARTESIAN_POINT('',(1.5189508286633,-1.,3.42859860294306));
#30956=CARTESIAN_POINT('Ctrl Pts',(1.8386753923786,-1.,3.77614523045147));
#30957=CARTESIAN_POINT('Ctrl Pts',(1.83742834010626,-1.,3.77518714457833));
#30958=CARTESIAN_POINT('Ctrl Pts',(1.83493697934534,-1.,3.77326886064398));
#30959=CARTESIAN_POINT('Ctrl Pts',(1.83120816955645,-1.,3.77038509817999));
#30960=CARTESIAN_POINT('Ctrl Pts',(1.82625289220915,-1.,3.76652740353775));
#30961=CARTESIAN_POINT('Ctrl Pts',(1.82008629694091,-1.,3.76168412707948));
#30962=CARTESIAN_POINT('Ctrl Pts',(1.8139472983358,-1.,3.75681965683071));
#30963=CARTESIAN_POINT('Ctrl Pts',(1.80783603939617,-1.,3.75193395887977));
#30964=CARTESIAN_POINT('Ctrl Pts',(1.8017527148577,-1.,3.74702700875467));
#30965=CARTESIAN_POINT('Ctrl Pts',(1.79569757859422,-1.,3.74209880352445));
#30966=CARTESIAN_POINT('Ctrl Pts',(1.78967092823491,-1.,3.73714934730681));
#30967=CARTESIAN_POINT('Ctrl Pts',(1.78367308442901,-1.,3.7321786309547));
#30968=CARTESIAN_POINT('Ctrl Pts',(1.77770437039658,-1.,3.72718661205609));
#30969=CARTESIAN_POINT('Ctrl Pts',(1.77176509401761,-1.,3.72217319911254));
#30970=CARTESIAN_POINT('Ctrl Pts',(1.76585552124394,-1.,3.71713822377359));
#30971=CARTESIAN_POINT('Ctrl Pts',(1.75997588498865,-1.,3.71208146346136));
#30972=CARTESIAN_POINT('Ctrl Pts',(1.75412641804042,-1.,3.70700269736659));
#30973=CARTESIAN_POINT('Ctrl Pts',(1.74830738046057,-1.,3.7019017567335));
#30974=CARTESIAN_POINT('Ctrl Pts',(1.74251908492617,-1.,3.69677856910517));
#30975=CARTESIAN_POINT('Ctrl Pts',(1.73676193254557,-1.,3.69163322648036));
#30976=CARTESIAN_POINT('Ctrl Pts',(1.73103640956717,-1.,3.68646597019332));
#30977=CARTESIAN_POINT('Ctrl Pts',(1.72534302437056,-1.,3.68127704936579));
#30978=CARTESIAN_POINT('Ctrl Pts',(1.71968225581808,-1.,3.67606660374709));
#30979=CARTESIAN_POINT('Ctrl Pts',(1.71405450210383,-1.,3.67083454901611));
#30980=CARTESIAN_POINT('Ctrl Pts',(1.70846001610956,-1.,3.66558043198876));
#30981=CARTESIAN_POINT('Ctrl Pts',(1.70289888566873,-1.,3.66030338774847));
#30982=CARTESIAN_POINT('Ctrl Pts',(1.69737117722534,-1.,3.65500246526749));
#30983=CARTESIAN_POINT('Ctrl Pts',(1.69187705481689,-1.,3.64967689827371));
#30984=CARTESIAN_POINT('Ctrl Pts',(1.68641690471457,-1.,3.64432638915203));
#30985=CARTESIAN_POINT('Ctrl Pts',(1.68099146651586,-1.,3.63895140887462));
#30986=CARTESIAN_POINT('Ctrl Pts',(1.67560193613156,-1.,3.63355343201232));
#30987=CARTESIAN_POINT('Ctrl Pts',(1.67024966008044,-1.,3.62813422105271));
#30988=CARTESIAN_POINT('Ctrl Pts',(1.66493585923855,-1.,3.62269517989109));
#30989=CARTESIAN_POINT('Ctrl Pts',(1.65966133399186,-1.,3.61723666482456));
#30990=CARTESIAN_POINT('Ctrl Pts',(1.65442619244325,-1.,3.61175734965127));
#30991=CARTESIAN_POINT('Ctrl Pts',(1.64922952425832,-1.,3.60625346556992));
#30992=CARTESIAN_POINT('Ctrl Pts',(1.64407004385582,-1.,3.60072028513845));
#30993=CARTESIAN_POINT('Ctrl Pts',(1.63894676675352,-1.,3.59515368334893));
#30994=CARTESIAN_POINT('Ctrl Pts',(1.6338597145126,-1.,3.58955176627879));
#30995=CARTESIAN_POINT('Ctrl Pts',(1.62881051550745,-1.,3.58391625774343));
#30996=CARTESIAN_POINT('Ctrl Pts',(1.62380329464844,-1.,3.5782545595439));
#30997=CARTESIAN_POINT('Ctrl Pts',(1.61884340915404,-1.,3.57257679609806));
#30998=CARTESIAN_POINT('Ctrl Pts',(1.61393581747514,-1.,3.56689200468387));
#30999=CARTESIAN_POINT('Ctrl Pts',(1.60908344685457,-1.,3.5612043248298));
#31000=CARTESIAN_POINT('Ctrl Pts',(1.60428584699853,-1.,3.55550985096129));
#31001=CARTESIAN_POINT('Ctrl Pts',(1.59953698113457,-1.,3.54979148634454));
#31002=CARTESIAN_POINT('Ctrl Pts',(1.59482766949766,-1.,3.54402458182337));
#31003=CARTESIAN_POINT('Ctrl Pts',(1.59014958368739,-1.,3.53818616861077));
#31004=CARTESIAN_POINT('Ctrl Pts',(1.58549906268088,-1.,3.5322637814708));
#31005=CARTESIAN_POINT('Ctrl Pts',(1.58088027227848,-1.,3.52626275334881));
#31006=CARTESIAN_POINT('Ctrl Pts',(1.57631049988158,-1.,3.52021847865912));
#31007=CARTESIAN_POINT('Ctrl Pts',(1.57181569799743,-1.,3.51418598431665));
#31008=CARTESIAN_POINT('Ctrl Pts',(1.56742097575012,-1.,3.50821771695363));
#31009=CARTESIAN_POINT('Ctrl Pts',(1.56314187758675,-1.,3.50234321621578));
#31010=CARTESIAN_POINT('Ctrl Pts',(1.55897703097874,-1.,3.49655185179655));
#31011=CARTESIAN_POINT('Ctrl Pts',(1.55489595901116,-1.,3.4907646087742));
#31012=CARTESIAN_POINT('Ctrl Pts',(1.55084702970452,-1.,3.48485155928567));
#31013=CARTESIAN_POINT('Ctrl Pts',(1.54678009290276,-1.,3.47868272898751));
#31014=CARTESIAN_POINT('Ctrl Pts',(1.54266605398187,-1.,3.47217189224653));
#31015=CARTESIAN_POINT('Ctrl Pts',(1.53851507915502,-1.,3.46531752207153));
#31016=CARTESIAN_POINT('Ctrl Pts',(1.53440195378792,-1.,3.45825932955032));
#31017=CARTESIAN_POINT('Ctrl Pts',(1.53046244461635,-1.,3.45127136828305));
#31018=CARTESIAN_POINT('Ctrl Pts',(1.52686242875556,-1.,3.44469547526647));
#31019=CARTESIAN_POINT('Ctrl Pts',(1.5237734895035,-1.,3.4388889597401));
#31020=CARTESIAN_POINT('Ctrl Pts',(1.52134826724292,-1.,3.43417156977893));
#31021=CARTESIAN_POINT('Ctrl Pts',(1.5198144909338,-1.,3.43101631893414));
#31022=CARTESIAN_POINT('Ctrl Pts',(1.51914806898491,-1.,3.42946838852587));
#31023=CARTESIAN_POINT('Ctrl Pts',(1.5189513329503,-1.,3.42884302333841));
#31024=CARTESIAN_POINT('Ctrl Pts',(1.51893924967331,-1.,3.42864616361875));
#31025=CARTESIAN_POINT('Ctrl Pts',(1.5189508286633,-1.,3.42859860294306));
#31026=CARTESIAN_POINT('',(1.35032489087269,-1.,3.49844575334386));
#31027=CARTESIAN_POINT('Origin',(0.,-1.,0.));
#31028=CARTESIAN_POINT('',(1.36999806084572,-1.,3.97027773754922));
#31029=CARTESIAN_POINT('Ctrl Pts',(1.35032489087269,-1.,3.49844575334386));
#31030=CARTESIAN_POINT('Ctrl Pts',(1.35036670893102,-1.,3.49847119623841));
#31031=CARTESIAN_POINT('Ctrl Pts',(1.35049736560633,-1.,3.49861894124915));
#31032=CARTESIAN_POINT('Ctrl Pts',(1.35080045218652,-1.,3.49920025459856));
#31033=CARTESIAN_POINT('Ctrl Pts',(1.35142377279535,-1.,3.5007660381658));
#31034=CARTESIAN_POINT('Ctrl Pts',(1.3525703284343,-1.,3.50408168106113));
#31035=CARTESIAN_POINT('Ctrl Pts',(1.35419113576022,-1.,3.50913227060177));
#31036=CARTESIAN_POINT('Ctrl Pts',(1.35611275237288,-1.,3.51542230699919));
#31037=CARTESIAN_POINT('Ctrl Pts',(1.35821701528975,-1.,3.52261776117121));
#31038=CARTESIAN_POINT('Ctrl Pts',(1.36037259643827,-1.,3.53034464961849));
#31039=CARTESIAN_POINT('Ctrl Pts',(1.36245507339334,-1.,3.53824396425032));
#31040=CARTESIAN_POINT('Ctrl Pts',(1.36436666257567,-1.,3.54602591832893));
#31041=CARTESIAN_POINT('Ctrl Pts',(1.36606145456711,-1.,3.55353883995793));
#31042=CARTESIAN_POINT('Ctrl Pts',(1.36754771771174,-1.,3.56077662028492));
#31043=CARTESIAN_POINT('Ctrl Pts',(1.36886584973349,-1.,3.56782080304554));
#31044=CARTESIAN_POINT('Ctrl Pts',(1.37007229485646,-1.,3.57479875549453));
#31045=CARTESIAN_POINT('Ctrl Pts',(1.37122241663073,-1.,3.58183885982745));
#31046=CARTESIAN_POINT('Ctrl Pts',(1.37235053661,-1.,3.5890185384643));
#31047=CARTESIAN_POINT('Ctrl Pts',(1.37346320103184,-1.,3.59634627869117));
#31048=CARTESIAN_POINT('Ctrl Pts',(1.37455051379642,-1.,3.60379020124038));
#31049=CARTESIAN_POINT('Ctrl Pts',(1.37559314436641,-1.,3.61129546591082));
#31050=CARTESIAN_POINT('Ctrl Pts',(1.37657053403102,-1.,3.61880481160408));
#31051=CARTESIAN_POINT('Ctrl Pts',(1.37746987919868,-1.,3.62628098665112));
#31052=CARTESIAN_POINT('Ctrl Pts',(1.37829035457324,-1.,3.63371727442448));
#31053=CARTESIAN_POINT('Ctrl Pts',(1.37903818567347,-1.,3.64112507791112));
#31054=CARTESIAN_POINT('Ctrl Pts',(1.37972372481598,-1.,3.64852652756444));
#31055=CARTESIAN_POINT('Ctrl Pts',(1.38035791051215,-1.,3.65594554404396));
#31056=CARTESIAN_POINT('Ctrl Pts',(1.38094856333558,-1.,3.66339848520874));
#31057=CARTESIAN_POINT('Ctrl Pts',(1.38149812653876,-1.,3.67088843112282));
#31058=CARTESIAN_POINT('Ctrl Pts',(1.38200574290626,-1.,3.6784103848243));
#31059=CARTESIAN_POINT('Ctrl Pts',(1.38246852827185,-1.,3.68595444983844));
#31060=CARTESIAN_POINT('Ctrl Pts',(1.38288311171649,-1.,3.69350967899523));
#31061=CARTESIAN_POINT('Ctrl Pts',(1.38324717612862,-1.,3.70106792167894));
#31062=CARTESIAN_POINT('Ctrl Pts',(1.38356065402122,-1.,3.70862680753343));
#31063=CARTESIAN_POINT('Ctrl Pts',(1.38382489984585,-1.,3.7161876605181));
#31064=CARTESIAN_POINT('Ctrl Pts',(1.3840421342895,-1.,3.72375409358805));
#31065=CARTESIAN_POINT('Ctrl Pts',(1.38421479111531,-1.,3.73133035859283));
#31066=CARTESIAN_POINT('Ctrl Pts',(1.38434489156456,-1.,3.73891976418099));
#31067=CARTESIAN_POINT('Ctrl Pts',(1.38443344984389,-1.,3.7465231716786));
#31068=CARTESIAN_POINT('Ctrl Pts',(1.38448077997155,-1.,3.75413976318727));
#31069=CARTESIAN_POINT('Ctrl Pts',(1.38448675253343,-1.,3.76176768271347));
#31070=CARTESIAN_POINT('Ctrl Pts',(1.38445107339517,-1.,3.76940473185775));
#31071=CARTESIAN_POINT('Ctrl Pts',(1.38437354551435,-1.,3.77704902230441));
#31072=CARTESIAN_POINT('Ctrl Pts',(1.38425435883773,-1.,3.78469969805134));
#31073=CARTESIAN_POINT('Ctrl Pts',(1.38409399694588,-1.,3.79235669640907));
#31074=CARTESIAN_POINT('Ctrl Pts',(1.38389311766701,-1.,3.80002044322169));
#31075=CARTESIAN_POINT('Ctrl Pts',(1.38365244046226,-1.,3.80769156398429));
#31076=CARTESIAN_POINT('Ctrl Pts',(1.38337263902766,-1.,3.81537060817765));
#31077=CARTESIAN_POINT('Ctrl Pts',(1.38305421262724,-1.,3.82305771743715));
#31078=CARTESIAN_POINT('Ctrl Pts',(1.38269750245086,-1.,3.83075266982138));
#31079=CARTESIAN_POINT('Ctrl Pts',(1.38230274828774,-1.,3.83845502790609));
#31080=CARTESIAN_POINT('Ctrl Pts',(1.38187013346089,-1.,3.84616425605705));
#31081=CARTESIAN_POINT('Ctrl Pts',(1.38139983115075,-1.,3.85387983979557));
#31082=CARTESIAN_POINT('Ctrl Pts',(1.38089205993067,-1.,3.86160143044187));
#31083=CARTESIAN_POINT('Ctrl Pts',(1.38034709213129,-1.,3.86932885813403));
#31084=CARTESIAN_POINT('Ctrl Pts',(1.37976523097187,-1.,3.87706205830865));
#31085=CARTESIAN_POINT('Ctrl Pts',(1.37914679719446,-1.,3.88480102249461));
#31086=CARTESIAN_POINT('Ctrl Pts',(1.37849211287981,-1.,3.89254574338385));
#31087=CARTESIAN_POINT('Ctrl Pts',(1.3778014851263,-1.,3.90029615196255));
#31088=CARTESIAN_POINT('Ctrl Pts',(1.3770751963376,-1.,3.90805209522729));
#31089=CARTESIAN_POINT('Ctrl Pts',(1.37631350505516,-1.,3.91581337461825));
#31090=CARTESIAN_POINT('Ctrl Pts',(1.37551664448057,-1.,3.92357976987132));
#31091=CARTESIAN_POINT('Ctrl Pts',(1.37468482215784,-1.,3.93135106761941));
#31092=CARTESIAN_POINT('Ctrl Pts',(1.37381821967499,-1.,3.93912709041791));
#31093=CARTESIAN_POINT('Ctrl Pts',(1.37291699203423,-1.,3.94690771786926));
#31094=CARTESIAN_POINT('Ctrl Pts',(1.37198126433139,-1.,3.95469287283105));
#31095=CARTESIAN_POINT('Ctrl Pts',(1.37120515615663,-1.,3.96092458508407));
#31096=CARTESIAN_POINT('Ctrl Pts',(1.37060761746027,-1.,3.96560037975788));
#31097=CARTESIAN_POINT('Ctrl Pts',(1.37020239094758,-1.,3.9687184694173));
#31098=CARTESIAN_POINT('Ctrl Pts',(1.36999806084572,-1.,3.97027773754922));
#31099=CARTESIAN_POINT('',(1.22531898815164,-1.,4.01728681790024));
#31100=CARTESIAN_POINT('',(1.36999806084572,-1.,3.97027773754922));
#31101=CARTESIAN_POINT('',(0.963899035118985,-1.,3.62400312501199));
#31102=CARTESIAN_POINT('Ctrl Pts',(1.22531898815164,-1.,4.01728681790024));
#31103=CARTESIAN_POINT('Ctrl Pts',(1.22423716681317,-1.,4.01614544569895));
#31104=CARTESIAN_POINT('Ctrl Pts',(1.22207656455845,-1.,4.01386104433519));
#31105=CARTESIAN_POINT('Ctrl Pts',(1.21884478244403,-1.,4.01042947140789));
#31106=CARTESIAN_POINT('Ctrl Pts',(1.21455398918133,-1.,4.00584409522722));
#31107=CARTESIAN_POINT('Ctrl Pts',(1.20922097029551,-1.,4.00009577950721));
#31108=CARTESIAN_POINT('Ctrl Pts',(1.20391852375138,-1.,3.99433084799666));
#31109=CARTESIAN_POINT('Ctrl Pts',(1.19864679609566,-1.,3.98854928957189));
#31110=CARTESIAN_POINT('Ctrl Pts',(1.19340598349475,-1.,3.98275111052561));
#31111=CARTESIAN_POINT('Ctrl Pts',(1.18819633715539,-1.,3.97693634767754));
#31112=CARTESIAN_POINT('Ctrl Pts',(1.18301815039831,-1.,3.97110505165415));
#31113=CARTESIAN_POINT('Ctrl Pts',(1.17787174135592,-1.,3.96525726358159));
#31114=CARTESIAN_POINT('Ctrl Pts',(1.17275743590361,-1.,3.95939299213276));
#31115=CARTESIAN_POINT('Ctrl Pts',(1.16767555244438,-1.,3.95351219509876));
#31116=CARTESIAN_POINT('Ctrl Pts',(1.16262637999157,-1.,3.94761474780583));
#31117=CARTESIAN_POINT('Ctrl Pts',(1.15761018340956,-1.,3.94170046685203));
#31118=CARTESIAN_POINT('Ctrl Pts',(1.1526272271632,-1.,3.9357691705628));
#31119=CARTESIAN_POINT('Ctrl Pts',(1.14767779451123,-1.,3.92982073294257));
#31120=CARTESIAN_POINT('Ctrl Pts',(1.14276220561593,-1.,3.92385513133997));
#31121=CARTESIAN_POINT('Ctrl Pts',(1.13788084225554,-1.,3.91787251936827));
#31122=CARTESIAN_POINT('Ctrl Pts',(1.13303414693896,-1.,3.91187321145649));
#31123=CARTESIAN_POINT('Ctrl Pts',(1.12822258281553,-1.,3.90585753318737));
#31124=CARTESIAN_POINT('Ctrl Pts',(1.12344660099043,-1.,3.89982569750025));
#31125=CARTESIAN_POINT('Ctrl Pts',(1.11870660794603,-1.,3.89377768340344));
#31126=CARTESIAN_POINT('Ctrl Pts',(1.11400292434429,-1.,3.88771308285171));
#31127=CARTESIAN_POINT('Ctrl Pts',(1.10933577224008,-1.,3.88163105531724));
#31128=CARTESIAN_POINT('Ctrl Pts',(1.10470536603287,-1.,3.87553067187514));
#31129=CARTESIAN_POINT('Ctrl Pts',(1.10011198761195,-1.,3.86941120134849));
#31130=CARTESIAN_POINT('Ctrl Pts',(1.09555606505013,-1.,3.86327241021247));
#31131=CARTESIAN_POINT('Ctrl Pts',(1.09103825516294,-1.,3.85711487933931));
#31132=CARTESIAN_POINT('Ctrl Pts',(1.08655950846384,-1.,3.85094025222713));
#31133=CARTESIAN_POINT('Ctrl Pts',(1.08212087917991,-1.,3.8447504803063));
#31134=CARTESIAN_POINT('Ctrl Pts',(1.07772335353858,-1.,3.83854714117491));
#31135=CARTESIAN_POINT('Ctrl Pts',(1.07336766633459,-1.,3.83233071195144));
#31136=CARTESIAN_POINT('Ctrl Pts',(1.06905413180359,-1.,3.82609989967276));
#31137=CARTESIAN_POINT('Ctrl Pts',(1.0647824403893,-1.,3.81985083953012));
#31138=CARTESIAN_POINT('Ctrl Pts',(1.06055206187299,-1.,3.8135786611749));
#31139=CARTESIAN_POINT('Ctrl Pts',(1.05636266918644,-1.,3.80727913637791));
#31140=CARTESIAN_POINT('Ctrl Pts',(1.05221457990016,-1.,3.80095039790681));
#31141=CARTESIAN_POINT('Ctrl Pts',(1.04810913267639,-1.,3.79459440308786));
#31142=CARTESIAN_POINT('Ctrl Pts',(1.04404924374422,-1.,3.78821910787179));
#31143=CARTESIAN_POINT('Ctrl Pts',(1.04003862055798,-1.,3.7818353500817));
#31144=CARTESIAN_POINT('Ctrl Pts',(1.03608074678008,-1.,3.77545283140427));
#31145=CARTESIAN_POINT('Ctrl Pts',(1.03217786604919,-1.,3.76907609832516));
#31146=CARTESIAN_POINT('Ctrl Pts',(1.02833014458184,-1.,3.76270122291245));
#31147=CARTESIAN_POINT('Ctrl Pts',(1.02453429444668,-1.,3.75631037456224));
#31148=CARTESIAN_POINT('Ctrl Pts',(1.02078510487439,-1.,3.74987777155873));
#31149=CARTESIAN_POINT('Ctrl Pts',(1.01707794311088,-1.,3.74337942504993));
#31150=CARTESIAN_POINT('Ctrl Pts',(1.01341114319906,-1.,3.73680245055747));
#31151=CARTESIAN_POINT('Ctrl Pts',(1.00978798539491,-1.,3.73015276704407));
#31152=CARTESIAN_POINT('Ctrl Pts',(1.00622000735696,-1.,3.72346803750544));
#31153=CARTESIAN_POINT('Ctrl Pts',(1.00272423396802,-1.,3.71680667125047));
#31154=CARTESIAN_POINT('Ctrl Pts',(0.999317260756344,-1.,3.7102243971387));
#31155=CARTESIAN_POINT('Ctrl Pts',(0.996009819772431,-1.,3.70375282282107));
#31156=CARTESIAN_POINT('Ctrl Pts',(0.992802218332103,-1.,3.69738123415696));
#31157=CARTESIAN_POINT('Ctrl Pts',(0.989676715398858,-1.,3.69102682138955));
#31158=CARTESIAN_POINT('Ctrl Pts',(0.986602639864285,-1.,3.6845531792623));
#31159=CARTESIAN_POINT('Ctrl Pts',(0.983550791470864,-1.,3.67782408841876));
#31160=CARTESIAN_POINT('Ctrl Pts',(0.980505922458494,-1.,3.67074983340444));
#31161=CARTESIAN_POINT('Ctrl Pts',(0.977478312751416,-1.,3.66333049637403));
#31162=CARTESIAN_POINT('Ctrl Pts',(0.974519971354138,-1.,3.6557157673487));
#31163=CARTESIAN_POINT('Ctrl Pts',(0.971722122060277,-1.,3.64819756447072));
#31164=CARTESIAN_POINT('Ctrl Pts',(0.969195124674828,-1.,3.64113946505393));
#31165=CARTESIAN_POINT('Ctrl Pts',(0.967052554540877,-1.,3.6349212208096));
#31166=CARTESIAN_POINT('Ctrl Pts',(0.965395153165715,-1.,3.62988252139998));
#31167=CARTESIAN_POINT('Ctrl Pts',(0.964373850166081,-1.,3.62652618145252));
#31168=CARTESIAN_POINT('Ctrl Pts',(0.963957782642589,-1.,3.62489305727516));
#31169=CARTESIAN_POINT('Ctrl Pts',(0.963861297423578,-1.,3.62424461507455));
#31170=CARTESIAN_POINT('Ctrl Pts',(0.963880158556713,-1.,3.62404828878374));
#31171=CARTESIAN_POINT('Ctrl Pts',(0.963899035118985,-1.,3.62400312501199));
#31172=CARTESIAN_POINT('',(0.786422660833742,-1.,3.66661143271648));
#31173=CARTESIAN_POINT('Origin',(0.,-1.,0.));
#31174=CARTESIAN_POINT('',(0.732042837400619,-1.,4.13571194405636));
#31175=CARTESIAN_POINT('Ctrl Pts',(0.786422660833742,-1.,3.66661143271648));
#31176=CARTESIAN_POINT('Ctrl Pts',(0.786459983896781,-1.,3.66664310415236));
#31177=CARTESIAN_POINT('Ctrl Pts',(0.786565919559889,-1.,3.66680946938396));
#31178=CARTESIAN_POINT('Ctrl Pts',(0.786774337198499,-1.,3.66743103898844));
#31179=CARTESIAN_POINT('Ctrl Pts',(0.787145041181588,-1.,3.66907505398769));
#31180=CARTESIAN_POINT('Ctrl Pts',(0.787758799995426,-1.,3.672529236635));
#31181=CARTESIAN_POINT('Ctrl Pts',(0.788569566220662,-1.,3.67777119516438));
#31182=CARTESIAN_POINT('Ctrl Pts',(0.789483546065158,-1.,3.68428439784285));
#31183=CARTESIAN_POINT('Ctrl Pts',(0.790436284989579,-1.,3.69172044327754));
#31184=CARTESIAN_POINT('Ctrl Pts',(0.791356575696508,-1.,3.69968940808982));
#31185=CARTESIAN_POINT('Ctrl Pts',(0.792177688845967,-1.,3.70781724021879));
#31186=CARTESIAN_POINT('Ctrl Pts',(0.792848377370115,-1.,3.7158024239604));
#31187=CARTESIAN_POINT('Ctrl Pts',(0.79334702378387,-1.,3.7234879729357));
#31188=CARTESIAN_POINT('Ctrl Pts',(0.793682750269347,-1.,3.7308691469564));
#31189=CARTESIAN_POINT('Ctrl Pts',(0.79388270093679,-1.,3.73803280541576));
#31190=CARTESIAN_POINT('Ctrl Pts',(0.79398270045988,-1.,3.74511357728827));
#31191=CARTESIAN_POINT('Ctrl Pts',(0.79401734737144,-1.,3.75224692493895));
#31192=CARTESIAN_POINT('Ctrl Pts',(0.794008429135046,-1.,3.75951468666325));
#31193=CARTESIAN_POINT('Ctrl Pts',(0.793961083689141,-1.,3.76692626931184));
#31194=CARTESIAN_POINT('Ctrl Pts',(0.793870523787515,-1.,3.77444863801264));
#31195=CARTESIAN_POINT('Ctrl Pts',(0.793726235781339,-1.,3.78202460377617));
#31196=CARTESIAN_POINT('Ctrl Pts',(0.793516871680965,-1.,3.78959439439222));
#31197=CARTESIAN_POINT('Ctrl Pts',(0.7932356129732,-1.,3.79711921389862));
#31198=CARTESIAN_POINT('Ctrl Pts',(0.792882695234692,-1.,3.80459229925598));
#31199=CARTESIAN_POINT('Ctrl Pts',(0.792462483517568,-1.,3.81202588694726));
#31200=CARTESIAN_POINT('Ctrl Pts',(0.791981740718606,-1.,3.81944345442237));
#31201=CARTESIAN_POINT('Ctrl Pts',(0.791447528662381,-1.,3.82687033899799));
#31202=CARTESIAN_POINT('Ctrl Pts',(0.790865012705339,-1.,3.83432392054804));
#31203=CARTESIAN_POINT('Ctrl Pts',(0.790236124191289,-1.,3.84180762342476));
#31204=CARTESIAN_POINT('Ctrl Pts',(0.789560798155618,-1.,3.8493163780891));
#31205=CARTESIAN_POINT('Ctrl Pts',(0.788837734090688,-1.,3.85683995872536));
#31206=CARTESIAN_POINT('Ctrl Pts',(0.78806531509377,-1.,3.86436702561342));
#31207=CARTESIAN_POINT('Ctrl Pts',(0.78724252761798,-1.,3.87188916600905));
#31208=CARTESIAN_POINT('Ctrl Pts',(0.786369675812591,-1.,3.87940402818186));
#31209=CARTESIAN_POINT('Ctrl Pts',(0.785447890340723,-1.,3.88691313167399));
#31210=CARTESIAN_POINT('Ctrl Pts',(0.784478799358335,-1.,3.89442039235105));
#31211=CARTESIAN_POINT('Ctrl Pts',(0.783464141529082,-1.,3.90193039043971));
#31212=CARTESIAN_POINT('Ctrl Pts',(0.782405395622758,-1.,3.90944671004536));
#31213=CARTESIAN_POINT('Ctrl Pts',(0.781303428618343,-1.,3.9169703605466));
#31214=CARTESIAN_POINT('Ctrl Pts',(0.780158678615506,-1.,3.92450058323799));
#31215=CARTESIAN_POINT('Ctrl Pts',(0.778971308134786,-1.,3.93203552473153));
#31216=CARTESIAN_POINT('Ctrl Pts',(0.777741370568549,-1.,3.93957296768098));
#31217=CARTESIAN_POINT('Ctrl Pts',(0.776468966697959,-1.,3.94711101619471));
#31218=CARTESIAN_POINT('Ctrl Pts',(0.775154418039441,-1.,3.95464885452364));
#31219=CARTESIAN_POINT('Ctrl Pts',(0.773798212026682,-1.,3.96218649639876));
#31220=CARTESIAN_POINT('Ctrl Pts',(0.772400931772238,-1.,3.96972446532832));
#31221=CARTESIAN_POINT('Ctrl Pts',(0.770963190030503,-1.,3.97726349165507));
#31222=CARTESIAN_POINT('Ctrl Pts',(0.769485566245459,-1.,3.98480422348403));
#31223=CARTESIAN_POINT('Ctrl Pts',(0.767968531377707,-1.,3.99234687880892));
#31224=CARTESIAN_POINT('Ctrl Pts',(0.766412457135785,-1.,3.99989129179464));
#31225=CARTESIAN_POINT('Ctrl Pts',(0.764817648784946,-1.,4.00743706791366));
#31226=CARTESIAN_POINT('Ctrl Pts',(0.763184371182826,-1.,4.01498370680434));
#31227=CARTESIAN_POINT('Ctrl Pts',(0.761512875859941,-1.,4.02253072741347));
#31228=CARTESIAN_POINT('Ctrl Pts',(0.759803433244165,-1.,4.0300778195465));
#31229=CARTESIAN_POINT('Ctrl Pts',(0.758056338885553,-1.,4.03762485803468));
#31230=CARTESIAN_POINT('Ctrl Pts',(0.756271902370186,-1.,4.04517182654344));
#31231=CARTESIAN_POINT('Ctrl Pts',(0.754450441816411,-1.,4.05271876688106));
#31232=CARTESIAN_POINT('Ctrl Pts',(0.752592276482868,-1.,4.06026572221399));
#31233=CARTESIAN_POINT('Ctrl Pts',(0.750697720483175,-1.,4.06781267241886));
#31234=CARTESIAN_POINT('Ctrl Pts',(0.748767076679176,-1.,4.07535951055363));
#31235=CARTESIAN_POINT('Ctrl Pts',(0.746800631490821,-1.,4.08290608094789));
#31236=CARTESIAN_POINT('Ctrl Pts',(0.744798649705513,-1.,4.09045220253011));
#31237=CARTESIAN_POINT('Ctrl Pts',(0.742761369690017,-1.,4.09799769702712));
#31238=CARTESIAN_POINT('Ctrl Pts',(0.740688998555151,-1.,4.1055424175856));
#31239=CARTESIAN_POINT('Ctrl Pts',(0.738581708229118,-1.,4.11308626953795));
#31240=CARTESIAN_POINT('Ctrl Pts',(0.736439634335347,-1.,4.12062919626082));
#31241=CARTESIAN_POINT('Ctrl Pts',(0.734698226767512,-1.,4.12666277572794));
#31242=CARTESIAN_POINT('Ctrl Pts',(0.733376589325634,-1.,4.13118752796397));
#31243=CARTESIAN_POINT('Ctrl Pts',(0.732488575135925,-1.,4.13420383737278));
#31244=CARTESIAN_POINT('Ctrl Pts',(0.732042837400619,-1.,4.13571194405636));
#31245=CARTESIAN_POINT('',(0.581791163835814,-1.,4.15950947128175));
#31246=CARTESIAN_POINT('',(0.732042837400619,-1.,4.13571194405636));
#31247=CARTESIAN_POINT('',(0.385112848332549,-1.,3.73017266276632));
#31248=CARTESIAN_POINT('Ctrl Pts',(0.581791163835814,-1.,4.15950947128175));
#31249=CARTESIAN_POINT('Ctrl Pts',(0.580901211462913,-1.,4.15821291712391));
#31250=CARTESIAN_POINT('Ctrl Pts',(0.579124568912543,-1.,4.15561864787379));
#31251=CARTESIAN_POINT('Ctrl Pts',(0.576469391673916,-1.,4.1517237611974));
#31252=CARTESIAN_POINT('Ctrl Pts',(0.572948736066276,-1.,4.14652361065787));
#31253=CARTESIAN_POINT('Ctrl Pts',(0.568580610187115,-1.,4.14001179828669));
#31254=CARTESIAN_POINT('Ctrl Pts',(0.564245279535705,-1.,4.13348835726086));
#31255=CARTESIAN_POINT('Ctrl Pts',(0.559942890594628,-1.,4.12695329951859));
#31256=CARTESIAN_POINT('Ctrl Pts',(0.555673636130778,-1.,4.1204066619623));
#31257=CARTESIAN_POINT('Ctrl Pts',(0.551437758498246,-1.,4.11384852025578));
#31258=CARTESIAN_POINT('Ctrl Pts',(0.547235539486759,-1.,4.1072789702877));
#31259=CARTESIAN_POINT('Ctrl Pts',(0.543067286878457,-1.,4.10069810244473));
#31260=CARTESIAN_POINT('Ctrl Pts',(0.53893332117992,-1.,4.09410597627116));
#31261=CARTESIAN_POINT('Ctrl Pts',(0.534833963476999,-1.,4.08750259988693));
#31262=CARTESIAN_POINT('Ctrl Pts',(0.530769518728075,-1.,4.08088789536488));
#31263=CARTESIAN_POINT('Ctrl Pts',(0.526740277226999,-1.,4.07426172299496));
#31264=CARTESIAN_POINT('Ctrl Pts',(0.522746528602767,-1.,4.06762394471075));
#31265=CARTESIAN_POINT('Ctrl Pts',(0.518788572336809,-1.,4.06097448037934));
#31266=CARTESIAN_POINT('Ctrl Pts',(0.514866728193103,-1.,4.05431335771261));
#31267=CARTESIAN_POINT('Ctrl Pts',(0.510981349219173,-1.,4.04764078815591));
#31268=CARTESIAN_POINT('Ctrl Pts',(0.507132823288361,-1.,4.04095715149074));
#31269=CARTESIAN_POINT('Ctrl Pts',(0.503321556915513,-1.,4.0342628417439));
#31270=CARTESIAN_POINT('Ctrl Pts',(0.499547962340889,-1.,4.0275581398015));
#31271=CARTESIAN_POINT('Ctrl Pts',(0.495812444326222,-1.,4.02084308851813));
#31272=CARTESIAN_POINT('Ctrl Pts',(0.49211538341793,-1.,4.01411733503486));
#31273=CARTESIAN_POINT('Ctrl Pts',(0.48845713042453,-1.,4.0073800839092));
#31274=CARTESIAN_POINT('Ctrl Pts',(0.484838042421754,-1.,4.00063045119234));
#31275=CARTESIAN_POINT('Ctrl Pts',(0.481258512209637,-1.,3.99386775880655));
#31276=CARTESIAN_POINT('Ctrl Pts',(0.477718999122033,-1.,3.98709184306743));
#31277=CARTESIAN_POINT('Ctrl Pts',(0.474220061019542,-1.,3.9803033804443));
#31278=CARTESIAN_POINT('Ctrl Pts',(0.470762379613477,-1.,3.97350414289415));
#31279=CARTESIAN_POINT('Ctrl Pts',(0.467346690880671,-1.,3.96669622273946));
#31280=CARTESIAN_POINT('Ctrl Pts',(0.463973722115744,-1.,3.95988133243543));
#31281=CARTESIAN_POINT('Ctrl Pts',(0.460644124429119,-1.,3.95306005817363));
#31282=CARTESIAN_POINT('Ctrl Pts',(0.457358410451673,-1.,3.94623117206675));
#31283=CARTESIAN_POINT('Ctrl Pts',(0.454116879027575,-1.,3.93939080846298));
#31284=CARTESIAN_POINT('Ctrl Pts',(0.450919768356346,-1.,3.93253407403128));
#31285=CARTESIAN_POINT('Ctrl Pts',(0.447767416837296,-1.,3.92565674143424));
#31286=CARTESIAN_POINT('Ctrl Pts',(0.444660430230592,-1.,3.91875701610721));
#31287=CARTESIAN_POINT('Ctrl Pts',(0.441599824524047,-1.,3.91183704069146));
#31288=CARTESIAN_POINT('Ctrl Pts',(0.438587235458233,-1.,3.90490512938546));
#31289=CARTESIAN_POINT('Ctrl Pts',(0.435624629433505,-1.,3.8979725665544));
#31290=CARTESIAN_POINT('Ctrl Pts',(0.432713929544439,-1.,3.89104947940592));
#31291=CARTESIAN_POINT('Ctrl Pts',(0.429856640579733,-1.,3.88414070943334));
#31292=CARTESIAN_POINT('Ctrl Pts',(0.427053541173469,-1.,3.87724240306609));
#31293=CARTESIAN_POINT('Ctrl Pts',(0.424304173195142,-1.,3.87033643487882));
#31294=CARTESIAN_POINT('Ctrl Pts',(0.421607423177575,-1.,3.86339652542749));
#31295=CARTESIAN_POINT('Ctrl Pts',(0.418962468086809,-1.,3.85639825648031));
#31296=CARTESIAN_POINT('Ctrl Pts',(0.41636967805292,-1.,3.8493286415751));
#31297=CARTESIAN_POINT('Ctrl Pts',(0.413831367016726,-1.,3.84219403994742));
#31298=CARTESIAN_POINT('Ctrl Pts',(0.411353038798459,-1.,3.83503345578645));
#31299=CARTESIAN_POINT('Ctrl Pts',(0.408942371447376,-1.,3.82790724256397));
#31300=CARTESIAN_POINT('Ctrl Pts',(0.406607038258906,-1.,3.82087303913741));
#31301=CARTESIAN_POINT('Ctrl Pts',(0.404352694628236,-1.,3.81396374287762));
#31302=CARTESIAN_POINT('Ctrl Pts',(0.402181320148474,-1.,3.80716881962763));
#31303=CARTESIAN_POINT('Ctrl Pts',(0.400088346504726,-1.,3.80040370384659));
#31304=CARTESIAN_POINT('Ctrl Pts',(0.398064818684158,-1.,3.79352887163457));
#31305=CARTESIAN_POINT('Ctrl Pts',(0.396103205335028,-1.,3.78640521279479));
#31306=CARTESIAN_POINT('Ctrl Pts',(0.394202481011595,-1.,3.77894173114368));
#31307=CARTESIAN_POINT('Ctrl Pts',(0.392372786223346,-1.,3.77114011595892));
#31308=CARTESIAN_POINT('Ctrl Pts',(0.390642072979258,-1.,3.76315635032993));
#31309=CARTESIAN_POINT('Ctrl Pts',(0.38905477589825,-1.,3.75529302894757));
#31310=CARTESIAN_POINT('Ctrl Pts',(0.387663020050396,-1.,3.74792651696269));
#31311=CARTESIAN_POINT('Ctrl Pts',(0.386519576222035,-1.,3.74144965781088));
#31312=CARTESIAN_POINT('Ctrl Pts',(0.385670806454744,-1.,3.73621371845475));
#31313=CARTESIAN_POINT('Ctrl Pts',(0.385187124633964,-1.,3.73273893363318));
#31314=CARTESIAN_POINT('Ctrl Pts',(0.385031656499141,-1.,3.73106082862399));
#31315=CARTESIAN_POINT('Ctrl Pts',(0.385037797882046,-1.,3.73040527620929));
#31316=CARTESIAN_POINT('Ctrl Pts',(0.385087139001608,-1.,3.73021431755218));
#31317=CARTESIAN_POINT('Ctrl Pts',(0.385112848332549,-1.,3.73017266276632));
#31318=CARTESIAN_POINT('',(0.203156094897895,-1.,3.74449296982994));
#31319=CARTESIAN_POINT('Origin',(0.,-1.,0.));
#31320=CARTESIAN_POINT('',(0.0760622897878233,-1.,4.19931119685982));
#31321=CARTESIAN_POINT('Ctrl Pts',(0.203156094897895,-1.,3.74449296982994));
#31322=CARTESIAN_POINT('Ctrl Pts',(0.203188003947964,-1.,3.74453008995129));
#31323=CARTESIAN_POINT('Ctrl Pts',(0.203266610111263,-1.,3.74471097893961));
#31324=CARTESIAN_POINT('Ctrl Pts',(0.203375226874331,-1.,3.74535749969262));
#31325=CARTESIAN_POINT('Ctrl Pts',(0.203484186269314,-1.,3.74703926501843));
#31326=CARTESIAN_POINT('Ctrl Pts',(0.203550035479096,-1.,3.75054693397716));
#31327=CARTESIAN_POINT('Ctrl Pts',(0.203530796848403,-1.,3.75585118707924));
#31328=CARTESIAN_POINT('Ctrl Pts',(0.203414634707646,-1.,3.76242717937273));
#31329=CARTESIAN_POINT('Ctrl Pts',(0.203192390045337,-1.,3.76992071595267));
#31330=CARTESIAN_POINT('Ctrl Pts',(0.202854729699196,-1.,3.77793553476879));
#31331=CARTESIAN_POINT('Ctrl Pts',(0.202394260512192,-1.,3.78609175019317));
#31332=CARTESIAN_POINT('Ctrl Pts',(0.201807533800798,-1.,3.79408354187274));
#31333=CARTESIAN_POINT('Ctrl Pts',(0.201097756307251,-1.,3.80175247447171));
#31334=CARTESIAN_POINT('Ctrl Pts',(0.200274679433289,-1.,3.80909529318501));
#31335=CARTESIAN_POINT('Ctrl Pts',(0.199351525297396,-1.,3.81620203429702));
#31336=CARTESIAN_POINT('Ctrl Pts',(0.198342616900469,-1.,3.82321127348981));
#31337=CARTESIAN_POINT('Ctrl Pts',(0.197260935827375,-1.,3.83026221776488));
#31338=CARTESIAN_POINT('Ctrl Pts',(0.196115198971889,-1.,3.83743910616265));
#31339=CARTESIAN_POINT('Ctrl Pts',(0.194909009460254,-1.,3.84475203347052));
#31340=CARTESIAN_POINT('Ctrl Pts',(0.193642806777747,-1.,3.85216762264019));
#31341=CARTESIAN_POINT('Ctrl Pts',(0.192315153044979,-1.,3.85962774407652));
#31342=CARTESIAN_POINT('Ctrl Pts',(0.190924190418612,-1.,3.8670715862477));
#31343=CARTESIAN_POINT('Ctrl Pts',(0.189469253358254,-1.,3.87445976418377));
#31344=CARTESIAN_POINT('Ctrl Pts',(0.187951632512663,-1.,3.88178563496187));
#31345=CARTESIAN_POINT('Ctrl Pts',(0.186373724985263,-1.,3.88906196725817));
#31346=CARTESIAN_POINT('Ctrl Pts',(0.184738537728034,-1.,3.89631300742633));
#31347=CARTESIAN_POINT('Ctrl Pts',(0.183049081993193,-1.,3.90356488555138));
#31348=CARTESIAN_POINT('Ctrl Pts',(0.181307740731795,-1.,3.91083557557193));
#31349=CARTESIAN_POINT('Ctrl Pts',(0.179515885822894,-1.,3.91812876180948));
#31350=CARTESIAN_POINT('Ctrl Pts',(0.177674246152328,-1.,3.92543942697672));
#31351=CARTESIAN_POINT('Ctrl Pts',(0.175783136893872,-1.,3.93275726771049));
#31352=CARTESIAN_POINT('Ctrl Pts',(0.173842734974607,-1.,3.94007083096214));
#31353=CARTESIAN_POINT('Ctrl Pts',(0.171853355369232,-1.,3.94737164900861));
#31354=CARTESIAN_POINT('Ctrl Pts',(0.16981566637413,-1.,3.95465744665263));
#31355=CARTESIAN_POINT('Ctrl Pts',(0.167730547023312,-1.,3.96192990160296));
#31356=CARTESIAN_POINT('Ctrl Pts',(0.165598992851097,-1.,3.9691931362141));
#31357=CARTESIAN_POINT('Ctrl Pts',(0.163422004609998,-1.,3.97645194630944));
#31358=CARTESIAN_POINT('Ctrl Pts',(0.161200482186087,-1.,3.98371010319866));
#31359=CARTESIAN_POINT('Ctrl Pts',(0.158935123982796,-1.,3.99096873945862));
#31360=CARTESIAN_POINT('Ctrl Pts',(0.156626481393735,-1.,3.99822717425869));
#31361=CARTESIAN_POINT('Ctrl Pts',(0.154275004872309,-1.,4.00548360245297));
#31362=CARTESIAN_POINT('Ctrl Pts',(0.151881094022909,-1.,4.01273584234684));
#31363=CARTESIAN_POINT('Ctrl Pts',(0.149445144968707,-1.,4.01998203715588));
#31364=CARTESIAN_POINT('Ctrl Pts',(0.146967602878998,-1.,4.02722143147048));
#31365=CARTESIAN_POINT('Ctrl Pts',(0.144448947038352,-1.,4.03445411510403));
#31366=CARTESIAN_POINT('Ctrl Pts',(0.141889671485507,-1.,4.04168069633842));
#31367=CARTESIAN_POINT('Ctrl Pts',(0.139290267180059,-1.,4.04890199238056));
#31368=CARTESIAN_POINT('Ctrl Pts',(0.136651205046111,-1.,4.05611873400122));
#31369=CARTESIAN_POINT('Ctrl Pts',(0.133972916144225,-1.,4.06333121018476));
#31370=CARTESIAN_POINT('Ctrl Pts',(0.131255793548914,-1.,4.07053931528579));
#31371=CARTESIAN_POINT('Ctrl Pts',(0.128500200484813,-1.,4.07774270738809));
#31372=CARTESIAN_POINT('Ctrl Pts',(0.125706476822529,-1.,4.08494093372315));
#31373=CARTESIAN_POINT('Ctrl Pts',(0.122874946249119,-1.,4.09213355850836));
#31374=CARTESIAN_POINT('Ctrl Pts',(0.120005924388162,-1.,4.09932031767243));
#31375=CARTESIAN_POINT('Ctrl Pts',(0.117099722731704,-1.,4.10650113382187));
#31376=CARTESIAN_POINT('Ctrl Pts',(0.114156649609601,-1.,4.11367603925313));
#31377=CARTESIAN_POINT('Ctrl Pts',(0.111177012683377,-1.,4.12084512502444));
#31378=CARTESIAN_POINT('Ctrl Pts',(0.10816112052835,-1.,4.12800848371386));
#31379=CARTESIAN_POINT('Ctrl Pts',(0.105109286538864,-1.,4.13516614458396));
#31380=CARTESIAN_POINT('Ctrl Pts',(0.102021826577453,-1.,4.14231804938737));
#31381=CARTESIAN_POINT('Ctrl Pts',(0.0988990478899809,-1.,4.1494640891762));
#31382=CARTESIAN_POINT('Ctrl Pts',(0.0957412403297065,-1.,4.15660412653006));
#31383=CARTESIAN_POINT('Ctrl Pts',(0.0925486672167687,-1.,4.16373802265942));
#31384=CARTESIAN_POINT('Ctrl Pts',(0.0893215560850325,-1.,4.17086566491823));
#31385=CARTESIAN_POINT('Ctrl Pts',(0.0860600915552512,-1.,4.17798698669991));
#31386=CARTESIAN_POINT('Ctrl Pts',(0.0827644164389507,-1.,4.1851019532944));
#31387=CARTESIAN_POINT('Ctrl Pts',(0.08010058871176,-1.,4.19078883322483));
#31388=CARTESIAN_POINT('Ctrl Pts',(0.0780873956244399,-1.,4.19505112860624));
#31389=CARTESIAN_POINT('Ctrl Pts',(0.0767384596142192,-1.,4.19789138621624));
#31390=CARTESIAN_POINT('Ctrl Pts',(0.0760622897878233,-1.,4.19931119685982));
#31391=CARTESIAN_POINT('',(-0.0760622897878249,-1.,4.19931119685982));
#31392=CARTESIAN_POINT('',(0.0760622897878233,-1.,4.19931119685982));
#31393=CARTESIAN_POINT('',(-0.203156094896101,-1.,3.74449296983004));
#31394=CARTESIAN_POINT('Ctrl Pts',(-0.0760622897878249,-1.,4.19931119685982));
#31395=CARTESIAN_POINT('Ctrl Pts',(-0.0767384596141467,-1.,4.1978913862118));
#31396=CARTESIAN_POINT('Ctrl Pts',(-0.07808739562424,-1.,4.19505112859416));
#31397=CARTESIAN_POINT('Ctrl Pts',(-0.0801005887114322,-1.,4.19078883320504));
#31398=CARTESIAN_POINT('Ctrl Pts',(-0.0827644164385681,-1.,4.18510195327123));
#31399=CARTESIAN_POINT('Ctrl Pts',(-0.0860600915549399,-1.,4.17798698668094));
#31400=CARTESIAN_POINT('Ctrl Pts',(-0.0893215560848652,-1.,4.17086566490794));
#31401=CARTESIAN_POINT('Ctrl Pts',(-0.0925486672167534,-1.,4.16373802265839));
#31402=CARTESIAN_POINT('Ctrl Pts',(-0.0957412403298009,-1.,4.15660412653577));
#31403=CARTESIAN_POINT('Ctrl Pts',(-0.0988990478901228,-1.,4.14946408918485));
#31404=CARTESIAN_POINT('Ctrl Pts',(-0.102021826577584,-1.,4.14231804939538));
#31405=CARTESIAN_POINT('Ctrl Pts',(-0.105109286538945,-1.,4.13516614458895));
#31406=CARTESIAN_POINT('Ctrl Pts',(-0.10816112052837,-1.,4.12800848371504));
#31407=CARTESIAN_POINT('Ctrl Pts',(-0.111177012683347,-1.,4.1208451250225));
#31408=CARTESIAN_POINT('Ctrl Pts',(-0.114156649609546,-1.,4.11367603924961));
#31409=CARTESIAN_POINT('Ctrl Pts',(-0.117099722731648,-1.,4.10650113381833));
#31410=CARTESIAN_POINT('Ctrl Pts',(-0.120005924388124,-1.,4.09932031767002));
#31411=CARTESIAN_POINT('Ctrl Pts',(-0.122874946249107,-1.,4.09213355850756));
#31412=CARTESIAN_POINT('Ctrl Pts',(-0.12570647682254,-1.,4.08494093372377));
#31413=CARTESIAN_POINT('Ctrl Pts',(-0.128500200484838,-1.,4.07774270738954));
#31414=CARTESIAN_POINT('Ctrl Pts',(-0.131255793548941,-1.,4.0705393152874));
#31415=CARTESIAN_POINT('Ctrl Pts',(-0.133972916144245,-1.,4.06333121018596));
#31416=CARTESIAN_POINT('Ctrl Pts',(-0.136651205046119,-1.,4.05611873400172));
#31417=CARTESIAN_POINT('Ctrl Pts',(-0.139290267180057,-1.,4.04890199238036));
#31418=CARTESIAN_POINT('Ctrl Pts',(-0.1418896714855,-1.,4.04168069633781));
#31419=CARTESIAN_POINT('Ctrl Pts',(-0.144448947038345,-1.,4.03445411510333));
#31420=CARTESIAN_POINT('Ctrl Pts',(-0.146967602878994,-1.,4.02722143146994));
#31421=CARTESIAN_POINT('Ctrl Pts',(-0.149445144968707,-1.,4.01998203715564));
#31422=CARTESIAN_POINT('Ctrl Pts',(-0.151881094022911,-1.,4.01273584234689));
#31423=CARTESIAN_POINT('Ctrl Pts',(-0.154275004872311,-1.,4.00548360245319));
#31424=CARTESIAN_POINT('Ctrl Pts',(-0.156626481393734,-1.,3.99822717425893));
#31425=CARTESIAN_POINT('Ctrl Pts',(-0.158935123982793,-1.,3.99096873945878));
#31426=CARTESIAN_POINT('Ctrl Pts',(-0.161200482186085,-1.,3.98371010319872));
#31427=CARTESIAN_POINT('Ctrl Pts',(-0.163422004609999,-1.,3.97645194630943));
#31428=CARTESIAN_POINT('Ctrl Pts',(-0.165598992851102,-1.,3.96919313621407));
#31429=CARTESIAN_POINT('Ctrl Pts',(-0.16773054702332,-1.,3.96192990160296));
#31430=CARTESIAN_POINT('Ctrl Pts',(-0.169815666374139,-1.,3.95465744665268));
#31431=CARTESIAN_POINT('Ctrl Pts',(-0.17185335536924,-1.,3.94737164900868));
#31432=CARTESIAN_POINT('Ctrl Pts',(-0.17384273497461,-1.,3.94007083096217));
#31433=CARTESIAN_POINT('Ctrl Pts',(-0.175783136893868,-1.,3.93275726771042));
#31434=CARTESIAN_POINT('Ctrl Pts',(-0.177674246152318,-1.,3.92543942697655));
#31435=CARTESIAN_POINT('Ctrl Pts',(-0.179515885822882,-1.,3.91812876180926));
#31436=CARTESIAN_POINT('Ctrl Pts',(-0.181307740731786,-1.,3.91083557557175));
#31437=CARTESIAN_POINT('Ctrl Pts',(-0.183049081993191,-1.,3.90356488555132));
#31438=CARTESIAN_POINT('Ctrl Pts',(-0.184738537728043,-1.,3.89631300742646));
#31439=CARTESIAN_POINT('Ctrl Pts',(-0.186373724985281,-1.,3.88906196725848));
#31440=CARTESIAN_POINT('Ctrl Pts',(-0.187951632512685,-1.,3.88178563496228));
#31441=CARTESIAN_POINT('Ctrl Pts',(-0.189469253358273,-1.,3.87445976418412));
#31442=CARTESIAN_POINT('Ctrl Pts',(-0.19092419041862,-1.,3.86707158624783));
#31443=CARTESIAN_POINT('Ctrl Pts',(-0.192315153044971,-1.,3.85962774407633));
#31444=CARTESIAN_POINT('Ctrl Pts',(-0.193642806777723,-1.,3.85216762263966));
#31445=CARTESIAN_POINT('Ctrl Pts',(-0.194909009460221,-1.,3.84475203346977));
#31446=CARTESIAN_POINT('Ctrl Pts',(-0.196115198971859,-1.,3.83743910616195));
#31447=CARTESIAN_POINT('Ctrl Pts',(-0.197260935827362,-1.,3.83026221776456));
#31448=CARTESIAN_POINT('Ctrl Pts',(-0.198342616900487,-1.,3.82321127349016));
#31449=CARTESIAN_POINT('Ctrl Pts',(-0.199351525297447,-1.,3.81620203429815));
#31450=CARTESIAN_POINT('Ctrl Pts',(-0.200274679433365,-1.,3.80909529318669));
#31451=CARTESIAN_POINT('Ctrl Pts',(-0.201097756307326,-1.,3.80175247447337));
#31452=CARTESIAN_POINT('Ctrl Pts',(-0.201807533800837,-1.,3.7940835418736));
#31453=CARTESIAN_POINT('Ctrl Pts',(-0.20239426051216,-1.,3.78609175019242));
#31454=CARTESIAN_POINT('Ctrl Pts',(-0.202854729699081,-1.,3.77793553476614));
#31455=CARTESIAN_POINT('Ctrl Pts',(-0.203192390045165,-1.,3.7699207159487));
#31456=CARTESIAN_POINT('Ctrl Pts',(-0.203414634707479,-1.,3.76242717936885));
#31457=CARTESIAN_POINT('Ctrl Pts',(-0.203530796848322,-1.,3.75585118707734));
#31458=CARTESIAN_POINT('Ctrl Pts',(-0.203550035479166,-1.,3.75054693397875));
#31459=CARTESIAN_POINT('Ctrl Pts',(-0.203484186269415,-1.,3.74703926501752));
#31460=CARTESIAN_POINT('Ctrl Pts',(-0.203375226874122,-1.,3.74535749969115));
#31461=CARTESIAN_POINT('Ctrl Pts',(-0.203266610110531,-1.,3.74471097893845));
#31462=CARTESIAN_POINT('Ctrl Pts',(-0.203188003946657,-1.,3.74453008995092));
#31463=CARTESIAN_POINT('Ctrl Pts',(-0.203156094896101,-1.,3.74449296983004));
#31464=CARTESIAN_POINT('',(-0.385112848330762,-1.,3.73017266276651));
#31465=CARTESIAN_POINT('Origin',(0.,-1.,0.));
#31466=CARTESIAN_POINT('',(-0.581791163835815,-1.,4.15950947128175));
#31467=CARTESIAN_POINT('Ctrl Pts',(-0.385112848330762,-1.,3.73017266276651));
#31468=CARTESIAN_POINT('Ctrl Pts',(-0.385087139000375,-1.,3.73021431755274));
#31469=CARTESIAN_POINT('Ctrl Pts',(-0.385037797881504,-1.,3.73040527621055));
#31470=CARTESIAN_POINT('Ctrl Pts',(-0.385031656499164,-1.,3.73106082862548));
#31471=CARTESIAN_POINT('Ctrl Pts',(-0.385187124634206,-1.,3.73273893363406));
#31472=CARTESIAN_POINT('Ctrl Pts',(-0.385670806454566,-1.,3.73621371845318));
#31473=CARTESIAN_POINT('Ctrl Pts',(-0.386519576222251,-1.,3.74144965781276));
#31474=CARTESIAN_POINT('Ctrl Pts',(-0.387663020050836,-1.,3.74792651696654));
#31475=CARTESIAN_POINT('Ctrl Pts',(-0.389054775898702,-1.,3.75529302895152));
#31476=CARTESIAN_POINT('Ctrl Pts',(-0.39064207297956,-1.,3.76315635033257));
#31477=CARTESIAN_POINT('Ctrl Pts',(-0.392372786223433,-1.,3.77114011595967));
#31478=CARTESIAN_POINT('Ctrl Pts',(-0.394202481011499,-1.,3.77894173114283));
#31479=CARTESIAN_POINT('Ctrl Pts',(-0.396103205334841,-1.,3.78640521279313));
#31480=CARTESIAN_POINT('Ctrl Pts',(-0.39806481868397,-1.,3.7935288716329));
#31481=CARTESIAN_POINT('Ctrl Pts',(-0.4000883465046,-1.,3.80040370384546));
#31482=CARTESIAN_POINT('Ctrl Pts',(-0.402181320148436,-1.,3.80716881962728));
#31483=CARTESIAN_POINT('Ctrl Pts',(-0.404352694628273,-1.,3.81396374287793));
#31484=CARTESIAN_POINT('Ctrl Pts',(-0.406607038258985,-1.,3.8208730391381));
#31485=CARTESIAN_POINT('Ctrl Pts',(-0.40894237144746,-1.,3.82790724256471));
#31486=CARTESIAN_POINT('Ctrl Pts',(-0.411353038798519,-1.,3.83503345578698));
#31487=CARTESIAN_POINT('Ctrl Pts',(-0.413831367016748,-1.,3.84219403994762));
#31488=CARTESIAN_POINT('Ctrl Pts',(-0.416369678052907,-1.,3.84932864157497));
#31489=CARTESIAN_POINT('Ctrl Pts',(-0.418962468086773,-1.,3.85639825647996));
#31490=CARTESIAN_POINT('Ctrl Pts',(-0.421607423177534,-1.,3.86339652542709));
#31491=CARTESIAN_POINT('Ctrl Pts',(-0.424304173195111,-1.,3.87033643487851));
#31492=CARTESIAN_POINT('Ctrl Pts',(-0.427053541173457,-1.,3.87724240306597));
#31493=CARTESIAN_POINT('Ctrl Pts',(-0.429856640579741,-1.,3.88414070943341));
#31494=CARTESIAN_POINT('Ctrl Pts',(-0.432713929544458,-1.,3.89104947940611));
#31495=CARTESIAN_POINT('Ctrl Pts',(-0.435624629433528,-1.,3.89797256655462));
#31496=CARTESIAN_POINT('Ctrl Pts',(-0.43858723545825,-1.,3.90490512938563));
#31497=CARTESIAN_POINT('Ctrl Pts',(-0.441599824524054,-1.,3.91183704069153));
#31498=CARTESIAN_POINT('Ctrl Pts',(-0.444660430230591,-1.,3.91875701610719));
#31499=CARTESIAN_POINT('Ctrl Pts',(-0.447767416837293,-1.,3.92565674143416));
#31500=CARTESIAN_POINT('Ctrl Pts',(-0.450919768356348,-1.,3.93253407403123));
#31501=CARTESIAN_POINT('Ctrl Pts',(-0.454116879027584,-1.,3.93939080846298));
#31502=CARTESIAN_POINT('Ctrl Pts',(-0.457358410451683,-1.,3.94623117206678));
#31503=CARTESIAN_POINT('Ctrl Pts',(-0.460644124429121,-1.,3.95306005817364));
#31504=CARTESIAN_POINT('Ctrl Pts',(-0.463973722115733,-1.,3.95988133243538));
#31505=CARTESIAN_POINT('Ctrl Pts',(-0.467346690880643,-1.,3.9666962227393));
#31506=CARTESIAN_POINT('Ctrl Pts',(-0.470762379613439,-1.,3.97350414289392));
#31507=CARTESIAN_POINT('Ctrl Pts',(-0.47422006101951,-1.,3.98030338044409));
#31508=CARTESIAN_POINT('Ctrl Pts',(-0.477718999122027,-1.,3.98709184306738));
#31509=CARTESIAN_POINT('Ctrl Pts',(-0.481258512209675,-1.,3.99386775880679));
#31510=CARTESIAN_POINT('Ctrl Pts',(-0.484838042421835,-1.,4.00063045119288));
#31511=CARTESIAN_POINT('Ctrl Pts',(-0.488457130424633,-1.,4.0073800839099));
#31512=CARTESIAN_POINT('Ctrl Pts',(-0.492115383418018,-1.,4.01411733503546));
#31513=CARTESIAN_POINT('Ctrl Pts',(-0.495812444326251,-1.,4.02084308851832));
#31514=CARTESIAN_POINT('Ctrl Pts',(-0.499547962340821,-1.,4.02755813980101));
#31515=CARTESIAN_POINT('Ctrl Pts',(-0.503321556915346,-1.,4.03426284174272));
#31516=CARTESIAN_POINT('Ctrl Pts',(-0.507132823288136,-1.,4.04095715148915));
#31517=CARTESIAN_POINT('Ctrl Pts',(-0.51098134921897,-1.,4.04764078815447));
#31518=CARTESIAN_POINT('Ctrl Pts',(-0.514866728193017,-1.,4.05431335771199));
#31519=CARTESIAN_POINT('Ctrl Pts',(-0.518788572336924,-1.,4.06097448038013));
#31520=CARTESIAN_POINT('Ctrl Pts',(-0.522746528603107,-1.,4.06762394471314));
#31521=CARTESIAN_POINT('Ctrl Pts',(-0.526740277227498,-1.,4.07426172299847));
#31522=CARTESIAN_POINT('Ctrl Pts',(-0.530769518728571,-1.,4.08088789536836));
#31523=CARTESIAN_POINT('Ctrl Pts',(-0.534833963477273,-1.,4.08750259988885));
#31524=CARTESIAN_POINT('Ctrl Pts',(-0.538933321179756,-1.,4.09410597627));
#31525=CARTESIAN_POINT('Ctrl Pts',(-0.543067286877757,-1.,4.10069810243979));
#31526=CARTESIAN_POINT('Ctrl Pts',(-0.547235539485637,-1.,4.10727897027977));
#31527=CARTESIAN_POINT('Ctrl Pts',(-0.551437758497033,-1.,4.11384852024721));
#31528=CARTESIAN_POINT('Ctrl Pts',(-0.555673636129977,-1.,4.12040666195664));
#31529=CARTESIAN_POINT('Ctrl Pts',(-0.559942890594774,-1.,4.12695329951961));
#31530=CARTESIAN_POINT('Ctrl Pts',(-0.564245279537149,-1.,4.13348835727104));
#31531=CARTESIAN_POINT('Ctrl Pts',(-0.568580610189775,-1.,4.14001179830547));
#31532=CARTESIAN_POINT('Ctrl Pts',(-0.572948736069522,-1.,4.14652361068081));
#31533=CARTESIAN_POINT('Ctrl Pts',(-0.576469391676688,-1.,4.151723761217));
#31534=CARTESIAN_POINT('Ctrl Pts',(-0.579124568914235,-1.,4.15561864788576));
#31535=CARTESIAN_POINT('Ctrl Pts',(-0.580901211463535,-1.,4.1582129171283));
#31536=CARTESIAN_POINT('Ctrl Pts',(-0.581791163835815,-1.,4.15950947128175));
#31537=CARTESIAN_POINT('',(-0.73204283740062,-1.,4.13571194405636));
#31538=CARTESIAN_POINT('',(-0.581791163835815,-1.,4.15950947128175));
#31539=CARTESIAN_POINT('',(-0.786422660831985,-1.,3.66661143271685));
#31540=CARTESIAN_POINT('Ctrl Pts',(-0.73204283740062,-1.,4.13571194405636));
#31541=CARTESIAN_POINT('Ctrl Pts',(-0.73248857513516,-1.,4.1342038373684));
#31542=CARTESIAN_POINT('Ctrl Pts',(-0.733376589323546,-1.,4.13118752795207));
#31543=CARTESIAN_POINT('Ctrl Pts',(-0.734698226764092,-1.,4.12666277570844));
#31544=CARTESIAN_POINT('Ctrl Pts',(-0.736439634331345,-1.,4.120629196238));
#31545=CARTESIAN_POINT('Ctrl Pts',(-0.738581708225844,-1.,4.11308626951927));
#31546=CARTESIAN_POINT('Ctrl Pts',(-0.740688998553377,-1.,4.10554241757547));
#31547=CARTESIAN_POINT('Ctrl Pts',(-0.742761369689841,-1.,4.09799769702611));
#31548=CARTESIAN_POINT('Ctrl Pts',(-0.7447986497065,-1.,4.09045220253573));
#31549=CARTESIAN_POINT('Ctrl Pts',(-0.746800631492315,-1.,4.08290608095642));
#31550=CARTESIAN_POINT('Ctrl Pts',(-0.748767076680557,-1.,4.07535951056152));
#31551=CARTESIAN_POINT('Ctrl Pts',(-0.750697720484036,-1.,4.06781267242378));
#31552=CARTESIAN_POINT('Ctrl Pts',(-0.752592276483072,-1.,4.06026572221515));
#31553=CARTESIAN_POINT('Ctrl Pts',(-0.754450441816078,-1.,4.05271876687915));
#31554=CARTESIAN_POINT('Ctrl Pts',(-0.756271902369581,-1.,4.04517182653997));
#31555=CARTESIAN_POINT('Ctrl Pts',(-0.758056338884944,-1.,4.03762485803119));
#31556=CARTESIAN_POINT('Ctrl Pts',(-0.759803433243752,-1.,4.03007781954412));
#31557=CARTESIAN_POINT('Ctrl Pts',(-0.761512875859804,-1.,4.02253072741268));
#31558=CARTESIAN_POINT('Ctrl Pts',(-0.763184371182935,-1.,4.01498370680496));
#31559=CARTESIAN_POINT('Ctrl Pts',(-0.764817648785198,-1.,4.00743706791509));
#31560=CARTESIAN_POINT('Ctrl Pts',(-0.766412457136064,-1.,3.99989129179622));
#31561=CARTESIAN_POINT('Ctrl Pts',(-0.767968531377915,-1.,3.9923468788101));
#31562=CARTESIAN_POINT('Ctrl Pts',(-0.769485566245544,-1.,3.98480422348451));
#31563=CARTESIAN_POINT('Ctrl Pts',(-0.770963190030471,-1.,3.97726349165488));
#31564=CARTESIAN_POINT('Ctrl Pts',(-0.772400931772136,-1.,3.96972446532772));
#31565=CARTESIAN_POINT('Ctrl Pts',(-0.773798212026566,-1.,3.96218649639807));
#31566=CARTESIAN_POINT('Ctrl Pts',(-0.775154418039352,-1.,3.9546488545231));
#31567=CARTESIAN_POINT('Ctrl Pts',(-0.776468966697921,-1.,3.94711101619447));
#31568=CARTESIAN_POINT('Ctrl Pts',(-0.777741370568559,-1.,3.93957296768103));
#31569=CARTESIAN_POINT('Ctrl Pts',(-0.778971308134821,-1.,3.93203552473174));
#31570=CARTESIAN_POINT('Ctrl Pts',(-0.780158678615543,-1.,3.92450058323823));
#31571=CARTESIAN_POINT('Ctrl Pts',(-0.781303428618367,-1.,3.91697036054676));
#31572=CARTESIAN_POINT('Ctrl Pts',(-0.782405395622764,-1.,3.90944671004542));
#31573=CARTESIAN_POINT('Ctrl Pts',(-0.783464141529081,-1.,3.9019303904397));
#31574=CARTESIAN_POINT('Ctrl Pts',(-0.784478799358336,-1.,3.89442039235103));
#31575=CARTESIAN_POINT('Ctrl Pts',(-0.78544789034073,-1.,3.88691313167398));
#31576=CARTESIAN_POINT('Ctrl Pts',(-0.786369675812609,-1.,3.8794040281819));
#31577=CARTESIAN_POINT('Ctrl Pts',(-0.787242527617999,-1.,3.87188916600912));
#31578=CARTESIAN_POINT('Ctrl Pts',(-0.788065315093778,-1.,3.86436702561345));
#31579=CARTESIAN_POINT('Ctrl Pts',(-0.788837734090672,-1.,3.85683995872529));
#31580=CARTESIAN_POINT('Ctrl Pts',(-0.789560798155582,-1.,3.84931637808894));
#31581=CARTESIAN_POINT('Ctrl Pts',(-0.790236124191242,-1.,3.84180762342454));
#31582=CARTESIAN_POINT('Ctrl Pts',(-0.790865012705301,-1.,3.83432392054786));
#31583=CARTESIAN_POINT('Ctrl Pts',(-0.791447528662369,-1.,3.82687033899792));
#31584=CARTESIAN_POINT('Ctrl Pts',(-0.791981740718635,-1.,3.81944345442249));
#31585=CARTESIAN_POINT('Ctrl Pts',(-0.792462483517634,-1.,3.81202588694756));
#31586=CARTESIAN_POINT('Ctrl Pts',(-0.792882695234778,-1.,3.80459229925637));
#31587=CARTESIAN_POINT('Ctrl Pts',(-0.793235612973273,-1.,3.79711921389897));
#31588=CARTESIAN_POINT('Ctrl Pts',(-0.793516871680993,-1.,3.78959439439235));
#31589=CARTESIAN_POINT('Ctrl Pts',(-0.7937262357813,-1.,3.78202460377598));
#31590=CARTESIAN_POINT('Ctrl Pts',(-0.793870523787408,-1.,3.77444863801212));
#31591=CARTESIAN_POINT('Ctrl Pts',(-0.793961083688992,-1.,3.76692626931111));
#31592=CARTESIAN_POINT('Ctrl Pts',(-0.794008429134907,-1.,3.75951468666257));
#31593=CARTESIAN_POINT('Ctrl Pts',(-0.794017347371377,-1.,3.75224692493864));
#31594=CARTESIAN_POINT('Ctrl Pts',(-0.793982700459952,-1.,3.74511357728861));
#31595=CARTESIAN_POINT('Ctrl Pts',(-0.793882700937017,-1.,3.73803280541687));
#31596=CARTESIAN_POINT('Ctrl Pts',(-0.793682750269684,-1.,3.73086914695805));
#31597=CARTESIAN_POINT('Ctrl Pts',(-0.793347023784205,-1.,3.72348797293734));
#31598=CARTESIAN_POINT('Ctrl Pts',(-0.792848377370287,-1.,3.71580242396124));
#31599=CARTESIAN_POINT('Ctrl Pts',(-0.792177688845818,-1.,3.70781724021806));
#31600=CARTESIAN_POINT('Ctrl Pts',(-0.79135657569598,-1.,3.69968940808721));
#31601=CARTESIAN_POINT('Ctrl Pts',(-0.790436284988788,-1.,3.69172044327364));
#31602=CARTESIAN_POINT('Ctrl Pts',(-0.789483546064387,-1.,3.68428439783905));
#31603=CARTESIAN_POINT('Ctrl Pts',(-0.788569566220285,-1.,3.67777119516252));
#31604=CARTESIAN_POINT('Ctrl Pts',(-0.787758799995743,-1.,3.67252923663655));
#31605=CARTESIAN_POINT('Ctrl Pts',(-0.787145041181546,-1.,3.66907505398677));
#31606=CARTESIAN_POINT('Ctrl Pts',(-0.786774337198062,-1.,3.66743103898702));
#31607=CARTESIAN_POINT('Ctrl Pts',(-0.786565919558984,-1.,3.66680946938292));
#31608=CARTESIAN_POINT('Ctrl Pts',(-0.786459983895432,-1.,3.6666431041522));
#31609=CARTESIAN_POINT('Ctrl Pts',(-0.786422660831985,-1.,3.66661143271685));
#31610=CARTESIAN_POINT('',(-0.963899035117249,-1.,3.62400312501245));
#31611=CARTESIAN_POINT('Origin',(0.,-1.,0.));
#31612=CARTESIAN_POINT('',(-1.22531898815164,-1.,4.01728681790024));
#31613=CARTESIAN_POINT('Ctrl Pts',(-0.963899035117249,-1.,3.62400312501245));
#31614=CARTESIAN_POINT('Ctrl Pts',(-0.963880158555582,-1.,3.6240482887845));
#31615=CARTESIAN_POINT('Ctrl Pts',(-0.963861297423241,-1.,3.62424461507588));
#31616=CARTESIAN_POINT('Ctrl Pts',(-0.963957782642843,-1.,3.62489305727662));
#31617=CARTESIAN_POINT('Ctrl Pts',(-0.964373850166458,-1.,3.62652618145335));
#31618=CARTESIAN_POINT('Ctrl Pts',(-0.965395153165293,-1.,3.62988252139846));
#31619=CARTESIAN_POINT('Ctrl Pts',(-0.967052554541386,-1.,3.63492122081143));
#31620=CARTESIAN_POINT('Ctrl Pts',(-0.969195124675866,-1.,3.64113946505766));
#31621=CARTESIAN_POINT('Ctrl Pts',(-0.971722122061341,-1.,3.64819756447455));
#31622=CARTESIAN_POINT('Ctrl Pts',(-0.974519971354848,-1.,3.65571576735126));
#31623=CARTESIAN_POINT('Ctrl Pts',(-0.977478312751618,-1.,3.66333049637475));
#31624=CARTESIAN_POINT('Ctrl Pts',(-0.980505922458267,-1.,3.67074983340361));
#31625=CARTESIAN_POINT('Ctrl Pts',(-0.983550791470419,-1.,3.67782408841715));
#31626=CARTESIAN_POINT('Ctrl Pts',(-0.986602639863838,-1.,3.68455317926068));
#31627=CARTESIAN_POINT('Ctrl Pts',(-0.989676715398558,-1.,3.69102682138846));
#31628=CARTESIAN_POINT('Ctrl Pts',(-0.99280221833201,-1.,3.69738123415662));
#31629=CARTESIAN_POINT('Ctrl Pts',(-0.996009819772518,-1.,3.70375282282138));
#31630=CARTESIAN_POINT('Ctrl Pts',(-0.999317260756531,-1.,3.71022439713938));
#31631=CARTESIAN_POINT('Ctrl Pts',(-1.00272423396822,-1.,3.71680667125118));
#31632=CARTESIAN_POINT('Ctrl Pts',(-1.0062200073571,-1.,3.72346803750595));
#31633=CARTESIAN_POINT('Ctrl Pts',(-1.00978798539496,-1.,3.73015276704426));
#31634=CARTESIAN_POINT('Ctrl Pts',(-1.01341114319903,-1.,3.73680245055734));
#31635=CARTESIAN_POINT('Ctrl Pts',(-1.01707794311079,-1.,3.74337942504959));
#31636=CARTESIAN_POINT('Ctrl Pts',(-1.02078510487428,-1.,3.74987777155834));
#31637=CARTESIAN_POINT('Ctrl Pts',(-1.0245342944466,-1.,3.75631037456194));
#31638=CARTESIAN_POINT('Ctrl Pts',(-1.02833014458181,-1.,3.76270122291232));
#31639=CARTESIAN_POINT('Ctrl Pts',(-1.0321778660492,-1.,3.76907609832522));
#31640=CARTESIAN_POINT('Ctrl Pts',(-1.03608074678013,-1.,3.77545283140445));
#31641=CARTESIAN_POINT('Ctrl Pts',(-1.04003862055804,-1.,3.78183535008192));
#31642=CARTESIAN_POINT('Ctrl Pts',(-1.04404924374426,-1.,3.78821910787195));
#31643=CARTESIAN_POINT('Ctrl Pts',(-1.04810913267641,-1.,3.79459440308793));
#31644=CARTESIAN_POINT('Ctrl Pts',(-1.05221457990015,-1.,3.80095039790678));
#31645=CARTESIAN_POINT('Ctrl Pts',(-1.05636266918643,-1.,3.80727913637784));
#31646=CARTESIAN_POINT('Ctrl Pts',(-1.06055206187298,-1.,3.81357866117485));
#31647=CARTESIAN_POINT('Ctrl Pts',(-1.06478244038931,-1.,3.81985083953012));
#31648=CARTESIAN_POINT('Ctrl Pts',(-1.0690541318036,-1.,3.82609989967278));
#31649=CARTESIAN_POINT('Ctrl Pts',(-1.0733676663346,-1.,3.83233071195145));
#31650=CARTESIAN_POINT('Ctrl Pts',(-1.07772335353856,-1.,3.83854714117486));
#31651=CARTESIAN_POINT('Ctrl Pts',(-1.08212087917986,-1.,3.84475048030615));
#31652=CARTESIAN_POINT('Ctrl Pts',(-1.08655950846377,-1.,3.8509402522269));
#31653=CARTESIAN_POINT('Ctrl Pts',(-1.09103825516288,-1.,3.85711487933911));
#31654=CARTESIAN_POINT('Ctrl Pts',(-1.09555606505012,-1.,3.86327241021242));
#31655=CARTESIAN_POINT('Ctrl Pts',(-1.10011198761202,-1.,3.86941120134872));
#31656=CARTESIAN_POINT('Ctrl Pts',(-1.10470536603303,-1.,3.87553067187566));
#31657=CARTESIAN_POINT('Ctrl Pts',(-1.10933577224029,-1.,3.88163105531791));
#31658=CARTESIAN_POINT('Ctrl Pts',(-1.11400292434447,-1.,3.88771308285229));
#31659=CARTESIAN_POINT('Ctrl Pts',(-1.11870660794609,-1.,3.89377768340362));
#31660=CARTESIAN_POINT('Ctrl Pts',(-1.12344660099029,-1.,3.89982569749978));
#31661=CARTESIAN_POINT('Ctrl Pts',(-1.12822258281518,-1.,3.90585753318622));
#31662=CARTESIAN_POINT('Ctrl Pts',(-1.13303414693849,-1.,3.91187321145495));
#31663=CARTESIAN_POINT('Ctrl Pts',(-1.13788084225511,-1.,3.91787251936688));
#31664=CARTESIAN_POINT('Ctrl Pts',(-1.14276220561575,-1.,3.92385513133937));
#31665=CARTESIAN_POINT('Ctrl Pts',(-1.14767779451147,-1.,3.92982073294334));
#31666=CARTESIAN_POINT('Ctrl Pts',(-1.15262722716391,-1.,3.9357691705651));
#31667=CARTESIAN_POINT('Ctrl Pts',(-1.1576101834106,-1.,3.94170046685542));
#31668=CARTESIAN_POINT('Ctrl Pts',(-1.16262637999261,-1.,3.9476147478092));
#31669=CARTESIAN_POINT('Ctrl Pts',(-1.16767555244495,-1.,3.95351219510062));
#31670=CARTESIAN_POINT('Ctrl Pts',(-1.17275743590327,-1.,3.95939299213164));
#31671=CARTESIAN_POINT('Ctrl Pts',(-1.17787174135445,-1.,3.96525726357682));
#31672=CARTESIAN_POINT('Ctrl Pts',(-1.18301815039596,-1.,3.9711050516465));
#31673=CARTESIAN_POINT('Ctrl Pts',(-1.18819633715285,-1.,3.97693634766926));
#31674=CARTESIAN_POINT('Ctrl Pts',(-1.19340598349307,-1.,3.98275111052015));
#31675=CARTESIAN_POINT('Ctrl Pts',(-1.19864679609596,-1.,3.98854928957287));
#31676=CARTESIAN_POINT('Ctrl Pts',(-1.2039185237544,-1.,3.99433084800649));
#31677=CARTESIAN_POINT('Ctrl Pts',(-1.20922097030107,-1.,4.00009577952534));
#31678=CARTESIAN_POINT('Ctrl Pts',(-1.21455398918813,-1.,4.00584409524937));
#31679=CARTESIAN_POINT('Ctrl Pts',(-1.21884478244983,-1.,4.01042947142681));
#31680=CARTESIAN_POINT('Ctrl Pts',(-1.22207656456199,-1.,4.01386104434674));
#31681=CARTESIAN_POINT('Ctrl Pts',(-1.22423716681447,-1.,4.0161454457032));
#31682=CARTESIAN_POINT('Ctrl Pts',(-1.22531898815164,-1.,4.01728681790024));
#31683=CARTESIAN_POINT('',(-1.36999806084572,-1.,3.97027773754922));
#31684=CARTESIAN_POINT('',(-1.22531898815164,-1.,4.01728681790024));
#31685=CARTESIAN_POINT('',(-1.35032489087101,-1.,3.4984457533445));
#31686=CARTESIAN_POINT('Ctrl Pts',(-1.36999806084572,-1.,3.97027773754922));
#31687=CARTESIAN_POINT('Ctrl Pts',(-1.37020239094614,-1.,3.9687184694131));
#31688=CARTESIAN_POINT('Ctrl Pts',(-1.37060761745635,-1.,3.96560037974645));
#31689=CARTESIAN_POINT('Ctrl Pts',(-1.3712051561502,-1.,3.96092458506535));
#31690=CARTESIAN_POINT('Ctrl Pts',(-1.37198126432386,-1.,3.95469287280914));
#31691=CARTESIAN_POINT('Ctrl Pts',(-1.37291699202807,-1.,3.94690771785133));
#31692=CARTESIAN_POINT('Ctrl Pts',(-1.37381821967165,-1.,3.93912709040818));
#31693=CARTESIAN_POINT('Ctrl Pts',(-1.37468482215751,-1.,3.93135106761844));
#31694=CARTESIAN_POINT('Ctrl Pts',(-1.37551664448242,-1.,3.92357976987672));
#31695=CARTESIAN_POINT('Ctrl Pts',(-1.37631350505797,-1.,3.91581337462644));
#31696=CARTESIAN_POINT('Ctrl Pts',(-1.3770751963402,-1.,3.90805209523486));
#31697=CARTESIAN_POINT('Ctrl Pts',(-1.37780148512792,-1.,3.90029615196727));
#31698=CARTESIAN_POINT('Ctrl Pts',(-1.3784921128802,-1.,3.89254574338496));
#31699=CARTESIAN_POINT('Ctrl Pts',(-1.37914679719383,-1.,3.88480102249277));
#31700=CARTESIAN_POINT('Ctrl Pts',(-1.37976523097073,-1.,3.87706205830532));
#31701=CARTESIAN_POINT('Ctrl Pts',(-1.38034709213014,-1.,3.86932885813068));
#31702=CARTESIAN_POINT('Ctrl Pts',(-1.38089205992989,-1.,3.86160143043959));
#31703=CARTESIAN_POINT('Ctrl Pts',(-1.38139983115049,-1.,3.85387983979481));
#31704=CARTESIAN_POINT('Ctrl Pts',(-1.38187013346109,-1.,3.84616425605764));
#31705=CARTESIAN_POINT('Ctrl Pts',(-1.38230274828822,-1.,3.83845502790746));
#31706=CARTESIAN_POINT('Ctrl Pts',(-1.38269750245138,-1.,3.8307526698229));
#31707=CARTESIAN_POINT('Ctrl Pts',(-1.38305421262763,-1.,3.82305771743829));
#31708=CARTESIAN_POINT('Ctrl Pts',(-1.38337263902782,-1.,3.81537060817811));
#31709=CARTESIAN_POINT('Ctrl Pts',(-1.3836524404622,-1.,3.80769156398411));
#31710=CARTESIAN_POINT('Ctrl Pts',(-1.38389311766682,-1.,3.80002044322111));
#31711=CARTESIAN_POINT('Ctrl Pts',(-1.38409399694566,-1.,3.79235669640841));
#31712=CARTESIAN_POINT('Ctrl Pts',(-1.38425435883756,-1.,3.78469969805082));
#31713=CARTESIAN_POINT('Ctrl Pts',(-1.38437354551428,-1.,3.77704902230418));
#31714=CARTESIAN_POINT('Ctrl Pts',(-1.38445107339518,-1.,3.76940473185779));
#31715=CARTESIAN_POINT('Ctrl Pts',(-1.3844867525335,-1.,3.76176768271367));
#31716=CARTESIAN_POINT('Ctrl Pts',(-1.38448077997163,-1.,3.7541397631875));
#31717=CARTESIAN_POINT('Ctrl Pts',(-1.38443344984394,-1.,3.74652317167876));
#31718=CARTESIAN_POINT('Ctrl Pts',(-1.38434489156458,-1.,3.73891976418104));
#31719=CARTESIAN_POINT('Ctrl Pts',(-1.38421479111531,-1.,3.73133035859282));
#31720=CARTESIAN_POINT('Ctrl Pts',(-1.3840421342895,-1.,3.72375409358803));
#31721=CARTESIAN_POINT('Ctrl Pts',(-1.38382489984586,-1.,3.7161876605181));
#31722=CARTESIAN_POINT('Ctrl Pts',(-1.38356065402124,-1.,3.70862680753347));
#31723=CARTESIAN_POINT('Ctrl Pts',(-1.38324717612865,-1.,3.701067921679));
#31724=CARTESIAN_POINT('Ctrl Pts',(-1.38288311171651,-1.,3.69350967899526));
#31725=CARTESIAN_POINT('Ctrl Pts',(-1.38246852827182,-1.,3.68595444983837));
#31726=CARTESIAN_POINT('Ctrl Pts',(-1.3820057429062,-1.,3.67841038482414));
#31727=CARTESIAN_POINT('Ctrl Pts',(-1.38149812653868,-1.,3.67088843112262));
#31728=CARTESIAN_POINT('Ctrl Pts',(-1.38094856333552,-1.,3.66339848520857));
#31729=CARTESIAN_POINT('Ctrl Pts',(-1.38035791051213,-1.,3.6559455440439));
#31730=CARTESIAN_POINT('Ctrl Pts',(-1.37972372481603,-1.,3.64852652756456));
#31731=CARTESIAN_POINT('Ctrl Pts',(-1.37903818567359,-1.,3.64112507791141));
#31732=CARTESIAN_POINT('Ctrl Pts',(-1.37829035457339,-1.,3.63371727442486));
#31733=CARTESIAN_POINT('Ctrl Pts',(-1.37746987919881,-1.,3.62628098665145));
#31734=CARTESIAN_POINT('Ctrl Pts',(-1.37657053403107,-1.,3.6188048116042));
#31735=CARTESIAN_POINT('Ctrl Pts',(-1.37559314436634,-1.,3.61129546591064));
#31736=CARTESIAN_POINT('Ctrl Pts',(-1.37455051379623,-1.,3.60379020123988));
#31737=CARTESIAN_POINT('Ctrl Pts',(-1.37346320103157,-1.,3.59634627869048));
#31738=CARTESIAN_POINT('Ctrl Pts',(-1.37235053660976,-1.,3.58901853846365));
#31739=CARTESIAN_POINT('Ctrl Pts',(-1.37122241663062,-1.,3.58183885982715));
#31740=CARTESIAN_POINT('Ctrl Pts',(-1.37007229485659,-1.,3.57479875549486));
#31741=CARTESIAN_POINT('Ctrl Pts',(-1.36886584973389,-1.,3.5678208030466));
#31742=CARTESIAN_POINT('Ctrl Pts',(-1.36754771771233,-1.,3.56077662028649));
#31743=CARTESIAN_POINT('Ctrl Pts',(-1.3660614545677,-1.,3.55353883995949));
#31744=CARTESIAN_POINT('Ctrl Pts',(-1.36436666257598,-1.,3.54602591832973));
#31745=CARTESIAN_POINT('Ctrl Pts',(-1.36245507339307,-1.,3.53824396424961));
#31746=CARTESIAN_POINT('Ctrl Pts',(-1.36037259643734,-1.,3.530344649616));
#31747=CARTESIAN_POINT('Ctrl Pts',(-1.35821701528836,-1.,3.52261776116748));
#31748=CARTESIAN_POINT('Ctrl Pts',(-1.35611275237152,-1.,3.51542230699556));
#31749=CARTESIAN_POINT('Ctrl Pts',(-1.35419113575956,-1.,3.50913227059999));
#31750=CARTESIAN_POINT('Ctrl Pts',(-1.35257032843486,-1.,3.50408168106261));
#31751=CARTESIAN_POINT('Ctrl Pts',(-1.35142377279517,-1.,3.5007660381649));
#31752=CARTESIAN_POINT('Ctrl Pts',(-1.35080045218587,-1.,3.49920025459723));
#31753=CARTESIAN_POINT('Ctrl Pts',(-1.35049736560527,-1.,3.49861894124827));
#31754=CARTESIAN_POINT('Ctrl Pts',(-1.35036670892966,-1.,3.49847119623846));
#31755=CARTESIAN_POINT('Ctrl Pts',(-1.35032489087101,-1.,3.4984457533445));
#31756=CARTESIAN_POINT('',(-1.51895082866166,-1.,3.42859860294378));
#31757=CARTESIAN_POINT('Origin',(0.,-1.,0.));
#31758=CARTESIAN_POINT('',(-1.83867539237861,-1.,3.77614523045147));
#31759=CARTESIAN_POINT('Ctrl Pts',(-1.51895082866166,-1.,3.42859860294378));
#31760=CARTESIAN_POINT('Ctrl Pts',(-1.51893924967231,-1.,3.42864616361967));
#31761=CARTESIAN_POINT('Ctrl Pts',(-1.51895133295017,-1.,3.42884302333978));
#31762=CARTESIAN_POINT('Ctrl Pts',(-1.51914806898539,-1.,3.42946838852728));
#31763=CARTESIAN_POINT('Ctrl Pts',(-1.5198144909343,-1.,3.4310163189349));
#31764=CARTESIAN_POINT('Ctrl Pts',(-1.52134826724227,-1.,3.43417156977749));
#31765=CARTESIAN_POINT('Ctrl Pts',(-1.52377348950429,-1.,3.43888895974182));
#31766=CARTESIAN_POINT('Ctrl Pts',(-1.52686242875717,-1.,3.44469547527));
#31767=CARTESIAN_POINT('Ctrl Pts',(-1.530462444618,-1.,3.45127136828667));
#31768=CARTESIAN_POINT('Ctrl Pts',(-1.53440195378902,-1.,3.45825932955273));
#31769=CARTESIAN_POINT('Ctrl Pts',(-1.53851507915533,-1.,3.46531752207222));
#31770=CARTESIAN_POINT('Ctrl Pts',(-1.54266605398152,-1.,3.47217189224576));
#31771=CARTESIAN_POINT('Ctrl Pts',(-1.54678009290207,-1.,3.47868272898599));
#31772=CARTESIAN_POINT('Ctrl Pts',(-1.55084702970382,-1.,3.48485155928414));
#31773=CARTESIAN_POINT('Ctrl Pts',(-1.5548959590107,-1.,3.49076460877317));
#31774=CARTESIAN_POINT('Ctrl Pts',(-1.55897703097859,-1.,3.49655185179623));
#31775=CARTESIAN_POINT('Ctrl Pts',(-1.56314187758689,-1.,3.50234321621607));
#31776=CARTESIAN_POINT('Ctrl Pts',(-1.56742097575041,-1.,3.50821771695427));
#31777=CARTESIAN_POINT('Ctrl Pts',(-1.57181569799774,-1.,3.51418598431733));
#31778=CARTESIAN_POINT('Ctrl Pts',(-1.5763104998818,-1.,3.52021847865961));
#31779=CARTESIAN_POINT('Ctrl Pts',(-1.58088027227856,-1.,3.52626275334899));
#31780=CARTESIAN_POINT('Ctrl Pts',(-1.58549906268083,-1.,3.53226378147068));
#31781=CARTESIAN_POINT('Ctrl Pts',(-1.59014958368725,-1.,3.53818616861045));
#31782=CARTESIAN_POINT('Ctrl Pts',(-1.5948276694975,-1.,3.544024581823));
#31783=CARTESIAN_POINT('Ctrl Pts',(-1.59953698113444,-1.,3.54979148634426));
#31784=CARTESIAN_POINT('Ctrl Pts',(-1.60428584699848,-1.,3.55550985096117));
#31785=CARTESIAN_POINT('Ctrl Pts',(-1.60908344685459,-1.,3.56120432482986));
#31786=CARTESIAN_POINT('Ctrl Pts',(-1.61393581747522,-1.,3.56689200468404));
#31787=CARTESIAN_POINT('Ctrl Pts',(-1.61884340915412,-1.,3.57257679609826));
#31788=CARTESIAN_POINT('Ctrl Pts',(-1.62380329464851,-1.,3.57825455954405));
#31789=CARTESIAN_POINT('Ctrl Pts',(-1.62881051550748,-1.,3.5839162577435));
#31790=CARTESIAN_POINT('Ctrl Pts',(-1.63385971451259,-1.,3.58955176627876));
#31791=CARTESIAN_POINT('Ctrl Pts',(-1.63894676675349,-1.,3.59515368334887));
#31792=CARTESIAN_POINT('Ctrl Pts',(-1.6440700438558,-1.,3.6007202851384));
#31793=CARTESIAN_POINT('Ctrl Pts',(-1.64922952425833,-1.,3.60625346556992));
#31794=CARTESIAN_POINT('Ctrl Pts',(-1.65442619244327,-1.,3.61175734965129));
#31795=CARTESIAN_POINT('Ctrl Pts',(-1.65966133399186,-1.,3.61723666482457));
#31796=CARTESIAN_POINT('Ctrl Pts',(-1.66493585923853,-1.,3.62269517989104));
#31797=CARTESIAN_POINT('Ctrl Pts',(-1.67024966008037,-1.,3.62813422105257));
#31798=CARTESIAN_POINT('Ctrl Pts',(-1.67560193613145,-1.,3.63355343201211));
#31799=CARTESIAN_POINT('Ctrl Pts',(-1.68099146651577,-1.,3.63895140887443));
#31800=CARTESIAN_POINT('Ctrl Pts',(-1.68641690471455,-1.,3.64432638915199));
#31801=CARTESIAN_POINT('Ctrl Pts',(-1.691877054817,-1.,3.64967689827393));
#31802=CARTESIAN_POINT('Ctrl Pts',(-1.69737117722559,-1.,3.65500246526798));
#31803=CARTESIAN_POINT('Ctrl Pts',(-1.70289888566904,-1.,3.6603033877491));
#31804=CARTESIAN_POINT('Ctrl Pts',(-1.70846001610983,-1.,3.6655804319893));
#31805=CARTESIAN_POINT('Ctrl Pts',(-1.71405450210392,-1.,3.67083454901629));
#31806=CARTESIAN_POINT('Ctrl Pts',(-1.71968225581787,-1.,3.67606660374665));
#31807=CARTESIAN_POINT('Ctrl Pts',(-1.72534302437003,-1.,3.68127704936472));
#31808=CARTESIAN_POINT('Ctrl Pts',(-1.73103640956647,-1.,3.68646597019188));
#31809=CARTESIAN_POINT('Ctrl Pts',(-1.73676193254493,-1.,3.69163322647906));
#31810=CARTESIAN_POINT('Ctrl Pts',(-1.74251908492589,-1.,3.6967785691046));
#31811=CARTESIAN_POINT('Ctrl Pts',(-1.74830738046092,-1.,3.70190175673422));
#31812=CARTESIAN_POINT('Ctrl Pts',(-1.75412641804148,-1.,3.70700269736876));
#31813=CARTESIAN_POINT('Ctrl Pts',(-1.75997588499021,-1.,3.71208146346454));
#31814=CARTESIAN_POINT('Ctrl Pts',(-1.76585552124549,-1.,3.71713822377675));
#31815=CARTESIAN_POINT('Ctrl Pts',(-1.77176509401846,-1.,3.72217319911429));
#31816=CARTESIAN_POINT('Ctrl Pts',(-1.77770437039606,-1.,3.72718661205504));
#31817=CARTESIAN_POINT('Ctrl Pts',(-1.78367308442682,-1.,3.73217863095022));
#31818=CARTESIAN_POINT('Ctrl Pts',(-1.78967092823139,-1.,3.73714934729962));
#31819=CARTESIAN_POINT('Ctrl Pts',(-1.79569757859041,-1.,3.74209880351667));
#31820=CARTESIAN_POINT('Ctrl Pts',(-1.80175271485519,-1.,3.74702700874954));
#31821=CARTESIAN_POINT('Ctrl Pts',(-1.80783603939662,-1.,3.75193395888069));
#31822=CARTESIAN_POINT('Ctrl Pts',(-1.81394729834032,-1.,3.75681965683995));
#31823=CARTESIAN_POINT('Ctrl Pts',(-1.82008629694924,-1.,3.76168412709652));
#31824=CARTESIAN_POINT('Ctrl Pts',(-1.82625289221933,-1.,3.76652740355856));
#31825=CARTESIAN_POINT('Ctrl Pts',(-1.83120816956515,-1.,3.77038509819777));
#31826=CARTESIAN_POINT('Ctrl Pts',(-1.83493697935064,-1.,3.77326886065484));
#31827=CARTESIAN_POINT('Ctrl Pts',(-1.83742834010821,-1.,3.77518714458232));
#31828=CARTESIAN_POINT('Ctrl Pts',(-1.83867539237861,-1.,3.77614523045147));
#31829=CARTESIAN_POINT('',(-1.97421938526992,-1.,3.70708211654725));
#31830=CARTESIAN_POINT('',(-1.83867539237861,-1.,3.77614523045147));
#31831=CARTESIAN_POINT('',(-1.88097764062542,-1.,3.24413672884902));
#31832=CARTESIAN_POINT('Ctrl Pts',(-1.97421938526992,-1.,3.70708211654725));
#31833=CARTESIAN_POINT('Ctrl Pts',(-1.974177276451,-1.,3.7055100813194));
#31834=CARTESIAN_POINT('Ctrl Pts',(-1.97408973726149,-1.,3.70236698911837));
#31835=CARTESIAN_POINT('Ctrl Pts',(-1.97394846382289,-1.,3.69765528558292));
#31836=CARTESIAN_POINT('Ctrl Pts',(-1.97374016224397,-1.,3.69137888597855));
#31837=CARTESIAN_POINT('Ctrl Pts',(-1.97344650303631,-1.,3.68354319913416));
#31838=CARTESIAN_POINT('Ctrl Pts',(-1.97311947678035,-1.,3.67571738106175));
#31839=CARTESIAN_POINT('Ctrl Pts',(-1.9727589719863,-1.,3.66790152751984));
#31840=CARTESIAN_POINT('Ctrl Pts',(-1.97236485439317,-1.,3.66009578166865));
#31841=CARTESIAN_POINT('Ctrl Pts',(-1.97193697240645,-1.,3.65230034717364));
#31842=CARTESIAN_POINT('Ctrl Pts',(-1.97147515441539,-1.,3.64451546724221));
#31843=CARTESIAN_POINT('Ctrl Pts',(-1.97097920454698,-1.,3.63674139590853));
#31844=CARTESIAN_POINT('Ctrl Pts',(-1.97044889850518,-1.,3.62897836973397));
#31845=CARTESIAN_POINT('Ctrl Pts',(-1.96988398129888,-1.,3.62122658401722));
#31846=CARTESIAN_POINT('Ctrl Pts',(-1.96928416040712,-1.,3.61348615496393));
#31847=CARTESIAN_POINT('Ctrl Pts',(-1.96864911885775,-1.,3.60575714017676));
#31848=CARTESIAN_POINT('Ctrl Pts',(-1.96797854118257,-1.,3.59803959819725));
#31849=CARTESIAN_POINT('Ctrl Pts',(-1.96727213799507,-1.,3.5903336402273));
#31850=CARTESIAN_POINT('Ctrl Pts',(-1.9665296668894,-1.,3.58263947663884));
#31851=CARTESIAN_POINT('Ctrl Pts',(-1.96575096652857,-1.,3.57495748601088));
#31852=CARTESIAN_POINT('Ctrl Pts',(-1.96493594634643,-1.,3.56728820357933));
#31853=CARTESIAN_POINT('Ctrl Pts',(-1.96408450906868,-1.,3.55963218706201));
#31854=CARTESIAN_POINT('Ctrl Pts',(-1.96319648628667,-1.,3.55198990600929));
#31855=CARTESIAN_POINT('Ctrl Pts',(-1.96227157573058,-1.,3.54436163300425));
#31856=CARTESIAN_POINT('Ctrl Pts',(-1.96130926212661,-1.,3.53674730625759));
#31857=CARTESIAN_POINT('Ctrl Pts',(-1.96030879411534,-1.,3.52914648844289));
#31858=CARTESIAN_POINT('Ctrl Pts',(-1.95926936324436,-1.,3.52155867431438));
#31859=CARTESIAN_POINT('Ctrl Pts',(-1.95819025316768,-1.,3.51398354617772));
#31860=CARTESIAN_POINT('Ctrl Pts',(-1.95707099606514,-1.,3.50642124159913));
#31861=CARTESIAN_POINT('Ctrl Pts',(-1.9559115382367,-1.,3.49887263575602));
#31862=CARTESIAN_POINT('Ctrl Pts',(-1.95471236969653,-1.,3.49133956289154));
#31863=CARTESIAN_POINT('Ctrl Pts',(-1.95347412486316,-1.,3.48382414832648));
#31864=CARTESIAN_POINT('Ctrl Pts',(-1.95219722189878,-1.,3.47632820495926));
#31865=CARTESIAN_POINT('Ctrl Pts',(-1.95088147859876,-1.,3.4688525897419));
#31866=CARTESIAN_POINT('Ctrl Pts',(-1.94952575850196,-1.,3.46139661060959));
#31867=CARTESIAN_POINT('Ctrl Pts',(-1.94812754766524,-1.,3.45395731584051));
#31868=CARTESIAN_POINT('Ctrl Pts',(-1.94668377715332,-1.,3.44653088665685));
#31869=CARTESIAN_POINT('Ctrl Pts',(-1.94519168842883,-1.,3.43911410197693));
#31870=CARTESIAN_POINT('Ctrl Pts',(-1.94364973660285,-1.,3.43170586602436));
#31871=CARTESIAN_POINT('Ctrl Pts',(-1.94205835913692,-1.,3.42430850941497));
#31872=CARTESIAN_POINT('Ctrl Pts',(-1.94042111965237,-1.,3.41692971994082));
#31873=CARTESIAN_POINT('Ctrl Pts',(-1.93874306008132,-1.,3.40957978266622));
#31874=CARTESIAN_POINT('Ctrl Pts',(-1.93702857723089,-1.,3.40226802104093));
#31875=CARTESIAN_POINT('Ctrl Pts',(-1.93527929945982,-1.,3.39499923640789));
#31876=CARTESIAN_POINT('Ctrl Pts',(-1.93349233176794,-1.,3.38777076883267));
#31877=CARTESIAN_POINT('Ctrl Pts',(-1.93165739093292,-1.,3.38056768525577));
#31878=CARTESIAN_POINT('Ctrl Pts',(-1.92975993109897,-1.,3.37336807068078));
#31879=CARTESIAN_POINT('Ctrl Pts',(-1.92778626543803,-1.,3.36615168657597));
#31880=CARTESIAN_POINT('Ctrl Pts',(-1.92572846125763,-1.,3.35890824422976));
#31881=CARTESIAN_POINT('Ctrl Pts',(-1.92358838440518,-1.,3.35164424847206));
#31882=CARTESIAN_POINT('Ctrl Pts',(-1.92138450828378,-1.,3.34439448941915));
#31883=CARTESIAN_POINT('Ctrl Pts',(-1.91914609610173,-1.,3.33721230709948));
#31884=CARTESIAN_POINT('Ctrl Pts',(-1.91690081930297,-1.,3.33014884257812));
#31885=CARTESIAN_POINT('Ctrl Pts',(-1.91466343916612,-1.,3.32323403454507));
#31886=CARTESIAN_POINT('Ctrl Pts',(-1.91242616234459,-1.,3.31646052426395));
#31887=CARTESIAN_POINT('Ctrl Pts',(-1.91014297830502,-1.,3.30975721158694));
#31888=CARTESIAN_POINT('Ctrl Pts',(-1.90773912171424,-1.,3.30300595568341));
#31889=CARTESIAN_POINT('Ctrl Pts',(-1.9051389186417,-1.,3.29608978722258));
#31890=CARTESIAN_POINT('Ctrl Pts',(-1.9022897124757,-1.,3.28893448600364));
#31891=CARTESIAN_POINT('Ctrl Pts',(-1.89918429230425,-1.,3.28154737912287));
#31892=CARTESIAN_POINT('Ctrl Pts',(-1.89589172903662,-1.,3.27407108932908));
#31893=CARTESIAN_POINT('Ctrl Pts',(-1.89255393500769,-1.,3.2667765388833));
#31894=CARTESIAN_POINT('Ctrl Pts',(-1.88934996203508,-1.,3.2599988519361));
#31895=CARTESIAN_POINT('Ctrl Pts',(-1.88646802523372,-1.,3.25408686339298));
#31896=CARTESIAN_POINT('Ctrl Pts',(-1.88407708646435,-1.,3.24935200512055));
#31897=CARTESIAN_POINT('Ctrl Pts',(-1.88242596600422,-1.,3.24625654410705));
#31898=CARTESIAN_POINT('Ctrl Pts',(-1.88156537699118,-1.,3.24480754675942));
#31899=CARTESIAN_POINT('Ctrl Pts',(-1.88117508446657,-1.,3.24428080352952));
#31900=CARTESIAN_POINT('Ctrl Pts',(-1.88102292397987,-1.,3.2441553167131));
#31901=CARTESIAN_POINT('Ctrl Pts',(-1.88097764062542,-1.,3.24413672884902));
#31902=CARTESIAN_POINT('',(-2.03660101169564,-1.,3.14877060440425));
#31903=CARTESIAN_POINT('Origin',(0.,-1.,0.));
#31904=CARTESIAN_POINT('',(-2.40675750623143,-1.,3.44202241512147));
#31905=CARTESIAN_POINT('Ctrl Pts',(-2.03660101169564,-1.,3.14877060440425));
#31906=CARTESIAN_POINT('Ctrl Pts',(-2.03659701539175,-1.,3.1488193908823));
#31907=CARTESIAN_POINT('Ctrl Pts',(-2.03663974554941,-1.,3.14901193669147));
#31908=CARTESIAN_POINT('Ctrl Pts',(-2.03693188810614,-1.,3.14959882629936));
#31909=CARTESIAN_POINT('Ctrl Pts',(-2.03783225496023,-1.,3.15102344775396));
#31910=CARTESIAN_POINT('Ctrl Pts',(-2.03984073791432,-1.,3.1538999167466));
#31911=CARTESIAN_POINT('Ctrl Pts',(-2.04297406404132,-1.,3.15817983946525));
#31912=CARTESIAN_POINT('Ctrl Pts',(-2.0469333124766,-1.,3.16343165059235));
#31913=CARTESIAN_POINT('Ctrl Pts',(-2.05151770247452,-1.,3.16936341689859));
#31914=CARTESIAN_POINT('Ctrl Pts',(-2.05650186773279,-1.,3.17564906975592));
#31915=CARTESIAN_POINT('Ctrl Pts',(-2.06166849827143,-1.,3.18197692964677));
#31916=CARTESIAN_POINT('Ctrl Pts',(-2.06684062744065,-1.,3.18809755562297));
#31917=CARTESIAN_POINT('Ctrl Pts',(-2.07192253497765,-1.,3.19388465568113));
#31918=CARTESIAN_POINT('Ctrl Pts',(-2.0769044187063,-1.,3.19934132835879));
#31919=CARTESIAN_POINT('Ctrl Pts',(-2.08182850370816,-1.,3.20454818630635));
#31920=CARTESIAN_POINT('Ctrl Pts',(-2.08676465517435,-1.,3.20962575845433));
#31921=CARTESIAN_POINT('Ctrl Pts',(-2.0917841946046,-1.,3.2146942960168));
#31922=CARTESIAN_POINT('Ctrl Pts',(-2.09692958434933,-1.,3.21982707347067));
#31923=CARTESIAN_POINT('Ctrl Pts',(-2.10220384298533,-1.,3.22503437553496));
#31924=CARTESIAN_POINT('Ctrl Pts',(-2.1075869964248,-1.,3.23028945793334));
#31925=CARTESIAN_POINT('Ctrl Pts',(-2.11304604021784,-1.,3.23554444767115));
#31926=CARTESIAN_POINT('Ctrl Pts',(-2.11854673326972,-1.,3.24074905517282));
#31927=CARTESIAN_POINT('Ctrl Pts',(-2.12406646410943,-1.,3.24587102613347));
#31928=CARTESIAN_POINT('Ctrl Pts',(-2.1296002839681,-1.,3.25090574493994));
#31929=CARTESIAN_POINT('Ctrl Pts',(-2.13515375878786,-1.,3.25586495065027));
#31930=CARTESIAN_POINT('Ctrl Pts',(-2.14073870754257,-1.,3.26077002641868));
#31931=CARTESIAN_POINT('Ctrl Pts',(-2.14636805295663,-1.,3.26564388189764));
#31932=CARTESIAN_POINT('Ctrl Pts',(-2.15205043199818,-1.,3.27050245897244));
#31933=CARTESIAN_POINT('Ctrl Pts',(-2.15778690038359,-1.,3.27534954469206));
#31934=CARTESIAN_POINT('Ctrl Pts',(-2.16357391934434,-1.,3.28018150841414));
#31935=CARTESIAN_POINT('Ctrl Pts',(-2.16940517773459,-1.,3.2849901997973));
#31936=CARTESIAN_POINT('Ctrl Pts',(-2.17527380048422,-1.,3.28976645712566));
#31937=CARTESIAN_POINT('Ctrl Pts',(-2.18117455557062,-1.,3.29450361500484));
#31938=CARTESIAN_POINT('Ctrl Pts',(-2.18710556500325,-1.,3.29920022557635));
#31939=CARTESIAN_POINT('Ctrl Pts',(-2.19306710376112,-1.,3.30385816281831));
#31940=CARTESIAN_POINT('Ctrl Pts',(-2.19906078949924,-1.,3.30848134694596));
#31941=CARTESIAN_POINT('Ctrl Pts',(-2.20508863150608,-1.,3.3130742460895));
#31942=CARTESIAN_POINT('Ctrl Pts',(-2.21115211847872,-1.,3.31764044024231));
#31943=CARTESIAN_POINT('Ctrl Pts',(-2.21725135110889,-1.,3.32218125618955));
#31944=CARTESIAN_POINT('Ctrl Pts',(-2.22338548312758,-1.,3.32669646722871));
#31945=CARTESIAN_POINT('Ctrl Pts',(-2.22955308907221,-1.,3.33118487773593));
#31946=CARTESIAN_POINT('Ctrl Pts',(-2.2357525632881,-1.,3.33564495756478));
#31947=CARTESIAN_POINT('Ctrl Pts',(-2.24198249391437,-1.,3.34007543738044));
#31948=CARTESIAN_POINT('Ctrl Pts',(-2.24824207678288,-1.,3.34447596770768));
#31949=CARTESIAN_POINT('Ctrl Pts',(-2.25453097693524,-1.,3.34884690292342));
#31950=CARTESIAN_POINT('Ctrl Pts',(-2.26084915222484,-1.,3.35318902552676));
#31951=CARTESIAN_POINT('Ctrl Pts',(-2.26719668579921,-1.,3.35750328523077));
#31952=CARTESIAN_POINT('Ctrl Pts',(-2.27357362620902,-1.,3.36179055004369));
#31953=CARTESIAN_POINT('Ctrl Pts',(-2.27997979457968,-1.,3.36605130712978));
#31954=CARTESIAN_POINT('Ctrl Pts',(-2.28641481081045,-1.,3.37028570206357));
#31955=CARTESIAN_POINT('Ctrl Pts',(-2.2928781800731,-1.,3.37449367172707));
#31956=CARTESIAN_POINT('Ctrl Pts',(-2.29936936127588,-1.,3.37867504959382));
#31957=CARTESIAN_POINT('Ctrl Pts',(-2.30588783640389,-1.,3.38282967336676));
#31958=CARTESIAN_POINT('Ctrl Pts',(-2.31243319489505,-1.,3.38695751492659));
#31959=CARTESIAN_POINT('Ctrl Pts',(-2.31900513925627,-1.,3.39105869475112));
#31960=CARTESIAN_POINT('Ctrl Pts',(-2.32560343902683,-1.,3.39513342020045));
#31961=CARTESIAN_POINT('Ctrl Pts',(-2.33222789882601,-1.,3.39918194578115));
#31962=CARTESIAN_POINT('Ctrl Pts',(-2.33887832342715,-1.,3.40320452776646));
#31963=CARTESIAN_POINT('Ctrl Pts',(-2.34555447648901,-1.,3.40720137403888));
#31964=CARTESIAN_POINT('Ctrl Pts',(-2.35225606823649,-1.,3.41117262313464));
#31965=CARTESIAN_POINT('Ctrl Pts',(-2.35898278606449,-1.,3.4151183675076));
#31966=CARTESIAN_POINT('Ctrl Pts',(-2.36573431470314,-1.,3.41903866635384));
#31967=CARTESIAN_POINT('Ctrl Pts',(-2.37251035954351,-1.,3.42293356216595));
#31968=CARTESIAN_POINT('Ctrl Pts',(-2.37931067029517,-1.,3.42680309755241));
#31969=CARTESIAN_POINT('Ctrl Pts',(-2.38613505844641,-1.,3.43064732714472));
#31970=CARTESIAN_POINT('Ctrl Pts',(-2.39298338805823,-1.,3.43446630680436));
#31971=CARTESIAN_POINT('Ctrl Pts',(-2.39848113411429,-1.,3.43750133066036));
#31972=CARTESIAN_POINT('Ctrl Pts',(-2.40261515590099,-1.,3.43976627485223));
#31973=CARTESIAN_POINT('Ctrl Pts',(-2.40537592959345,-1.,3.44127120683402));
#31974=CARTESIAN_POINT('Ctrl Pts',(-2.40675750623143,-1.,3.44202241512147));
#31975=CARTESIAN_POINT('',(-2.52982887637028,-1.,3.35260583073571));
#31976=CARTESIAN_POINT('',(-2.40675750623143,-1.,3.44202241512147));
#31977=CARTESIAN_POINT('',(-2.36531447826073,-1.,2.90994629141676));
#31978=CARTESIAN_POINT('Ctrl Pts',(-2.52982887637028,-1.,3.35260583073571));
#31979=CARTESIAN_POINT('Ctrl Pts',(-2.5295413654909,-1.,3.35105973714071));
#31980=CARTESIAN_POINT('Ctrl Pts',(-2.52896321610703,-1.,3.34796903576663));
#31981=CARTESIAN_POINT('Ctrl Pts',(-2.52808660915689,-1.,3.34333744115511));
#31982=CARTESIAN_POINT('Ctrl Pts',(-2.52689902690158,-1.,3.33717089999103));
#31983=CARTESIAN_POINT('Ctrl Pts',(-2.52538321164634,-1.,3.32947762187533));
#31984=CARTESIAN_POINT('Ctrl Pts',(-2.5238359839626,-1.,3.32179931078699));
#31985=CARTESIAN_POINT('Ctrl Pts',(-2.52225724871313,-1.,3.31413607874645));
#31986=CARTESIAN_POINT('Ctrl Pts',(-2.52064689568511,-1.,3.30648808815442));
#31987=CARTESIAN_POINT('Ctrl Pts',(-2.51900480701069,-1.,3.29885556388352));
#31988=CARTESIAN_POINT('Ctrl Pts',(-2.51733085123797,-1.,3.2912387729927));
#31989=CARTESIAN_POINT('Ctrl Pts',(-2.51562487464514,-1.,3.28363799702982));
#31990=CARTESIAN_POINT('Ctrl Pts',(-2.513886692704,-1.,3.27605350473142));
#31991=CARTESIAN_POINT('Ctrl Pts',(-2.51211608411423,-1.,3.26848552888115));
#31992=CARTESIAN_POINT('Ctrl Pts',(-2.51031277813486,-1.,3.26093423001434));
#31993=CARTESIAN_POINT('Ctrl Pts',(-2.50847647070723,-1.,3.25339971460982));
#31994=CARTESIAN_POINT('Ctrl Pts',(-2.506606859405,-1.,3.24588208983849));
#31995=CARTESIAN_POINT('Ctrl Pts',(-2.5047036758003,-1.,3.23838151080319));
#31996=CARTESIAN_POINT('Ctrl Pts',(-2.50276671338111,-1.,3.23089822320646));
#31997=CARTESIAN_POINT('Ctrl Pts',(-2.50079587201957,-1.,3.22343262620503));
#31998=CARTESIAN_POINT('Ctrl Pts',(-2.4987911459939,-1.,3.21598526261286));
#31999=CARTESIAN_POINT('Ctrl Pts',(-2.4967525264737,-1.,3.20855669849836));
#32000=CARTESIAN_POINT('Ctrl Pts',(-2.49467992057755,-1.,3.20114742397588));
#32001=CARTESIAN_POINT('Ctrl Pts',(-2.49257307239848,-1.,3.19375775555798));
#32002=CARTESIAN_POINT('Ctrl Pts',(-2.49043146334059,-1.,3.18638771282266));
#32003=CARTESIAN_POINT('Ctrl Pts',(-2.48825428288201,-1.,3.17903698136622));
#32004=CARTESIAN_POINT('Ctrl Pts',(-2.48604065348587,-1.,3.17170518863313));
#32005=CARTESIAN_POINT('Ctrl Pts',(-2.48378981792725,-1.,3.16439213290161));
#32006=CARTESIAN_POINT('Ctrl Pts',(-2.48150133566571,-1.,3.15709802322739));
#32007=CARTESIAN_POINT('Ctrl Pts',(-2.47917529057029,-1.,3.14982373241352));
#32008=CARTESIAN_POINT('Ctrl Pts',(-2.47681245356109,-1.,3.1425709954655));
#32009=CARTESIAN_POINT('Ctrl Pts',(-2.47441378371932,-1.,3.13534181229295));
#32010=CARTESIAN_POINT('Ctrl Pts',(-2.47197997765871,-1.,3.12813790805952));
#32011=CARTESIAN_POINT('Ctrl Pts',(-2.46951098947469,-1.,3.12096015766983));
#32012=CARTESIAN_POINT('Ctrl Pts',(-2.46700558843506,-1.,3.11380805536122));
#32013=CARTESIAN_POINT('Ctrl Pts',(-2.46446082979646,-1.,3.1066790790198));
#32014=CARTESIAN_POINT('Ctrl Pts',(-2.46187308501884,-1.,3.09956993697052));
#32015=CARTESIAN_POINT('Ctrl Pts',(-2.4592391256388,-1.,3.09247787931887));
#32016=CARTESIAN_POINT('Ctrl Pts',(-2.45655725437039,-1.,3.08540206545315));
#32017=CARTESIAN_POINT('Ctrl Pts',(-2.4538282678779,-1.,3.07834472886139));
#32018=CARTESIAN_POINT('Ctrl Pts',(-2.45105688854422,-1.,3.07131290521297));
#32019=CARTESIAN_POINT('Ctrl Pts',(-2.44824970516544,-1.,3.06431596421405));
#32020=CARTESIAN_POINT('Ctrl Pts',(-2.44541251892556,-1.,3.05736242671506));
#32021=CARTESIAN_POINT('Ctrl Pts',(-2.44254768923105,-1.,3.05045678021504));
#32022=CARTESIAN_POINT('Ctrl Pts',(-2.43965194061857,-1.,3.04359685040555));
#32023=CARTESIAN_POINT('Ctrl Pts',(-2.43671278042414,-1.,3.03676949672821));
#32024=CARTESIAN_POINT('Ctrl Pts',(-2.43371241361488,-1.,3.02995534946978));
#32025=CARTESIAN_POINT('Ctrl Pts',(-2.43063415586637,-1.,3.02313656036004));
#32026=CARTESIAN_POINT('Ctrl Pts',(-2.42746856264168,-1.,3.01630420830504));
#32027=CARTESIAN_POINT('Ctrl Pts',(-2.42421849439613,-1.,3.00946442616658));
#32028=CARTESIAN_POINT('Ctrl Pts',(-2.42090763946779,-1.,3.00264868585996));
#32029=CARTESIAN_POINT('Ctrl Pts',(-2.41757324500514,-1.,2.99590509293503));
#32030=CARTESIAN_POINT('Ctrl Pts',(-2.41425064199586,-1.,2.98927983005796));
#32031=CARTESIAN_POINT('Ctrl Pts',(-2.41095909342571,-1.,2.98280015815107));
#32032=CARTESIAN_POINT('Ctrl Pts',(-2.40768975073713,-1.,2.97646002822422));
#32033=CARTESIAN_POINT('Ctrl Pts',(-2.40438604734919,-1.,2.9701964131236));
#32034=CARTESIAN_POINT('Ctrl Pts',(-2.4009556571164,-1.,2.96390432240312));
#32035=CARTESIAN_POINT('Ctrl Pts',(-2.39730553974517,-1.,2.95748006482942));
#32036=CARTESIAN_POINT('Ctrl Pts',(-2.39337207631667,-1.,2.95085857128439));
#32037=CARTESIAN_POINT('Ctrl Pts',(-2.38914929090759,-1.,2.94404820669076));
#32038=CARTESIAN_POINT('Ctrl Pts',(-2.38472771516311,-1.,2.93717903280391));
#32039=CARTESIAN_POINT('Ctrl Pts',(-2.38028989582073,-1.,2.93049643640206));
#32040=CARTESIAN_POINT('Ctrl Pts',(-2.3760651052403,-1.,2.92430340582608));
#32041=CARTESIAN_POINT('Ctrl Pts',(-2.37229381109821,-1.,2.91891503791411));
#32042=CARTESIAN_POINT('Ctrl Pts',(-2.36919161373173,-1.,2.9146124988314));
#32043=CARTESIAN_POINT('Ctrl Pts',(-2.36707658451664,-1.,2.91181344022549));
#32044=CARTESIAN_POINT('Ctrl Pts',(-2.36599991765749,-1.,2.91051690822156));
#32045=CARTESIAN_POINT('Ctrl Pts',(-2.36553202948613,-1.,2.91005770527719));
#32046=CARTESIAN_POINT('Ctrl Pts',(-2.36536211188453,-1.,2.90995756655606));
#32047=CARTESIAN_POINT('Ctrl Pts',(-2.36531447826074,-1.,2.90994629141676));
#32048=CARTESIAN_POINT('',(-2.50410331873042,-1.,2.79140942341378));
#32049=CARTESIAN_POINT('Origin',(0.,-1.,0.));
#32050=CARTESIAN_POINT('',(-2.91557726271063,-1.,3.02314558451372));
#32051=CARTESIAN_POINT('Ctrl Pts',(-2.50410331873042,-1.,2.79140942341378));
#32052=CARTESIAN_POINT('Ctrl Pts',(-2.50410700351426,-1.,2.79145823440899));
#32053=CARTESIAN_POINT('Ctrl Pts',(-2.50417932839343,-1.,2.79164172519039));
#32054=CARTESIAN_POINT('Ctrl Pts',(-2.50455968395235,-1.,2.79217568804874));
#32055=CARTESIAN_POINT('Ctrl Pts',(-2.50567182569153,-1.,2.79344192164204));
#32056=CARTESIAN_POINT('Ctrl Pts',(-2.50810555977564,-1.,2.7959687805717));
#32057=CARTESIAN_POINT('Ctrl Pts',(-2.51186983687947,-1.,2.79970585014308));
#32058=CARTESIAN_POINT('Ctrl Pts',(-2.51660190466067,-1.,2.80427363984939));
#32059=CARTESIAN_POINT('Ctrl Pts',(-2.52205778589922,-1.,2.80941521967234));
#32060=CARTESIAN_POINT('Ctrl Pts',(-2.52796388055457,-1.,2.8148437904867));
#32061=CARTESIAN_POINT('Ctrl Pts',(-2.53405679667463,-1.,2.82028550483744));
#32062=CARTESIAN_POINT('Ctrl Pts',(-2.54012272520141,-1.,2.82552167649157));
#32063=CARTESIAN_POINT('Ctrl Pts',(-2.54604736792542,-1.,2.83044254225794));
#32064=CARTESIAN_POINT('Ctrl Pts',(-2.55182152806964,-1.,2.83505269592412));
#32065=CARTESIAN_POINT('Ctrl Pts',(-2.55749952145165,-1.,2.83942515220699));
#32066=CARTESIAN_POINT('Ctrl Pts',(-2.56316920798489,-1.,2.84366802680211));
#32067=CARTESIAN_POINT('Ctrl Pts',(-2.56891984251743,-1.,2.84788893329091));
#32068=CARTESIAN_POINT('Ctrl Pts',(-2.57480482727128,-1.,2.85215360144483));
#32069=CARTESIAN_POINT('Ctrl Pts',(-2.58082875254407,-1.,2.85647171715147));
#32070=CARTESIAN_POINT('Ctrl Pts',(-2.5869677064356,-1.,2.86081999003668));
#32071=CARTESIAN_POINT('Ctrl Pts',(-2.59318160184921,-1.,2.86515629953528));
#32072=CARTESIAN_POINT('Ctrl Pts',(-2.59942875223202,-1.,2.86943633170712));
#32073=CARTESIAN_POINT('Ctrl Pts',(-2.6056817788128,-1.,2.87363176656475));
#32074=CARTESIAN_POINT('Ctrl Pts',(-2.61193507170928,-1.,2.87773881947885));
#32075=CARTESIAN_POINT('Ctrl Pts',(-2.61819596473087,-1.,2.88176821427502));
#32076=CARTESIAN_POINT('Ctrl Pts',(-2.62447947640253,-1.,2.88573922195049));
#32077=CARTESIAN_POINT('Ctrl Pts',(-2.63080195420771,-1.,2.88967244854243));
#32078=CARTESIAN_POINT('Ctrl Pts',(-2.63717442263944,-1.,2.89358228854557));
#32079=CARTESIAN_POINT('Ctrl Pts',(-2.64359851684146,-1.,2.89747231723361));
#32080=CARTESIAN_POINT('Ctrl Pts',(-2.65007017365576,-1.,2.90133950224879));
#32081=CARTESIAN_POINT('Ctrl Pts',(-2.65658188464287,-1.,2.90517678087467));
#32082=CARTESIAN_POINT('Ctrl Pts',(-2.66312542616809,-1.,2.90897617968921));
#32083=CARTESIAN_POINT('Ctrl Pts',(-2.66969458792627,-1.,2.91273193382876));
#32084=CARTESIAN_POINT('Ctrl Pts',(-2.67628728855309,-1.,2.91644290704281));
#32085=CARTESIAN_POINT('Ctrl Pts',(-2.68290409279689,-1.,2.92011090722152));
#32086=CARTESIAN_POINT('Ctrl Pts',(-2.68954721165342,-1.,2.92373955325876));
#32087=CARTESIAN_POINT('Ctrl Pts',(-2.69621932864302,-1.,2.92733294395268));
#32088=CARTESIAN_POINT('Ctrl Pts',(-2.70292247416881,-1.,2.93089438233746));
#32089=CARTESIAN_POINT('Ctrl Pts',(-2.70965695523776,-1.,2.93442516311168));
#32090=CARTESIAN_POINT('Ctrl Pts',(-2.71642190053575,-1.,2.93792519474955));
#32091=CARTESIAN_POINT('Ctrl Pts',(-2.72321571511322,-1.,2.94139351933882));
#32092=CARTESIAN_POINT('Ctrl Pts',(-2.73003657371613,-1.,2.94482887675139));
#32093=CARTESIAN_POINT('Ctrl Pts',(-2.73688288329825,-1.,2.94823023414381));
#32094=CARTESIAN_POINT('Ctrl Pts',(-2.7437537949221,-1.,2.95159737214305));
#32095=CARTESIAN_POINT('Ctrl Pts',(-2.75064903318996,-1.,2.95493069316211));
#32096=CARTESIAN_POINT('Ctrl Pts',(-2.75756867888393,-1.,2.9582309766594));
#32097=CARTESIAN_POINT('Ctrl Pts',(-2.76451296269571,-1.,2.96149914764832));
#32098=CARTESIAN_POINT('Ctrl Pts',(-2.77148206836464,-1.,2.96473605585548));
#32099=CARTESIAN_POINT('Ctrl Pts',(-2.77847589542767,-1.,2.9679422104295));
#32100=CARTESIAN_POINT('Ctrl Pts',(-2.78549409123657,-1.,2.97111781461349));
#32101=CARTESIAN_POINT('Ctrl Pts',(-2.79253615718147,-1.,2.97426288347475));
#32102=CARTESIAN_POINT('Ctrl Pts',(-2.79960153278186,-1.,2.97737733718242));
#32103=CARTESIAN_POINT('Ctrl Pts',(-2.80668968101162,-1.,2.98046109647299));
#32104=CARTESIAN_POINT('Ctrl Pts',(-2.81380019196454,-1.,2.9835141977994));
#32105=CARTESIAN_POINT('Ctrl Pts',(-2.82093279065704,-1.,2.98653680669434));
#32106=CARTESIAN_POINT('Ctrl Pts',(-2.82808728190402,-1.,2.98952916401699));
#32107=CARTESIAN_POINT('Ctrl Pts',(-2.83526351254383,-1.,2.99249155170479));
#32108=CARTESIAN_POINT('Ctrl Pts',(-2.84246132984334,-1.,2.995424253416));
#32109=CARTESIAN_POINT('Ctrl Pts',(-2.84968053289104,-1.,2.99832751144566));
#32110=CARTESIAN_POINT('Ctrl Pts',(-2.85692085715129,-1.,3.0012015079552));
#32111=CARTESIAN_POINT('Ctrl Pts',(-2.86418200833065,-1.,3.00404638316245));
#32112=CARTESIAN_POINT('Ctrl Pts',(-2.87146368430104,-1.,3.00686224485374));
#32113=CARTESIAN_POINT('Ctrl Pts',(-2.87876560072799,-1.,3.0096491810855));
#32114=CARTESIAN_POINT('Ctrl Pts',(-2.88608751706796,-1.,3.01240727309568));
#32115=CARTESIAN_POINT('Ctrl Pts',(-2.8934292556764,-1.,3.01513660433291));
#32116=CARTESIAN_POINT('Ctrl Pts',(-2.90079069102661,-1.,3.01783725123646));
#32117=CARTESIAN_POINT('Ctrl Pts',(-2.90669553303902,-1.,3.01997487194926));
#32118=CARTESIAN_POINT('Ctrl Pts',(-2.91113297349052,-1.,3.02156522743299));
#32119=CARTESIAN_POINT('Ctrl Pts',(-2.91409518070707,-1.,3.02261975104912));
#32120=CARTESIAN_POINT('Ctrl Pts',(-2.91557726271063,-1.,3.02314558451372));
#32121=CARTESIAN_POINT('',(-3.02314558451372,-1.,2.91557726271063));
#32122=CARTESIAN_POINT('',(-2.91557726271063,-1.,3.02314558451372));
#32123=CARTESIAN_POINT('',(-2.79140942341258,-1.,2.50410331873176));
#32124=CARTESIAN_POINT('Ctrl Pts',(-3.02314558451372,-1.,2.91557726271063));
#32125=CARTESIAN_POINT('Ctrl Pts',(-3.02261975104593,-1.,2.91409518070399));
#32126=CARTESIAN_POINT('Ctrl Pts',(-3.02156522742431,-1.,2.91113297348212));
#32127=CARTESIAN_POINT('Ctrl Pts',(-3.01997487193503,-1.,2.90669553302526));
#32128=CARTESIAN_POINT('Ctrl Pts',(-3.01783725121981,-1.,2.9007906910105));
#32129=CARTESIAN_POINT('Ctrl Pts',(-3.01513660431928,-1.,2.89342925566321));
#32130=CARTESIAN_POINT('Ctrl Pts',(-3.01240727308829,-1.,2.8860875170608));
#32131=CARTESIAN_POINT('Ctrl Pts',(-3.00964918108476,-1.,2.87876560072727));
#32132=CARTESIAN_POINT('Ctrl Pts',(-3.00686224485784,-1.,2.87146368430502));
#32133=CARTESIAN_POINT('Ctrl Pts',(-3.00404638316867,-1.,2.86418200833667));
#32134=CARTESIAN_POINT('Ctrl Pts',(-3.00120150796095,-1.,2.85692085715686));
#32135=CARTESIAN_POINT('Ctrl Pts',(-2.99832751144925,-1.,2.84968053289451));
#32136=CARTESIAN_POINT('Ctrl Pts',(-2.99542425341685,-1.,2.84246132984415));
#32137=CARTESIAN_POINT('Ctrl Pts',(-2.9924915517034,-1.,2.83526351254248));
#32138=CARTESIAN_POINT('Ctrl Pts',(-2.98952916401446,-1.,2.82808728190157));
#32139=CARTESIAN_POINT('Ctrl Pts',(-2.9865368066918,-1.,2.82093279065457));
#32140=CARTESIAN_POINT('Ctrl Pts',(-2.98351419779767,-1.,2.81380019196286));
#32141=CARTESIAN_POINT('Ctrl Pts',(-2.98046109647241,-1.,2.80668968101106));
#32142=CARTESIAN_POINT('Ctrl Pts',(-2.97737733718287,-1.,2.7996015327823));
#32143=CARTESIAN_POINT('Ctrl Pts',(-2.9742628834758,-1.,2.79253615718248));
#32144=CARTESIAN_POINT('Ctrl Pts',(-2.97111781461465,-1.,2.78549409123769));
#32145=CARTESIAN_POINT('Ctrl Pts',(-2.96794221043036,-1.,2.7784758954285));
#32146=CARTESIAN_POINT('Ctrl Pts',(-2.96473605585583,-1.,2.77148206836498));
#32147=CARTESIAN_POINT('Ctrl Pts',(-2.96149914764818,-1.,2.76451296269557));
#32148=CARTESIAN_POINT('Ctrl Pts',(-2.95823097665896,-1.,2.7575686788835));
#32149=CARTESIAN_POINT('Ctrl Pts',(-2.95493069316161,-1.,2.75064903318947));
#32150=CARTESIAN_POINT('Ctrl Pts',(-2.95159737214266,-1.,2.74375379492172));
#32151=CARTESIAN_POINT('Ctrl Pts',(-2.94823023414364,-1.,2.73688288329808));
#32152=CARTESIAN_POINT('Ctrl Pts',(-2.94482887675143,-1.,2.73003657371617));
#32153=CARTESIAN_POINT('Ctrl Pts',(-2.94139351933897,-1.,2.72321571511337));
#32154=CARTESIAN_POINT('Ctrl Pts',(-2.93792519474972,-1.,2.71642190053592));
#32155=CARTESIAN_POINT('Ctrl Pts',(-2.93442516311179,-1.,2.70965695523787));
#32156=CARTESIAN_POINT('Ctrl Pts',(-2.9308943823375,-1.,2.70292247416885));
#32157=CARTESIAN_POINT('Ctrl Pts',(-2.92733294395267,-1.,2.69621932864301));
#32158=CARTESIAN_POINT('Ctrl Pts',(-2.92373955325875,-1.,2.68954721165339));
#32159=CARTESIAN_POINT('Ctrl Pts',(-2.92011090722152,-1.,2.68290409279688));
#32160=CARTESIAN_POINT('Ctrl Pts',(-2.91644290704285,-1.,2.67628728855312));
#32161=CARTESIAN_POINT('Ctrl Pts',(-2.91273193382882,-1.,2.66969458792631));
#32162=CARTESIAN_POINT('Ctrl Pts',(-2.90897617968923,-1.,2.6631254261681));
#32163=CARTESIAN_POINT('Ctrl Pts',(-2.90517678087461,-1.,2.65658188464282));
#32164=CARTESIAN_POINT('Ctrl Pts',(-2.90133950224867,-1.,2.65007017365564));
#32165=CARTESIAN_POINT('Ctrl Pts',(-2.89747231723345,-1.,2.64359851684131));
#32166=CARTESIAN_POINT('Ctrl Pts',(-2.89358228854544,-1.,2.63717442263932));
#32167=CARTESIAN_POINT('Ctrl Pts',(-2.88967244854239,-1.,2.63080195420767));
#32168=CARTESIAN_POINT('Ctrl Pts',(-2.88573922195059,-1.,2.62447947640262));
#32169=CARTESIAN_POINT('Ctrl Pts',(-2.88176821427525,-1.,2.61819596473108));
#32170=CARTESIAN_POINT('Ctrl Pts',(-2.87773881947916,-1.,2.61193507170955));
#32171=CARTESIAN_POINT('Ctrl Pts',(-2.87363176656501,-1.,2.60568177881303));
#32172=CARTESIAN_POINT('Ctrl Pts',(-2.86943633170722,-1.,2.5994287522321));
#32173=CARTESIAN_POINT('Ctrl Pts',(-2.86515629953513,-1.,2.59318160184908));
#32174=CARTESIAN_POINT('Ctrl Pts',(-2.86081999003629,-1.,2.58696770643524));
#32175=CARTESIAN_POINT('Ctrl Pts',(-2.85647171715092,-1.,2.58082875254357));
#32176=CARTESIAN_POINT('Ctrl Pts',(-2.85215360144431,-1.,2.57480482727081));
#32177=CARTESIAN_POINT('Ctrl Pts',(-2.84788893329067,-1.,2.56891984251721));
#32178=CARTESIAN_POINT('Ctrl Pts',(-2.84366802680237,-1.,2.56316920798513));
#32179=CARTESIAN_POINT('Ctrl Pts',(-2.83942515220782,-1.,2.55749952145241));
#32180=CARTESIAN_POINT('Ctrl Pts',(-2.83505269592536,-1.,2.55182152807077));
#32181=CARTESIAN_POINT('Ctrl Pts',(-2.83044254225917,-1.,2.54604736792655));
#32182=CARTESIAN_POINT('Ctrl Pts',(-2.8255216764922,-1.,2.54012272520199));
#32183=CARTESIAN_POINT('Ctrl Pts',(-2.82028550483689,-1.,2.53405679667412));
#32184=CARTESIAN_POINT('Ctrl Pts',(-2.81484379048475,-1.,2.52796388055278));
#32185=CARTESIAN_POINT('Ctrl Pts',(-2.80941521966941,-1.,2.52205778589653));
#32186=CARTESIAN_POINT('Ctrl Pts',(-2.80427363984653,-1.,2.51660190465805));
#32187=CARTESIAN_POINT('Ctrl Pts',(-2.79970585014168,-1.,2.51186983687818));
#32188=CARTESIAN_POINT('Ctrl Pts',(-2.79596878057287,-1.,2.50810555977671));
#32189=CARTESIAN_POINT('Ctrl Pts',(-2.79344192164147,-1.,2.50567182569081));
#32190=CARTESIAN_POINT('Ctrl Pts',(-2.79217568804755,-1.,2.50455968395146));
#32191=CARTESIAN_POINT('Ctrl Pts',(-2.79164172518905,-1.,2.50417932839313));
#32192=CARTESIAN_POINT('Ctrl Pts',(-2.79145823440781,-1.,2.50410700351493));
#32193=CARTESIAN_POINT('Ctrl Pts',(-2.79140942341258,-1.,2.50410331873176));
#32194=CARTESIAN_POINT('',(-2.90994629141562,-1.,2.36531447826213));
#32195=CARTESIAN_POINT('Origin',(0.,-1.,0.));
#32196=CARTESIAN_POINT('',(-3.35260583073571,-1.,2.52982887637028));
#32197=CARTESIAN_POINT('Ctrl Pts',(-2.90994629141562,-1.,2.36531447826213));
#32198=CARTESIAN_POINT('Ctrl Pts',(-2.90995756655558,-1.,2.3653621118858));
#32199=CARTESIAN_POINT('Ctrl Pts',(-2.9100577052777,-1.,2.36553202948741));
#32200=CARTESIAN_POINT('Ctrl Pts',(-2.91051690822262,-1.,2.36599991765853));
#32201=CARTESIAN_POINT('Ctrl Pts',(-2.91181344022628,-1.,2.36707658451709));
#32202=CARTESIAN_POINT('Ctrl Pts',(-2.91461249883016,-1.,2.36919161373074));
#32203=CARTESIAN_POINT('Ctrl Pts',(-2.9189150379156,-1.,2.37229381109939));
#32204=CARTESIAN_POINT('Ctrl Pts',(-2.92430340582912,-1.,2.37606510524271));
#32205=CARTESIAN_POINT('Ctrl Pts',(-2.93049643640517,-1.,2.3802898958232));
#32206=CARTESIAN_POINT('Ctrl Pts',(-2.93717903280599,-1.,2.38472771516476));
#32207=CARTESIAN_POINT('Ctrl Pts',(-2.94404820669135,-1.,2.38914929090806));
#32208=CARTESIAN_POINT('Ctrl Pts',(-2.95085857128372,-1.,2.39337207631613));
#32209=CARTESIAN_POINT('Ctrl Pts',(-2.95748006482811,-1.,2.39730553974412));
#32210=CARTESIAN_POINT('Ctrl Pts',(-2.96390432240181,-1.,2.40095565711535));
#32211=CARTESIAN_POINT('Ctrl Pts',(-2.97019641312272,-1.,2.40438604734848));
#32212=CARTESIAN_POINT('Ctrl Pts',(-2.97646002822395,-1.,2.40768975073691));
#32213=CARTESIAN_POINT('Ctrl Pts',(-2.98280015815132,-1.,2.41095909342591));
#32214=CARTESIAN_POINT('Ctrl Pts',(-2.98927983005851,-1.,2.4142506419963));
#32215=CARTESIAN_POINT('Ctrl Pts',(-2.99590509293561,-1.,2.4175732450056));
#32216=CARTESIAN_POINT('Ctrl Pts',(-3.00264868586038,-1.,2.42090763946812));
#32217=CARTESIAN_POINT('Ctrl Pts',(-3.00946442616674,-1.,2.42421849439625));
#32218=CARTESIAN_POINT('Ctrl Pts',(-3.01630420830494,-1.,2.4274685626416));
#32219=CARTESIAN_POINT('Ctrl Pts',(-3.02313656035977,-1.,2.43063415586615));
#32220=CARTESIAN_POINT('Ctrl Pts',(-3.02995534946946,-1.,2.43371241361462));
#32221=CARTESIAN_POINT('Ctrl Pts',(-3.03676949672797,-1.,2.43671278042394));
#32222=CARTESIAN_POINT('Ctrl Pts',(-3.04359685040545,-1.,2.43965194061849));
#32223=CARTESIAN_POINT('Ctrl Pts',(-3.05045678021509,-1.,2.44254768923109));
#32224=CARTESIAN_POINT('Ctrl Pts',(-3.05736242671521,-1.,2.44541251892568));
#32225=CARTESIAN_POINT('Ctrl Pts',(-3.06431596421422,-1.,2.44824970516558));
#32226=CARTESIAN_POINT('Ctrl Pts',(-3.0713129052131,-1.,2.45105688854432));
#32227=CARTESIAN_POINT('Ctrl Pts',(-3.07834472886145,-1.,2.45382826787795));
#32228=CARTESIAN_POINT('Ctrl Pts',(-3.08540206545313,-1.,2.45655725437037));
#32229=CARTESIAN_POINT('Ctrl Pts',(-3.09247787931881,-1.,2.45923912563875));
#32230=CARTESIAN_POINT('Ctrl Pts',(-3.09956993697048,-1.,2.4618730850188));
#32231=CARTESIAN_POINT('Ctrl Pts',(-3.10667907901981,-1.,2.46446082979645));
#32232=CARTESIAN_POINT('Ctrl Pts',(-3.11380805536124,-1.,2.46700558843507));
#32233=CARTESIAN_POINT('Ctrl Pts',(-3.12096015766984,-1.,2.4695109894747));
#32234=CARTESIAN_POINT('Ctrl Pts',(-3.12813790805948,-1.,2.47197997765868));
#32235=CARTESIAN_POINT('Ctrl Pts',(-3.13534181229282,-1.,2.47441378371923));
#32236=CARTESIAN_POINT('Ctrl Pts',(-3.14257099546531,-1.,2.47681245356095));
#32237=CARTESIAN_POINT('Ctrl Pts',(-3.14982373241335,-1.,2.47917529057016));
#32238=CARTESIAN_POINT('Ctrl Pts',(-3.15709802322735,-1.,2.48150133566568));
#32239=CARTESIAN_POINT('Ctrl Pts',(-3.16439213290181,-1.,2.48378981792739));
#32240=CARTESIAN_POINT('Ctrl Pts',(-3.17170518863357,-1.,2.48604065348619));
#32241=CARTESIAN_POINT('Ctrl Pts',(-3.17903698136679,-1.,2.48825428288243));
#32242=CARTESIAN_POINT('Ctrl Pts',(-3.18638771282315,-1.,2.49043146334095));
#32243=CARTESIAN_POINT('Ctrl Pts',(-3.19375775555814,-1.,2.4925730723986));
#32244=CARTESIAN_POINT('Ctrl Pts',(-3.20114742397549,-1.,2.49467992057726));
#32245=CARTESIAN_POINT('Ctrl Pts',(-3.2085566984974,-1.,2.49675252647298));
#32246=CARTESIAN_POINT('Ctrl Pts',(-3.21598526261157,-1.,2.49879114599293));
#32247=CARTESIAN_POINT('Ctrl Pts',(-3.22343262620387,-1.,2.5007958720187));
#32248=CARTESIAN_POINT('Ctrl Pts',(-3.23089822320596,-1.,2.50276671338074));
#32249=CARTESIAN_POINT('Ctrl Pts',(-3.23838151080383,-1.,2.50470367580078));
#32250=CARTESIAN_POINT('Ctrl Pts',(-3.24588208984042,-1.,2.50660685940645));
#32251=CARTESIAN_POINT('Ctrl Pts',(-3.25339971461265,-1.,2.50847647070936));
#32252=CARTESIAN_POINT('Ctrl Pts',(-3.26093423001716,-1.,2.51031277813697));
#32253=CARTESIAN_POINT('Ctrl Pts',(-3.26848552888271,-1.,2.51211608411539));
#32254=CARTESIAN_POINT('Ctrl Pts',(-3.27605350473048,-1.,2.51388669270329));
#32255=CARTESIAN_POINT('Ctrl Pts',(-3.28363799702583,-1.,2.51562487464215));
#32256=CARTESIAN_POINT('Ctrl Pts',(-3.2912387729863,-1.,2.51733085123316));
#32257=CARTESIAN_POINT('Ctrl Pts',(-3.29885556387661,-1.,2.51900480700548));
#32258=CARTESIAN_POINT('Ctrl Pts',(-3.30648808814986,-1.,2.52064689568167));
#32259=CARTESIAN_POINT('Ctrl Pts',(-3.31413607874727,-1.,2.52225724871375));
#32260=CARTESIAN_POINT('Ctrl Pts',(-3.32179931079521,-1.,2.52383598396878));
#32261=CARTESIAN_POINT('Ctrl Pts',(-3.32947762189049,-1.,2.52538321165774));
#32262=CARTESIAN_POINT('Ctrl Pts',(-3.33717090000955,-1.,2.52689902691551));
#32263=CARTESIAN_POINT('Ctrl Pts',(-3.34333744117093,-1.,2.52808660916879));
#32264=CARTESIAN_POINT('Ctrl Pts',(-3.34796903577628,-1.,2.5289632161143));
#32265=CARTESIAN_POINT('Ctrl Pts',(-3.35105973714426,-1.,2.52954136549357));
#32266=CARTESIAN_POINT('Ctrl Pts',(-3.35260583073571,-1.,2.52982887637028));
#32267=CARTESIAN_POINT('',(-3.44202241512147,-1.,2.40675750623143));
#32268=CARTESIAN_POINT('',(-3.35260583073571,-1.,2.52982887637028));
#32269=CARTESIAN_POINT('',(-3.14877060440327,-1.,2.03660101169715));
#32270=CARTESIAN_POINT('Ctrl Pts',(-3.44202241512147,-1.,2.40675750623143));
#32271=CARTESIAN_POINT('Ctrl Pts',(-3.44127120683039,-1.,2.4053759295909));
#32272=CARTESIAN_POINT('Ctrl Pts',(-3.43976627484234,-1.,2.40261515589405));
#32273=CARTESIAN_POINT('Ctrl Pts',(-3.43750133064416,-1.,2.39848113410292));
#32274=CARTESIAN_POINT('Ctrl Pts',(-3.4344663067854,-1.,2.39298338804493));
#32275=CARTESIAN_POINT('Ctrl Pts',(-3.4306473271292,-1.,2.38613505843552));
#32276=CARTESIAN_POINT('Ctrl Pts',(-3.42680309754399,-1.,2.37931067028926));
#32277=CARTESIAN_POINT('Ctrl Pts',(-3.42293356216511,-1.,2.37251035954292));
#32278=CARTESIAN_POINT('Ctrl Pts',(-3.41903866635852,-1.,2.36573431470642));
#32279=CARTESIAN_POINT('Ctrl Pts',(-3.41511836751469,-1.,2.35898278606946));
#32280=CARTESIAN_POINT('Ctrl Pts',(-3.41117262314119,-1.,2.35225606824109));
#32281=CARTESIAN_POINT('Ctrl Pts',(-3.40720137404297,-1.,2.34555447649188));
#32282=CARTESIAN_POINT('Ctrl Pts',(-3.40320452776743,-1.,2.33887832342782));
#32283=CARTESIAN_POINT('Ctrl Pts',(-3.39918194577956,-1.,2.33222789882489));
#32284=CARTESIAN_POINT('Ctrl Pts',(-3.39513342019756,-1.,2.3256034390248));
#32285=CARTESIAN_POINT('Ctrl Pts',(-3.39105869474822,-1.,2.31900513925424));
#32286=CARTESIAN_POINT('Ctrl Pts',(-3.38695751492462,-1.,2.31243319489367));
#32287=CARTESIAN_POINT('Ctrl Pts',(-3.3828296733661,-1.,2.30588783640343));
#32288=CARTESIAN_POINT('Ctrl Pts',(-3.37867504959433,-1.,2.29936936127624));
#32289=CARTESIAN_POINT('Ctrl Pts',(-3.37449367172826,-1.,2.29287818007393));
#32290=CARTESIAN_POINT('Ctrl Pts',(-3.37028570206488,-1.,2.28641481081137));
#32291=CARTESIAN_POINT('Ctrl Pts',(-3.36605130713076,-1.,2.27997979458037));
#32292=CARTESIAN_POINT('Ctrl Pts',(-3.36179055004409,-1.,2.2735736262093));
#32293=CARTESIAN_POINT('Ctrl Pts',(-3.35750328523061,-1.,2.2671966857991));
#32294=CARTESIAN_POINT('Ctrl Pts',(-3.35318902552626,-1.,2.26084915222449));
#32295=CARTESIAN_POINT('Ctrl Pts',(-3.34884690292285,-1.,2.25453097693483));
#32296=CARTESIAN_POINT('Ctrl Pts',(-3.34447596770723,-1.,2.24824207678256));
#32297=CARTESIAN_POINT('Ctrl Pts',(-3.34007543738025,-1.,2.24198249391422));
#32298=CARTESIAN_POINT('Ctrl Pts',(-3.33564495756482,-1.,2.23575256328812));
#32299=CARTESIAN_POINT('Ctrl Pts',(-3.33118487773611,-1.,2.22955308907233));
#32300=CARTESIAN_POINT('Ctrl Pts',(-3.3266964672289,-1.,2.22338548312772));
#32301=CARTESIAN_POINT('Ctrl Pts',(-3.32218125618968,-1.,2.21725135110898));
#32302=CARTESIAN_POINT('Ctrl Pts',(-3.31764044024235,-1.,2.21115211847875));
#32303=CARTESIAN_POINT('Ctrl Pts',(-3.31307424608949,-1.,2.20508863150607));
#32304=CARTESIAN_POINT('Ctrl Pts',(-3.30848134694595,-1.,2.19906078949923));
#32305=CARTESIAN_POINT('Ctrl Pts',(-3.30385816281831,-1.,2.19306710376111));
#32306=CARTESIAN_POINT('Ctrl Pts',(-3.29920022557639,-1.,2.18710556500327));
#32307=CARTESIAN_POINT('Ctrl Pts',(-3.2945036150049,-1.,2.18117455557065));
#32308=CARTESIAN_POINT('Ctrl Pts',(-3.28976645712568,-1.,2.17527380048423));
#32309=CARTESIAN_POINT('Ctrl Pts',(-3.28499019979724,-1.,2.16940517773455));
#32310=CARTESIAN_POINT('Ctrl Pts',(-3.280181508414,-1.,2.16357391934425));
#32311=CARTESIAN_POINT('Ctrl Pts',(-3.27534954469187,-1.,2.15778690038347));
#32312=CARTESIAN_POINT('Ctrl Pts',(-3.27050245897228,-1.,2.15205043199808));
#32313=CARTESIAN_POINT('Ctrl Pts',(-3.26564388189759,-1.,2.1463680529566));
#32314=CARTESIAN_POINT('Ctrl Pts',(-3.26077002641879,-1.,2.14073870754264));
#32315=CARTESIAN_POINT('Ctrl Pts',(-3.25586495065054,-1.,2.13515375878803));
#32316=CARTESIAN_POINT('Ctrl Pts',(-3.25090574494028,-1.,2.12960028396832));
#32317=CARTESIAN_POINT('Ctrl Pts',(-3.24587102613376,-1.,2.12406646410962));
#32318=CARTESIAN_POINT('Ctrl Pts',(-3.24074905517293,-1.,2.11854673326979));
#32319=CARTESIAN_POINT('Ctrl Pts',(-3.23554444767099,-1.,2.11304604021773));
#32320=CARTESIAN_POINT('Ctrl Pts',(-3.23028945793289,-1.,2.10758699642451));
#32321=CARTESIAN_POINT('Ctrl Pts',(-3.22503437553434,-1.,2.10220384298492));
#32322=CARTESIAN_POINT('Ctrl Pts',(-3.21982707347009,-1.,2.09692958434895));
#32323=CARTESIAN_POINT('Ctrl Pts',(-3.21469429601654,-1.,2.09178419460443));
#32324=CARTESIAN_POINT('Ctrl Pts',(-3.20962575845463,-1.,2.08676465517455));
#32325=CARTESIAN_POINT('Ctrl Pts',(-3.2045481863073,-1.,2.08182850370878));
#32326=CARTESIAN_POINT('Ctrl Pts',(-3.19934132836019,-1.,2.07690441870722));
#32327=CARTESIAN_POINT('Ctrl Pts',(-3.19388465568252,-1.,2.07192253497857));
#32328=CARTESIAN_POINT('Ctrl Pts',(-3.18809755562368,-1.,2.06684062744112));
#32329=CARTESIAN_POINT('Ctrl Pts',(-3.18197692964614,-1.,2.06166849827101));
#32330=CARTESIAN_POINT('Ctrl Pts',(-3.17564906975371,-1.,2.05650186773132));
#32331=CARTESIAN_POINT('Ctrl Pts',(-3.16936341689527,-1.,2.05151770247233));
#32332=CARTESIAN_POINT('Ctrl Pts',(-3.16343165058912,-1.,2.04693331247446));
#32333=CARTESIAN_POINT('Ctrl Pts',(-3.15817983946367,-1.,2.04297406404027));
#32334=CARTESIAN_POINT('Ctrl Pts',(-3.15389991674792,-1.,2.03984073791519));
#32335=CARTESIAN_POINT('Ctrl Pts',(-3.15102344775328,-1.,2.03783225495961));
#32336=CARTESIAN_POINT('Ctrl Pts',(-3.14959882629805,-1.,2.03693188810544));
#32337=CARTESIAN_POINT('Ctrl Pts',(-3.1490119366901,-1.,2.03663974554932));
#32338=CARTESIAN_POINT('Ctrl Pts',(-3.14881939088124,-1.,2.03659701539259));
#32339=CARTESIAN_POINT('Ctrl Pts',(-3.14877060440328,-1.,2.03660101169715));
#32340=CARTESIAN_POINT('',(-3.24413672884812,-1.,1.88097764062697));
#32341=CARTESIAN_POINT('Origin',(0.,-1.,0.));
#32342=CARTESIAN_POINT('',(-3.70708211654725,-1.,1.97421938526992));
#32343=CARTESIAN_POINT('Ctrl Pts',(-3.24413672884812,-1.,1.88097764062697));
#32344=CARTESIAN_POINT('Ctrl Pts',(-3.24415531671284,-1.,1.8810229239812));
#32345=CARTESIAN_POINT('Ctrl Pts',(-3.24428080353022,-1.,1.88117508446775));
#32346=CARTESIAN_POINT('Ctrl Pts',(-3.24480754676064,-1.,1.88156537699203));
#32347=CARTESIAN_POINT('Ctrl Pts',(-3.2462565441079,-1.,1.88242596600454));
#32348=CARTESIAN_POINT('Ctrl Pts',(-3.24935200511918,-1.,1.88407708646357));
#32349=CARTESIAN_POINT('Ctrl Pts',(-3.25408686339463,-1.,1.88646802523466));
#32350=CARTESIAN_POINT('Ctrl Pts',(-3.25999885193947,-1.,1.88934996203698));
#32351=CARTESIAN_POINT('Ctrl Pts',(-3.26677653888676,-1.,1.89255393500965));
#32352=CARTESIAN_POINT('Ctrl Pts',(-3.27407108933139,-1.,1.89589172903793));
#32353=CARTESIAN_POINT('Ctrl Pts',(-3.28154737912352,-1.,1.89918429230462));
#32354=CARTESIAN_POINT('Ctrl Pts',(-3.2889344860029,-1.,1.90228971247527));
#32355=CARTESIAN_POINT('Ctrl Pts',(-3.29608978722113,-1.,1.90513891864087));
#32356=CARTESIAN_POINT('Ctrl Pts',(-3.30300595568195,-1.,1.90773912171341));
#32357=CARTESIAN_POINT('Ctrl Pts',(-3.30975721158596,-1.,1.91014297830446));
#32358=CARTESIAN_POINT('Ctrl Pts',(-3.31646052426364,-1.,1.91242616234442));
#32359=CARTESIAN_POINT('Ctrl Pts',(-3.32323403454535,-1.,1.91466343916628));
#32360=CARTESIAN_POINT('Ctrl Pts',(-3.33014884257873,-1.,1.91690081930331));
#32361=CARTESIAN_POINT('Ctrl Pts',(-3.33721230710012,-1.,1.9191460961021));
#32362=CARTESIAN_POINT('Ctrl Pts',(-3.34439448941961,-1.,1.92138450828404));
#32363=CARTESIAN_POINT('Ctrl Pts',(-3.35164424847223,-1.,1.92358838440528));
#32364=CARTESIAN_POINT('Ctrl Pts',(-3.35890824422965,-1.,1.92572846125756));
#32365=CARTESIAN_POINT('Ctrl Pts',(-3.36615168657567,-1.,1.92778626543786));
#32366=CARTESIAN_POINT('Ctrl Pts',(-3.37336807068043,-1.,1.92975993109877));
#32367=CARTESIAN_POINT('Ctrl Pts',(-3.3805676852555,-1.,1.93165739093276));
#32368=CARTESIAN_POINT('Ctrl Pts',(-3.38777076883256,-1.,1.93349233176788));
#32369=CARTESIAN_POINT('Ctrl Pts',(-3.39499923640795,-1.,1.93527929945985));
#32370=CARTESIAN_POINT('Ctrl Pts',(-3.40226802104109,-1.,1.93702857723098));
#32371=CARTESIAN_POINT('Ctrl Pts',(-3.40957978266642,-1.,1.93874306008143));
#32372=CARTESIAN_POINT('Ctrl Pts',(-3.41692971994096,-1.,1.94042111965246));
#32373=CARTESIAN_POINT('Ctrl Pts',(-3.42430850941503,-1.,1.94205835913696));
#32374=CARTESIAN_POINT('Ctrl Pts',(-3.43170586602434,-1.,1.94364973660284));
#32375=CARTESIAN_POINT('Ctrl Pts',(-3.43911410197687,-1.,1.94519168842879));
#32376=CARTESIAN_POINT('Ctrl Pts',(-3.44653088665681,-1.,1.94668377715329));
#32377=CARTESIAN_POINT('Ctrl Pts',(-3.45395731584051,-1.,1.94812754766524));
#32378=CARTESIAN_POINT('Ctrl Pts',(-3.46139661060962,-1.,1.94952575850197));
#32379=CARTESIAN_POINT('Ctrl Pts',(-3.46885258974191,-1.,1.95088147859876));
#32380=CARTESIAN_POINT('Ctrl Pts',(-3.47632820495921,-1.,1.95219722189876));
#32381=CARTESIAN_POINT('Ctrl Pts',(-3.48382414832634,-1.,1.95347412486308));
#32382=CARTESIAN_POINT('Ctrl Pts',(-3.49133956289133,-1.,1.95471236969643));
#32383=CARTESIAN_POINT('Ctrl Pts',(-3.49887263575583,-1.,1.95591153823661));
#32384=CARTESIAN_POINT('Ctrl Pts',(-3.50642124159909,-1.,1.95707099606511));
#32385=CARTESIAN_POINT('Ctrl Pts',(-3.51398354617794,-1.,1.95819025316779));
#32386=CARTESIAN_POINT('Ctrl Pts',(-3.52155867431486,-1.,1.95926936324461));
#32387=CARTESIAN_POINT('Ctrl Pts',(-3.52914648844351,-1.,1.96030879411566));
#32388=CARTESIAN_POINT('Ctrl Pts',(-3.53674730625813,-1.,1.96130926212689));
#32389=CARTESIAN_POINT('Ctrl Pts',(-3.54436163300443,-1.,1.96227157573067));
#32390=CARTESIAN_POINT('Ctrl Pts',(-3.55198990600886,-1.,1.96319648628644));
#32391=CARTESIAN_POINT('Ctrl Pts',(-3.55963218706096,-1.,1.96408450906812));
#32392=CARTESIAN_POINT('Ctrl Pts',(-3.56728820357791,-1.,1.96493594634567));
#32393=CARTESIAN_POINT('Ctrl Pts',(-3.57495748600959,-1.,1.96575096652789));
#32394=CARTESIAN_POINT('Ctrl Pts',(-3.58263947663829,-1.,1.96652966688911));
#32395=CARTESIAN_POINT('Ctrl Pts',(-3.59033364022801,-1.,1.96727213799544));
#32396=CARTESIAN_POINT('Ctrl Pts',(-3.59803959819938,-1.,1.96797854118369));
#32397=CARTESIAN_POINT('Ctrl Pts',(-3.60575714017989,-1.,1.9686491188594));
#32398=CARTESIAN_POINT('Ctrl Pts',(-3.61348615496704,-1.,1.96928416040877));
#32399=CARTESIAN_POINT('Ctrl Pts',(-3.62122658401893,-1.,1.96988398129978));
#32400=CARTESIAN_POINT('Ctrl Pts',(-3.62897836973293,-1.,1.97044889850463));
#32401=CARTESIAN_POINT('Ctrl Pts',(-3.63674139590412,-1.,1.97097920454464));
#32402=CARTESIAN_POINT('Ctrl Pts',(-3.64451546723514,-1.,1.97147515441164));
#32403=CARTESIAN_POINT('Ctrl Pts',(-3.652300347166,-1.,1.9719369724024));
#32404=CARTESIAN_POINT('Ctrl Pts',(-3.6600957816636,-1.,1.9723648543905));
#32405=CARTESIAN_POINT('Ctrl Pts',(-3.66790152752075,-1.,1.97275897198678));
#32406=CARTESIAN_POINT('Ctrl Pts',(-3.67571738107084,-1.,1.97311947678516));
#32407=CARTESIAN_POINT('Ctrl Pts',(-3.68354319915092,-1.,1.97344650304519));
#32408=CARTESIAN_POINT('Ctrl Pts',(-3.69137888599902,-1.,1.97374016225483));
#32409=CARTESIAN_POINT('Ctrl Pts',(-3.6976552856004,-1.,1.97394846383216));
#32410=CARTESIAN_POINT('Ctrl Pts',(-3.70236698912904,-1.,1.97408973726715));
#32411=CARTESIAN_POINT('Ctrl Pts',(-3.70551008132332,-1.,1.97417727645308));
#32412=CARTESIAN_POINT('Ctrl Pts',(-3.70708211654725,-1.,1.97421938526992));
#32413=CARTESIAN_POINT('',(-3.77614523045147,-1.,1.8386753923786));
#32414=CARTESIAN_POINT('',(-3.70708211654725,-1.,1.97421938526992));
#32415=CARTESIAN_POINT('',(-3.42859860294306,-1.,1.5189508286633));
#32416=CARTESIAN_POINT('Ctrl Pts',(-3.77614523045147,-1.,1.8386753923786));
#32417=CARTESIAN_POINT('Ctrl Pts',(-3.77518714457833,-1.,1.83742834010626));
#32418=CARTESIAN_POINT('Ctrl Pts',(-3.77326886064398,-1.,1.83493697934534));
#32419=CARTESIAN_POINT('Ctrl Pts',(-3.77038509817999,-1.,1.83120816955645));
#32420=CARTESIAN_POINT('Ctrl Pts',(-3.76652740353775,-1.,1.82625289220915));
#32421=CARTESIAN_POINT('Ctrl Pts',(-3.76168412707948,-1.,1.82008629694091));
#32422=CARTESIAN_POINT('Ctrl Pts',(-3.75681965683071,-1.,1.8139472983358));
#32423=CARTESIAN_POINT('Ctrl Pts',(-3.75193395887977,-1.,1.80783603939617));
#32424=CARTESIAN_POINT('Ctrl Pts',(-3.74702700875467,-1.,1.8017527148577));
#32425=CARTESIAN_POINT('Ctrl Pts',(-3.74209880352445,-1.,1.79569757859422));
#32426=CARTESIAN_POINT('Ctrl Pts',(-3.73714934730681,-1.,1.78967092823491));
#32427=CARTESIAN_POINT('Ctrl Pts',(-3.7321786309547,-1.,1.78367308442901));
#32428=CARTESIAN_POINT('Ctrl Pts',(-3.72718661205609,-1.,1.77770437039658));
#32429=CARTESIAN_POINT('Ctrl Pts',(-3.72217319911254,-1.,1.77176509401761));
#32430=CARTESIAN_POINT('Ctrl Pts',(-3.71713822377359,-1.,1.76585552124394));
#32431=CARTESIAN_POINT('Ctrl Pts',(-3.71208146346136,-1.,1.75997588498865));
#32432=CARTESIAN_POINT('Ctrl Pts',(-3.70700269736659,-1.,1.75412641804042));
#32433=CARTESIAN_POINT('Ctrl Pts',(-3.7019017567335,-1.,1.74830738046057));
#32434=CARTESIAN_POINT('Ctrl Pts',(-3.69677856910517,-1.,1.74251908492617));
#32435=CARTESIAN_POINT('Ctrl Pts',(-3.69163322648036,-1.,1.73676193254557));
#32436=CARTESIAN_POINT('Ctrl Pts',(-3.68646597019332,-1.,1.73103640956717));
#32437=CARTESIAN_POINT('Ctrl Pts',(-3.68127704936579,-1.,1.72534302437056));
#32438=CARTESIAN_POINT('Ctrl Pts',(-3.67606660374709,-1.,1.71968225581808));
#32439=CARTESIAN_POINT('Ctrl Pts',(-3.67083454901611,-1.,1.71405450210383));
#32440=CARTESIAN_POINT('Ctrl Pts',(-3.66558043198876,-1.,1.70846001610956));
#32441=CARTESIAN_POINT('Ctrl Pts',(-3.66030338774847,-1.,1.70289888566873));
#32442=CARTESIAN_POINT('Ctrl Pts',(-3.65500246526749,-1.,1.69737117722534));
#32443=CARTESIAN_POINT('Ctrl Pts',(-3.64967689827371,-1.,1.69187705481689));
#32444=CARTESIAN_POINT('Ctrl Pts',(-3.64432638915203,-1.,1.68641690471457));
#32445=CARTESIAN_POINT('Ctrl Pts',(-3.63895140887462,-1.,1.68099146651586));
#32446=CARTESIAN_POINT('Ctrl Pts',(-3.63355343201232,-1.,1.67560193613156));
#32447=CARTESIAN_POINT('Ctrl Pts',(-3.62813422105271,-1.,1.67024966008045));
#32448=CARTESIAN_POINT('Ctrl Pts',(-3.62269517989109,-1.,1.66493585923855));
#32449=CARTESIAN_POINT('Ctrl Pts',(-3.61723666482456,-1.,1.65966133399186));
#32450=CARTESIAN_POINT('Ctrl Pts',(-3.61175734965127,-1.,1.65442619244325));
#32451=CARTESIAN_POINT('Ctrl Pts',(-3.60625346556992,-1.,1.64922952425832));
#32452=CARTESIAN_POINT('Ctrl Pts',(-3.60072028513845,-1.,1.64407004385582));
#32453=CARTESIAN_POINT('Ctrl Pts',(-3.59515368334893,-1.,1.63894676675352));
#32454=CARTESIAN_POINT('Ctrl Pts',(-3.58955176627879,-1.,1.6338597145126));
#32455=CARTESIAN_POINT('Ctrl Pts',(-3.58391625774343,-1.,1.62881051550745));
#32456=CARTESIAN_POINT('Ctrl Pts',(-3.5782545595439,-1.,1.62380329464844));
#32457=CARTESIAN_POINT('Ctrl Pts',(-3.57257679609806,-1.,1.61884340915404));
#32458=CARTESIAN_POINT('Ctrl Pts',(-3.56689200468387,-1.,1.61393581747514));
#32459=CARTESIAN_POINT('Ctrl Pts',(-3.5612043248298,-1.,1.60908344685457));
#32460=CARTESIAN_POINT('Ctrl Pts',(-3.55550985096129,-1.,1.60428584699853));
#32461=CARTESIAN_POINT('Ctrl Pts',(-3.54979148634454,-1.,1.59953698113457));
#32462=CARTESIAN_POINT('Ctrl Pts',(-3.54402458182337,-1.,1.59482766949766));
#32463=CARTESIAN_POINT('Ctrl Pts',(-3.53818616861077,-1.,1.59014958368739));
#32464=CARTESIAN_POINT('Ctrl Pts',(-3.5322637814708,-1.,1.58549906268088));
#32465=CARTESIAN_POINT('Ctrl Pts',(-3.52626275334881,-1.,1.58088027227848));
#32466=CARTESIAN_POINT('Ctrl Pts',(-3.52021847865912,-1.,1.57631049988158));
#32467=CARTESIAN_POINT('Ctrl Pts',(-3.51418598431665,-1.,1.57181569799743));
#32468=CARTESIAN_POINT('Ctrl Pts',(-3.50821771695363,-1.,1.56742097575012));
#32469=CARTESIAN_POINT('Ctrl Pts',(-3.50234321621578,-1.,1.56314187758675));
#32470=CARTESIAN_POINT('Ctrl Pts',(-3.49655185179655,-1.,1.55897703097874));
#32471=CARTESIAN_POINT('Ctrl Pts',(-3.4907646087742,-1.,1.55489595901116));
#32472=CARTESIAN_POINT('Ctrl Pts',(-3.48485155928567,-1.,1.55084702970452));
#32473=CARTESIAN_POINT('Ctrl Pts',(-3.47868272898751,-1.,1.54678009290276));
#32474=CARTESIAN_POINT('Ctrl Pts',(-3.47217189224653,-1.,1.54266605398187));
#32475=CARTESIAN_POINT('Ctrl Pts',(-3.46531752207153,-1.,1.53851507915502));
#32476=CARTESIAN_POINT('Ctrl Pts',(-3.45825932955032,-1.,1.53440195378792));
#32477=CARTESIAN_POINT('Ctrl Pts',(-3.45127136828305,-1.,1.53046244461635));
#32478=CARTESIAN_POINT('Ctrl Pts',(-3.44469547526647,-1.,1.52686242875556));
#32479=CARTESIAN_POINT('Ctrl Pts',(-3.4388889597401,-1.,1.5237734895035));
#32480=CARTESIAN_POINT('Ctrl Pts',(-3.43417156977893,-1.,1.52134826724292));
#32481=CARTESIAN_POINT('Ctrl Pts',(-3.43101631893414,-1.,1.5198144909338));
#32482=CARTESIAN_POINT('Ctrl Pts',(-3.42946838852587,-1.,1.51914806898491));
#32483=CARTESIAN_POINT('Ctrl Pts',(-3.42884302333841,-1.,1.5189513329503));
#32484=CARTESIAN_POINT('Ctrl Pts',(-3.42864616361875,-1.,1.51893924967331));
#32485=CARTESIAN_POINT('Ctrl Pts',(-3.42859860294306,-1.,1.5189508286633));
#32486=CARTESIAN_POINT('',(-3.49844575334386,-1.,1.35032489087269));
#32487=CARTESIAN_POINT('Origin',(0.,-1.,0.));
#32488=CARTESIAN_POINT('',(-3.97027773754922,-1.,1.36999806084572));
#32489=CARTESIAN_POINT('Ctrl Pts',(-3.49844575334386,-1.,1.35032489087269));
#32490=CARTESIAN_POINT('Ctrl Pts',(-3.49847119623841,-1.,1.35036670893102));
#32491=CARTESIAN_POINT('Ctrl Pts',(-3.49861894124915,-1.,1.35049736560633));
#32492=CARTESIAN_POINT('Ctrl Pts',(-3.49920025459856,-1.,1.35080045218652));
#32493=CARTESIAN_POINT('Ctrl Pts',(-3.5007660381658,-1.,1.35142377279535));
#32494=CARTESIAN_POINT('Ctrl Pts',(-3.50408168106113,-1.,1.3525703284343));
#32495=CARTESIAN_POINT('Ctrl Pts',(-3.50913227060177,-1.,1.35419113576022));
#32496=CARTESIAN_POINT('Ctrl Pts',(-3.51542230699919,-1.,1.35611275237288));
#32497=CARTESIAN_POINT('Ctrl Pts',(-3.52261776117121,-1.,1.35821701528975));
#32498=CARTESIAN_POINT('Ctrl Pts',(-3.53034464961849,-1.,1.36037259643827));
#32499=CARTESIAN_POINT('Ctrl Pts',(-3.53824396425032,-1.,1.36245507339334));
#32500=CARTESIAN_POINT('Ctrl Pts',(-3.54602591832893,-1.,1.36436666257567));
#32501=CARTESIAN_POINT('Ctrl Pts',(-3.55353883995793,-1.,1.36606145456711));
#32502=CARTESIAN_POINT('Ctrl Pts',(-3.56077662028492,-1.,1.36754771771174));
#32503=CARTESIAN_POINT('Ctrl Pts',(-3.56782080304554,-1.,1.36886584973349));
#32504=CARTESIAN_POINT('Ctrl Pts',(-3.57479875549453,-1.,1.37007229485646));
#32505=CARTESIAN_POINT('Ctrl Pts',(-3.58183885982745,-1.,1.37122241663073));
#32506=CARTESIAN_POINT('Ctrl Pts',(-3.5890185384643,-1.,1.37235053661));
#32507=CARTESIAN_POINT('Ctrl Pts',(-3.59634627869117,-1.,1.37346320103184));
#32508=CARTESIAN_POINT('Ctrl Pts',(-3.60379020124038,-1.,1.37455051379642));
#32509=CARTESIAN_POINT('Ctrl Pts',(-3.61129546591082,-1.,1.37559314436641));
#32510=CARTESIAN_POINT('Ctrl Pts',(-3.61880481160408,-1.,1.37657053403102));
#32511=CARTESIAN_POINT('Ctrl Pts',(-3.62628098665112,-1.,1.37746987919868));
#32512=CARTESIAN_POINT('Ctrl Pts',(-3.63371727442448,-1.,1.37829035457324));
#32513=CARTESIAN_POINT('Ctrl Pts',(-3.64112507791112,-1.,1.37903818567347));
#32514=CARTESIAN_POINT('Ctrl Pts',(-3.64852652756444,-1.,1.37972372481598));
#32515=CARTESIAN_POINT('Ctrl Pts',(-3.65594554404396,-1.,1.38035791051215));
#32516=CARTESIAN_POINT('Ctrl Pts',(-3.66339848520874,-1.,1.38094856333558));
#32517=CARTESIAN_POINT('Ctrl Pts',(-3.67088843112282,-1.,1.38149812653876));
#32518=CARTESIAN_POINT('Ctrl Pts',(-3.6784103848243,-1.,1.38200574290626));
#32519=CARTESIAN_POINT('Ctrl Pts',(-3.68595444983844,-1.,1.38246852827185));
#32520=CARTESIAN_POINT('Ctrl Pts',(-3.69350967899523,-1.,1.38288311171649));
#32521=CARTESIAN_POINT('Ctrl Pts',(-3.70106792167894,-1.,1.38324717612862));
#32522=CARTESIAN_POINT('Ctrl Pts',(-3.70862680753343,-1.,1.38356065402122));
#32523=CARTESIAN_POINT('Ctrl Pts',(-3.7161876605181,-1.,1.38382489984585));
#32524=CARTESIAN_POINT('Ctrl Pts',(-3.72375409358805,-1.,1.3840421342895));
#32525=CARTESIAN_POINT('Ctrl Pts',(-3.73133035859283,-1.,1.38421479111531));
#32526=CARTESIAN_POINT('Ctrl Pts',(-3.73891976418099,-1.,1.38434489156456));
#32527=CARTESIAN_POINT('Ctrl Pts',(-3.7465231716786,-1.,1.38443344984389));
#32528=CARTESIAN_POINT('Ctrl Pts',(-3.75413976318727,-1.,1.38448077997155));
#32529=CARTESIAN_POINT('Ctrl Pts',(-3.76176768271347,-1.,1.38448675253343));
#32530=CARTESIAN_POINT('Ctrl Pts',(-3.76940473185775,-1.,1.38445107339517));
#32531=CARTESIAN_POINT('Ctrl Pts',(-3.77704902230441,-1.,1.38437354551435));
#32532=CARTESIAN_POINT('Ctrl Pts',(-3.78469969805134,-1.,1.38425435883773));
#32533=CARTESIAN_POINT('Ctrl Pts',(-3.79235669640907,-1.,1.38409399694588));
#32534=CARTESIAN_POINT('Ctrl Pts',(-3.80002044322169,-1.,1.38389311766701));
#32535=CARTESIAN_POINT('Ctrl Pts',(-3.80769156398429,-1.,1.38365244046226));
#32536=CARTESIAN_POINT('Ctrl Pts',(-3.81537060817765,-1.,1.38337263902766));
#32537=CARTESIAN_POINT('Ctrl Pts',(-3.82305771743715,-1.,1.38305421262724));
#32538=CARTESIAN_POINT('Ctrl Pts',(-3.83075266982138,-1.,1.38269750245086));
#32539=CARTESIAN_POINT('Ctrl Pts',(-3.83845502790609,-1.,1.38230274828774));
#32540=CARTESIAN_POINT('Ctrl Pts',(-3.84616425605705,-1.,1.38187013346089));
#32541=CARTESIAN_POINT('Ctrl Pts',(-3.85387983979557,-1.,1.38139983115075));
#32542=CARTESIAN_POINT('Ctrl Pts',(-3.86160143044187,-1.,1.38089205993067));
#32543=CARTESIAN_POINT('Ctrl Pts',(-3.86932885813403,-1.,1.38034709213129));
#32544=CARTESIAN_POINT('Ctrl Pts',(-3.87706205830865,-1.,1.37976523097187));
#32545=CARTESIAN_POINT('Ctrl Pts',(-3.88480102249461,-1.,1.37914679719446));
#32546=CARTESIAN_POINT('Ctrl Pts',(-3.89254574338385,-1.,1.37849211287981));
#32547=CARTESIAN_POINT('Ctrl Pts',(-3.90029615196255,-1.,1.3778014851263));
#32548=CARTESIAN_POINT('Ctrl Pts',(-3.90805209522729,-1.,1.3770751963376));
#32549=CARTESIAN_POINT('Ctrl Pts',(-3.91581337461825,-1.,1.37631350505516));
#32550=CARTESIAN_POINT('Ctrl Pts',(-3.92357976987132,-1.,1.37551664448057));
#32551=CARTESIAN_POINT('Ctrl Pts',(-3.93135106761941,-1.,1.37468482215784));
#32552=CARTESIAN_POINT('Ctrl Pts',(-3.93912709041791,-1.,1.37381821967499));
#32553=CARTESIAN_POINT('Ctrl Pts',(-3.94690771786926,-1.,1.37291699203423));
#32554=CARTESIAN_POINT('Ctrl Pts',(-3.95469287283105,-1.,1.37198126433139));
#32555=CARTESIAN_POINT('Ctrl Pts',(-3.96092458508407,-1.,1.37120515615663));
#32556=CARTESIAN_POINT('Ctrl Pts',(-3.96560037975788,-1.,1.37060761746027));
#32557=CARTESIAN_POINT('Ctrl Pts',(-3.9687184694173,-1.,1.37020239094758));
#32558=CARTESIAN_POINT('Ctrl Pts',(-3.97027773754922,-1.,1.36999806084572));
#32559=CARTESIAN_POINT('',(-4.01728681790024,-1.,1.22531898815164));
#32560=CARTESIAN_POINT('',(-3.97027773754922,-1.,1.36999806084572));
#32561=CARTESIAN_POINT('',(-3.62400312501199,-1.,0.963899035118985));
#32562=CARTESIAN_POINT('Ctrl Pts',(-4.01728681790024,-1.,1.22531898815164));
#32563=CARTESIAN_POINT('Ctrl Pts',(-4.01614544569895,-1.,1.22423716681317));
#32564=CARTESIAN_POINT('Ctrl Pts',(-4.01386104433519,-1.,1.22207656455845));
#32565=CARTESIAN_POINT('Ctrl Pts',(-4.01042947140789,-1.,1.21884478244403));
#32566=CARTESIAN_POINT('Ctrl Pts',(-4.00584409522722,-1.,1.21455398918133));
#32567=CARTESIAN_POINT('Ctrl Pts',(-4.00009577950721,-1.,1.20922097029551));
#32568=CARTESIAN_POINT('Ctrl Pts',(-3.99433084799666,-1.,1.20391852375139));
#32569=CARTESIAN_POINT('Ctrl Pts',(-3.98854928957189,-1.,1.19864679609566));
#32570=CARTESIAN_POINT('Ctrl Pts',(-3.98275111052561,-1.,1.19340598349475));
#32571=CARTESIAN_POINT('Ctrl Pts',(-3.97693634767754,-1.,1.18819633715539));
#32572=CARTESIAN_POINT('Ctrl Pts',(-3.97110505165415,-1.,1.18301815039831));
#32573=CARTESIAN_POINT('Ctrl Pts',(-3.96525726358159,-1.,1.17787174135592));
#32574=CARTESIAN_POINT('Ctrl Pts',(-3.95939299213276,-1.,1.17275743590361));
#32575=CARTESIAN_POINT('Ctrl Pts',(-3.95351219509876,-1.,1.16767555244438));
#32576=CARTESIAN_POINT('Ctrl Pts',(-3.94761474780583,-1.,1.16262637999157));
#32577=CARTESIAN_POINT('Ctrl Pts',(-3.94170046685203,-1.,1.15761018340956));
#32578=CARTESIAN_POINT('Ctrl Pts',(-3.9357691705628,-1.,1.1526272271632));
#32579=CARTESIAN_POINT('Ctrl Pts',(-3.92982073294257,-1.,1.14767779451123));
#32580=CARTESIAN_POINT('Ctrl Pts',(-3.92385513133997,-1.,1.14276220561593));
#32581=CARTESIAN_POINT('Ctrl Pts',(-3.91787251936827,-1.,1.13788084225554));
#32582=CARTESIAN_POINT('Ctrl Pts',(-3.91187321145649,-1.,1.13303414693896));
#32583=CARTESIAN_POINT('Ctrl Pts',(-3.90585753318737,-1.,1.12822258281553));
#32584=CARTESIAN_POINT('Ctrl Pts',(-3.89982569750025,-1.,1.12344660099043));
#32585=CARTESIAN_POINT('Ctrl Pts',(-3.89377768340344,-1.,1.11870660794603));
#32586=CARTESIAN_POINT('Ctrl Pts',(-3.88771308285171,-1.,1.11400292434429));
#32587=CARTESIAN_POINT('Ctrl Pts',(-3.88163105531724,-1.,1.10933577224008));
#32588=CARTESIAN_POINT('Ctrl Pts',(-3.87553067187514,-1.,1.10470536603287));
#32589=CARTESIAN_POINT('Ctrl Pts',(-3.86941120134849,-1.,1.10011198761195));
#32590=CARTESIAN_POINT('Ctrl Pts',(-3.86327241021247,-1.,1.09555606505013));
#32591=CARTESIAN_POINT('Ctrl Pts',(-3.85711487933931,-1.,1.09103825516294));
#32592=CARTESIAN_POINT('Ctrl Pts',(-3.85094025222713,-1.,1.08655950846384));
#32593=CARTESIAN_POINT('Ctrl Pts',(-3.8447504803063,-1.,1.08212087917991));
#32594=CARTESIAN_POINT('Ctrl Pts',(-3.83854714117491,-1.,1.07772335353858));
#32595=CARTESIAN_POINT('Ctrl Pts',(-3.83233071195144,-1.,1.07336766633459));
#32596=CARTESIAN_POINT('Ctrl Pts',(-3.82609989967276,-1.,1.06905413180359));
#32597=CARTESIAN_POINT('Ctrl Pts',(-3.81985083953012,-1.,1.0647824403893));
#32598=CARTESIAN_POINT('Ctrl Pts',(-3.8135786611749,-1.,1.06055206187299));
#32599=CARTESIAN_POINT('Ctrl Pts',(-3.80727913637791,-1.,1.05636266918644));
#32600=CARTESIAN_POINT('Ctrl Pts',(-3.80095039790681,-1.,1.05221457990016));
#32601=CARTESIAN_POINT('Ctrl Pts',(-3.79459440308786,-1.,1.04810913267639));
#32602=CARTESIAN_POINT('Ctrl Pts',(-3.78821910787179,-1.,1.04404924374422));
#32603=CARTESIAN_POINT('Ctrl Pts',(-3.7818353500817,-1.,1.04003862055798));
#32604=CARTESIAN_POINT('Ctrl Pts',(-3.77545283140427,-1.,1.03608074678008));
#32605=CARTESIAN_POINT('Ctrl Pts',(-3.76907609832516,-1.,1.03217786604919));
#32606=CARTESIAN_POINT('Ctrl Pts',(-3.76270122291245,-1.,1.02833014458184));
#32607=CARTESIAN_POINT('Ctrl Pts',(-3.75631037456224,-1.,1.02453429444668));
#32608=CARTESIAN_POINT('Ctrl Pts',(-3.74987777155873,-1.,1.02078510487439));
#32609=CARTESIAN_POINT('Ctrl Pts',(-3.74337942504993,-1.,1.01707794311088));
#32610=CARTESIAN_POINT('Ctrl Pts',(-3.73680245055747,-1.,1.01341114319906));
#32611=CARTESIAN_POINT('Ctrl Pts',(-3.73015276704407,-1.,1.00978798539491));
#32612=CARTESIAN_POINT('Ctrl Pts',(-3.72346803750544,-1.,1.00622000735696));
#32613=CARTESIAN_POINT('Ctrl Pts',(-3.71680667125047,-1.,1.00272423396802));
#32614=CARTESIAN_POINT('Ctrl Pts',(-3.7102243971387,-1.,0.999317260756344));
#32615=CARTESIAN_POINT('Ctrl Pts',(-3.70375282282107,-1.,0.996009819772431));
#32616=CARTESIAN_POINT('Ctrl Pts',(-3.69738123415696,-1.,0.992802218332103));
#32617=CARTESIAN_POINT('Ctrl Pts',(-3.69102682138955,-1.,0.989676715398858));
#32618=CARTESIAN_POINT('Ctrl Pts',(-3.6845531792623,-1.,0.986602639864285));
#32619=CARTESIAN_POINT('Ctrl Pts',(-3.67782408841876,-1.,0.983550791470864));
#32620=CARTESIAN_POINT('Ctrl Pts',(-3.67074983340444,-1.,0.980505922458494));
#32621=CARTESIAN_POINT('Ctrl Pts',(-3.66333049637403,-1.,0.977478312751416));
#32622=CARTESIAN_POINT('Ctrl Pts',(-3.6557157673487,-1.,0.974519971354138));
#32623=CARTESIAN_POINT('Ctrl Pts',(-3.64819756447072,-1.,0.971722122060277));
#32624=CARTESIAN_POINT('Ctrl Pts',(-3.64113946505393,-1.,0.969195124674829));
#32625=CARTESIAN_POINT('Ctrl Pts',(-3.6349212208096,-1.,0.967052554540877));
#32626=CARTESIAN_POINT('Ctrl Pts',(-3.62988252139998,-1.,0.965395153165716));
#32627=CARTESIAN_POINT('Ctrl Pts',(-3.62652618145252,-1.,0.964373850166081));
#32628=CARTESIAN_POINT('Ctrl Pts',(-3.62489305727516,-1.,0.963957782642589));
#32629=CARTESIAN_POINT('Ctrl Pts',(-3.62424461507455,-1.,0.963861297423579));
#32630=CARTESIAN_POINT('Ctrl Pts',(-3.62404828878375,-1.,0.963880158556713));
#32631=CARTESIAN_POINT('Ctrl Pts',(-3.62400312501199,-1.,0.963899035118985));
#32632=CARTESIAN_POINT('',(-3.66661143271648,-1.,0.786422660833743));
#32633=CARTESIAN_POINT('Origin',(0.,-1.,0.));
#32634=CARTESIAN_POINT('',(-4.13571194405636,-1.,0.732042837400619));
#32635=CARTESIAN_POINT('Ctrl Pts',(-3.66661143271648,-1.,0.786422660833743));
#32636=CARTESIAN_POINT('Ctrl Pts',(-3.66664310415236,-1.,0.786459983896781));
#32637=CARTESIAN_POINT('Ctrl Pts',(-3.66680946938396,-1.,0.78656591955989));
#32638=CARTESIAN_POINT('Ctrl Pts',(-3.66743103898844,-1.,0.786774337198499));
#32639=CARTESIAN_POINT('Ctrl Pts',(-3.66907505398769,-1.,0.787145041181588));
#32640=CARTESIAN_POINT('Ctrl Pts',(-3.672529236635,-1.,0.787758799995426));
#32641=CARTESIAN_POINT('Ctrl Pts',(-3.67777119516438,-1.,0.788569566220662));
#32642=CARTESIAN_POINT('Ctrl Pts',(-3.68428439784285,-1.,0.789483546065158));
#32643=CARTESIAN_POINT('Ctrl Pts',(-3.69172044327754,-1.,0.79043628498958));
#32644=CARTESIAN_POINT('Ctrl Pts',(-3.69968940808982,-1.,0.791356575696509));
#32645=CARTESIAN_POINT('Ctrl Pts',(-3.70781724021879,-1.,0.792177688845967));
#32646=CARTESIAN_POINT('Ctrl Pts',(-3.7158024239604,-1.,0.792848377370115));
#32647=CARTESIAN_POINT('Ctrl Pts',(-3.7234879729357,-1.,0.79334702378387));
#32648=CARTESIAN_POINT('Ctrl Pts',(-3.7308691469564,-1.,0.793682750269347));
#32649=CARTESIAN_POINT('Ctrl Pts',(-3.73803280541576,-1.,0.79388270093679));
#32650=CARTESIAN_POINT('Ctrl Pts',(-3.74511357728827,-1.,0.79398270045988));
#32651=CARTESIAN_POINT('Ctrl Pts',(-3.75224692493895,-1.,0.79401734737144));
#32652=CARTESIAN_POINT('Ctrl Pts',(-3.75951468666325,-1.,0.794008429135047));
#32653=CARTESIAN_POINT('Ctrl Pts',(-3.76692626931184,-1.,0.793961083689141));
#32654=CARTESIAN_POINT('Ctrl Pts',(-3.77444863801264,-1.,0.793870523787515));
#32655=CARTESIAN_POINT('Ctrl Pts',(-3.78202460377617,-1.,0.793726235781339));
#32656=CARTESIAN_POINT('Ctrl Pts',(-3.78959439439222,-1.,0.793516871680966));
#32657=CARTESIAN_POINT('Ctrl Pts',(-3.79711921389862,-1.,0.7932356129732));
#32658=CARTESIAN_POINT('Ctrl Pts',(-3.80459229925598,-1.,0.792882695234693));
#32659=CARTESIAN_POINT('Ctrl Pts',(-3.81202588694726,-1.,0.792462483517568));
#32660=CARTESIAN_POINT('Ctrl Pts',(-3.81944345442237,-1.,0.791981740718606));
#32661=CARTESIAN_POINT('Ctrl Pts',(-3.82687033899799,-1.,0.791447528662381));
#32662=CARTESIAN_POINT('Ctrl Pts',(-3.83432392054804,-1.,0.79086501270534));
#32663=CARTESIAN_POINT('Ctrl Pts',(-3.84180762342476,-1.,0.790236124191289));
#32664=CARTESIAN_POINT('Ctrl Pts',(-3.8493163780891,-1.,0.789560798155618));
#32665=CARTESIAN_POINT('Ctrl Pts',(-3.85683995872536,-1.,0.788837734090688));
#32666=CARTESIAN_POINT('Ctrl Pts',(-3.86436702561342,-1.,0.788065315093771));
#32667=CARTESIAN_POINT('Ctrl Pts',(-3.87188916600905,-1.,0.78724252761798));
#32668=CARTESIAN_POINT('Ctrl Pts',(-3.87940402818186,-1.,0.786369675812592));
#32669=CARTESIAN_POINT('Ctrl Pts',(-3.88691313167399,-1.,0.785447890340723));
#32670=CARTESIAN_POINT('Ctrl Pts',(-3.89442039235105,-1.,0.784478799358335));
#32671=CARTESIAN_POINT('Ctrl Pts',(-3.90193039043971,-1.,0.783464141529082));
#32672=CARTESIAN_POINT('Ctrl Pts',(-3.90944671004536,-1.,0.782405395622758));
#32673=CARTESIAN_POINT('Ctrl Pts',(-3.9169703605466,-1.,0.781303428618343));
#32674=CARTESIAN_POINT('Ctrl Pts',(-3.92450058323799,-1.,0.780158678615506));
#32675=CARTESIAN_POINT('Ctrl Pts',(-3.93203552473153,-1.,0.778971308134786));
#32676=CARTESIAN_POINT('Ctrl Pts',(-3.93957296768098,-1.,0.777741370568549));
#32677=CARTESIAN_POINT('Ctrl Pts',(-3.94711101619471,-1.,0.77646896669796));
#32678=CARTESIAN_POINT('Ctrl Pts',(-3.95464885452364,-1.,0.775154418039441));
#32679=CARTESIAN_POINT('Ctrl Pts',(-3.96218649639876,-1.,0.773798212026682));
#32680=CARTESIAN_POINT('Ctrl Pts',(-3.96972446532832,-1.,0.772400931772238));
#32681=CARTESIAN_POINT('Ctrl Pts',(-3.97726349165507,-1.,0.770963190030503));
#32682=CARTESIAN_POINT('Ctrl Pts',(-3.98480422348403,-1.,0.769485566245459));
#32683=CARTESIAN_POINT('Ctrl Pts',(-3.99234687880892,-1.,0.767968531377708));
#32684=CARTESIAN_POINT('Ctrl Pts',(-3.99989129179464,-1.,0.766412457135785));
#32685=CARTESIAN_POINT('Ctrl Pts',(-4.00743706791366,-1.,0.764817648784946));
#32686=CARTESIAN_POINT('Ctrl Pts',(-4.01498370680434,-1.,0.763184371182826));
#32687=CARTESIAN_POINT('Ctrl Pts',(-4.02253072741347,-1.,0.761512875859941));
#32688=CARTESIAN_POINT('Ctrl Pts',(-4.0300778195465,-1.,0.759803433244166));
#32689=CARTESIAN_POINT('Ctrl Pts',(-4.03762485803468,-1.,0.758056338885553));
#32690=CARTESIAN_POINT('Ctrl Pts',(-4.04517182654344,-1.,0.756271902370186));
#32691=CARTESIAN_POINT('Ctrl Pts',(-4.05271876688106,-1.,0.754450441816411));
#32692=CARTESIAN_POINT('Ctrl Pts',(-4.06026572221399,-1.,0.752592276482869));
#32693=CARTESIAN_POINT('Ctrl Pts',(-4.06781267241886,-1.,0.750697720483175));
#32694=CARTESIAN_POINT('Ctrl Pts',(-4.07535951055363,-1.,0.748767076679177));
#32695=CARTESIAN_POINT('Ctrl Pts',(-4.08290608094789,-1.,0.746800631490821));
#32696=CARTESIAN_POINT('Ctrl Pts',(-4.09045220253011,-1.,0.744798649705514));
#32697=CARTESIAN_POINT('Ctrl Pts',(-4.09799769702712,-1.,0.742761369690017));
#32698=CARTESIAN_POINT('Ctrl Pts',(-4.1055424175856,-1.,0.740688998555151));
#32699=CARTESIAN_POINT('Ctrl Pts',(-4.11308626953795,-1.,0.738581708229118));
#32700=CARTESIAN_POINT('Ctrl Pts',(-4.12062919626082,-1.,0.736439634335347));
#32701=CARTESIAN_POINT('Ctrl Pts',(-4.12666277572794,-1.,0.734698226767512));
#32702=CARTESIAN_POINT('Ctrl Pts',(-4.13118752796397,-1.,0.733376589325634));
#32703=CARTESIAN_POINT('Ctrl Pts',(-4.13420383737278,-1.,0.732488575135926));
#32704=CARTESIAN_POINT('Ctrl Pts',(-4.13571194405636,-1.,0.732042837400619));
#32705=CARTESIAN_POINT('',(-4.15950947128175,-1.,0.581791163835814));
#32706=CARTESIAN_POINT('',(-4.13571194405636,-1.,0.732042837400619));
#32707=CARTESIAN_POINT('',(-3.73017266276632,-1.,0.385112848332549));
#32708=CARTESIAN_POINT('Ctrl Pts',(-4.15950947128175,-1.,0.581791163835814));
#32709=CARTESIAN_POINT('Ctrl Pts',(-4.15821291712391,-1.,0.580901211462913));
#32710=CARTESIAN_POINT('Ctrl Pts',(-4.15561864787379,-1.,0.579124568912543));
#32711=CARTESIAN_POINT('Ctrl Pts',(-4.1517237611974,-1.,0.576469391673916));
#32712=CARTESIAN_POINT('Ctrl Pts',(-4.14652361065787,-1.,0.572948736066276));
#32713=CARTESIAN_POINT('Ctrl Pts',(-4.14001179828669,-1.,0.568580610187116));
#32714=CARTESIAN_POINT('Ctrl Pts',(-4.13348835726086,-1.,0.564245279535705));
#32715=CARTESIAN_POINT('Ctrl Pts',(-4.12695329951859,-1.,0.559942890594628));
#32716=CARTESIAN_POINT('Ctrl Pts',(-4.1204066619623,-1.,0.555673636130778));
#32717=CARTESIAN_POINT('Ctrl Pts',(-4.11384852025578,-1.,0.551437758498246));
#32718=CARTESIAN_POINT('Ctrl Pts',(-4.1072789702877,-1.,0.547235539486759));
#32719=CARTESIAN_POINT('Ctrl Pts',(-4.10069810244473,-1.,0.543067286878457));
#32720=CARTESIAN_POINT('Ctrl Pts',(-4.09410597627116,-1.,0.53893332117992));
#32721=CARTESIAN_POINT('Ctrl Pts',(-4.08750259988693,-1.,0.534833963476999));
#32722=CARTESIAN_POINT('Ctrl Pts',(-4.08088789536488,-1.,0.530769518728075));
#32723=CARTESIAN_POINT('Ctrl Pts',(-4.07426172299496,-1.,0.526740277226999));
#32724=CARTESIAN_POINT('Ctrl Pts',(-4.06762394471075,-1.,0.522746528602767));
#32725=CARTESIAN_POINT('Ctrl Pts',(-4.06097448037934,-1.,0.518788572336809));
#32726=CARTESIAN_POINT('Ctrl Pts',(-4.05431335771261,-1.,0.514866728193104));
#32727=CARTESIAN_POINT('Ctrl Pts',(-4.04764078815591,-1.,0.510981349219173));
#32728=CARTESIAN_POINT('Ctrl Pts',(-4.04095715149074,-1.,0.507132823288361));
#32729=CARTESIAN_POINT('Ctrl Pts',(-4.0342628417439,-1.,0.503321556915513));
#32730=CARTESIAN_POINT('Ctrl Pts',(-4.0275581398015,-1.,0.499547962340889));
#32731=CARTESIAN_POINT('Ctrl Pts',(-4.02084308851813,-1.,0.495812444326223));
#32732=CARTESIAN_POINT('Ctrl Pts',(-4.01411733503486,-1.,0.49211538341793));
#32733=CARTESIAN_POINT('Ctrl Pts',(-4.0073800839092,-1.,0.48845713042453));
#32734=CARTESIAN_POINT('Ctrl Pts',(-4.00063045119234,-1.,0.484838042421754));
#32735=CARTESIAN_POINT('Ctrl Pts',(-3.99386775880655,-1.,0.481258512209638));
#32736=CARTESIAN_POINT('Ctrl Pts',(-3.98709184306743,-1.,0.477718999122033));
#32737=CARTESIAN_POINT('Ctrl Pts',(-3.9803033804443,-1.,0.474220061019542));
#32738=CARTESIAN_POINT('Ctrl Pts',(-3.97350414289415,-1.,0.470762379613477));
#32739=CARTESIAN_POINT('Ctrl Pts',(-3.96669622273946,-1.,0.467346690880671));
#32740=CARTESIAN_POINT('Ctrl Pts',(-3.95988133243543,-1.,0.463973722115744));
#32741=CARTESIAN_POINT('Ctrl Pts',(-3.95306005817363,-1.,0.460644124429119));
#32742=CARTESIAN_POINT('Ctrl Pts',(-3.94623117206675,-1.,0.457358410451674));
#32743=CARTESIAN_POINT('Ctrl Pts',(-3.93939080846298,-1.,0.454116879027576));
#32744=CARTESIAN_POINT('Ctrl Pts',(-3.93253407403128,-1.,0.450919768356347));
#32745=CARTESIAN_POINT('Ctrl Pts',(-3.92565674143424,-1.,0.447767416837296));
#32746=CARTESIAN_POINT('Ctrl Pts',(-3.91875701610721,-1.,0.444660430230592));
#32747=CARTESIAN_POINT('Ctrl Pts',(-3.91183704069146,-1.,0.441599824524047));
#32748=CARTESIAN_POINT('Ctrl Pts',(-3.90490512938546,-1.,0.438587235458233));
#32749=CARTESIAN_POINT('Ctrl Pts',(-3.8979725665544,-1.,0.435624629433505));
#32750=CARTESIAN_POINT('Ctrl Pts',(-3.89104947940592,-1.,0.432713929544439));
#32751=CARTESIAN_POINT('Ctrl Pts',(-3.88414070943334,-1.,0.429856640579733));
#32752=CARTESIAN_POINT('Ctrl Pts',(-3.87724240306609,-1.,0.427053541173469));
#32753=CARTESIAN_POINT('Ctrl Pts',(-3.87033643487882,-1.,0.424304173195142));
#32754=CARTESIAN_POINT('Ctrl Pts',(-3.86339652542749,-1.,0.421607423177575));
#32755=CARTESIAN_POINT('Ctrl Pts',(-3.85639825648031,-1.,0.418962468086809));
#32756=CARTESIAN_POINT('Ctrl Pts',(-3.8493286415751,-1.,0.41636967805292));
#32757=CARTESIAN_POINT('Ctrl Pts',(-3.84219403994742,-1.,0.413831367016726));
#32758=CARTESIAN_POINT('Ctrl Pts',(-3.83503345578645,-1.,0.411353038798459));
#32759=CARTESIAN_POINT('Ctrl Pts',(-3.82790724256397,-1.,0.408942371447377));
#32760=CARTESIAN_POINT('Ctrl Pts',(-3.82087303913741,-1.,0.406607038258906));
#32761=CARTESIAN_POINT('Ctrl Pts',(-3.81396374287762,-1.,0.404352694628236));
#32762=CARTESIAN_POINT('Ctrl Pts',(-3.80716881962763,-1.,0.402181320148474));
#32763=CARTESIAN_POINT('Ctrl Pts',(-3.80040370384659,-1.,0.400088346504726));
#32764=CARTESIAN_POINT('Ctrl Pts',(-3.79352887163457,-1.,0.398064818684158));
#32765=CARTESIAN_POINT('Ctrl Pts',(-3.78640521279479,-1.,0.396103205335028));
#32766=CARTESIAN_POINT('Ctrl Pts',(-3.77894173114368,-1.,0.394202481011595));
#32767=CARTESIAN_POINT('Ctrl Pts',(-3.77114011595892,-1.,0.392372786223346));
#32768=CARTESIAN_POINT('Ctrl Pts',(-3.76315635032993,-1.,0.390642072979259));
#32769=CARTESIAN_POINT('Ctrl Pts',(-3.75529302894757,-1.,0.389054775898251));
#32770=CARTESIAN_POINT('Ctrl Pts',(-3.74792651696269,-1.,0.387663020050396));
#32771=CARTESIAN_POINT('Ctrl Pts',(-3.74144965781088,-1.,0.386519576222035));
#32772=CARTESIAN_POINT('Ctrl Pts',(-3.73621371845475,-1.,0.385670806454744));
#32773=CARTESIAN_POINT('Ctrl Pts',(-3.73273893363318,-1.,0.385187124633964));
#32774=CARTESIAN_POINT('Ctrl Pts',(-3.73106082862399,-1.,0.385031656499141));
#32775=CARTESIAN_POINT('Ctrl Pts',(-3.73040527620929,-1.,0.385037797882046));
#32776=CARTESIAN_POINT('Ctrl Pts',(-3.73021431755218,-1.,0.385087139001609));
#32777=CARTESIAN_POINT('Ctrl Pts',(-3.73017266276632,-1.,0.385112848332549));
#32778=CARTESIAN_POINT('',(-3.74449296982994,-1.,0.203156094897895));
#32779=CARTESIAN_POINT('Origin',(0.,-1.,0.));
#32780=CARTESIAN_POINT('',(-4.19931119685982,-1.,0.0760622897878236));
#32781=CARTESIAN_POINT('Ctrl Pts',(-3.74449296982994,-1.,0.203156094897895));
#32782=CARTESIAN_POINT('Ctrl Pts',(-3.74453008995129,-1.,0.203188003947965));
#32783=CARTESIAN_POINT('Ctrl Pts',(-3.74471097893961,-1.,0.203266610111264));
#32784=CARTESIAN_POINT('Ctrl Pts',(-3.74535749969262,-1.,0.203375226874331));
#32785=CARTESIAN_POINT('Ctrl Pts',(-3.74703926501843,-1.,0.203484186269314));
#32786=CARTESIAN_POINT('Ctrl Pts',(-3.75054693397716,-1.,0.203550035479097));
#32787=CARTESIAN_POINT('Ctrl Pts',(-3.75585118707924,-1.,0.203530796848403));
#32788=CARTESIAN_POINT('Ctrl Pts',(-3.76242717937273,-1.,0.203414634707646));
#32789=CARTESIAN_POINT('Ctrl Pts',(-3.76992071595267,-1.,0.203192390045337));
#32790=CARTESIAN_POINT('Ctrl Pts',(-3.77793553476879,-1.,0.202854729699196));
#32791=CARTESIAN_POINT('Ctrl Pts',(-3.78609175019317,-1.,0.202394260512193));
#32792=CARTESIAN_POINT('Ctrl Pts',(-3.79408354187274,-1.,0.201807533800799));
#32793=CARTESIAN_POINT('Ctrl Pts',(-3.80175247447171,-1.,0.201097756307252));
#32794=CARTESIAN_POINT('Ctrl Pts',(-3.80909529318501,-1.,0.20027467943329));
#32795=CARTESIAN_POINT('Ctrl Pts',(-3.81620203429702,-1.,0.199351525297396));
#32796=CARTESIAN_POINT('Ctrl Pts',(-3.82321127348981,-1.,0.19834261690047));
#32797=CARTESIAN_POINT('Ctrl Pts',(-3.83026221776488,-1.,0.197260935827375));
#32798=CARTESIAN_POINT('Ctrl Pts',(-3.83743910616265,-1.,0.196115198971889));
#32799=CARTESIAN_POINT('Ctrl Pts',(-3.84475203347052,-1.,0.194909009460254));
#32800=CARTESIAN_POINT('Ctrl Pts',(-3.85216762264019,-1.,0.193642806777747));
#32801=CARTESIAN_POINT('Ctrl Pts',(-3.85962774407652,-1.,0.192315153044979));
#32802=CARTESIAN_POINT('Ctrl Pts',(-3.8670715862477,-1.,0.190924190418613));
#32803=CARTESIAN_POINT('Ctrl Pts',(-3.87445976418377,-1.,0.189469253358254));
#32804=CARTESIAN_POINT('Ctrl Pts',(-3.88178563496187,-1.,0.187951632512663));
#32805=CARTESIAN_POINT('Ctrl Pts',(-3.88906196725817,-1.,0.186373724985263));
#32806=CARTESIAN_POINT('Ctrl Pts',(-3.89631300742633,-1.,0.184738537728035));
#32807=CARTESIAN_POINT('Ctrl Pts',(-3.90356488555138,-1.,0.183049081993193));
#32808=CARTESIAN_POINT('Ctrl Pts',(-3.91083557557193,-1.,0.181307740731796));
#32809=CARTESIAN_POINT('Ctrl Pts',(-3.91812876180948,-1.,0.179515885822894));
#32810=CARTESIAN_POINT('Ctrl Pts',(-3.92543942697672,-1.,0.177674246152328));
#32811=CARTESIAN_POINT('Ctrl Pts',(-3.93275726771049,-1.,0.175783136893872));
#32812=CARTESIAN_POINT('Ctrl Pts',(-3.94007083096214,-1.,0.173842734974607));
#32813=CARTESIAN_POINT('Ctrl Pts',(-3.94737164900861,-1.,0.171853355369233));
#32814=CARTESIAN_POINT('Ctrl Pts',(-3.95465744665263,-1.,0.16981566637413));
#32815=CARTESIAN_POINT('Ctrl Pts',(-3.96192990160296,-1.,0.167730547023312));
#32816=CARTESIAN_POINT('Ctrl Pts',(-3.9691931362141,-1.,0.165598992851097));
#32817=CARTESIAN_POINT('Ctrl Pts',(-3.97645194630944,-1.,0.163422004609999));
#32818=CARTESIAN_POINT('Ctrl Pts',(-3.98371010319866,-1.,0.161200482186087));
#32819=CARTESIAN_POINT('Ctrl Pts',(-3.99096873945862,-1.,0.158935123982796));
#32820=CARTESIAN_POINT('Ctrl Pts',(-3.99822717425869,-1.,0.156626481393735));
#32821=CARTESIAN_POINT('Ctrl Pts',(-4.00548360245297,-1.,0.15427500487231));
#32822=CARTESIAN_POINT('Ctrl Pts',(-4.01273584234684,-1.,0.151881094022909));
#32823=CARTESIAN_POINT('Ctrl Pts',(-4.01998203715588,-1.,0.149445144968707));
#32824=CARTESIAN_POINT('Ctrl Pts',(-4.02722143147048,-1.,0.146967602878998));
#32825=CARTESIAN_POINT('Ctrl Pts',(-4.03445411510403,-1.,0.144448947038352));
#32826=CARTESIAN_POINT('Ctrl Pts',(-4.04168069633842,-1.,0.141889671485508));
#32827=CARTESIAN_POINT('Ctrl Pts',(-4.04890199238056,-1.,0.139290267180059));
#32828=CARTESIAN_POINT('Ctrl Pts',(-4.05611873400122,-1.,0.136651205046111));
#32829=CARTESIAN_POINT('Ctrl Pts',(-4.06333121018476,-1.,0.133972916144225));
#32830=CARTESIAN_POINT('Ctrl Pts',(-4.07053931528579,-1.,0.131255793548914));
#32831=CARTESIAN_POINT('Ctrl Pts',(-4.07774270738809,-1.,0.128500200484814));
#32832=CARTESIAN_POINT('Ctrl Pts',(-4.08494093372315,-1.,0.125706476822529));
#32833=CARTESIAN_POINT('Ctrl Pts',(-4.09213355850836,-1.,0.122874946249119));
#32834=CARTESIAN_POINT('Ctrl Pts',(-4.09932031767243,-1.,0.120005924388162));
#32835=CARTESIAN_POINT('Ctrl Pts',(-4.10650113382187,-1.,0.117099722731704));
#32836=CARTESIAN_POINT('Ctrl Pts',(-4.11367603925313,-1.,0.114156649609601));
#32837=CARTESIAN_POINT('Ctrl Pts',(-4.12084512502444,-1.,0.111177012683377));
#32838=CARTESIAN_POINT('Ctrl Pts',(-4.12800848371386,-1.,0.10816112052835));
#32839=CARTESIAN_POINT('Ctrl Pts',(-4.13516614458396,-1.,0.105109286538864));
#32840=CARTESIAN_POINT('Ctrl Pts',(-4.14231804938737,-1.,0.102021826577454));
#32841=CARTESIAN_POINT('Ctrl Pts',(-4.1494640891762,-1.,0.0988990478899811));
#32842=CARTESIAN_POINT('Ctrl Pts',(-4.15660412653006,-1.,0.0957412403297067));
#32843=CARTESIAN_POINT('Ctrl Pts',(-4.16373802265942,-1.,0.092548667216769));
#32844=CARTESIAN_POINT('Ctrl Pts',(-4.17086566491823,-1.,0.0893215560850327));
#32845=CARTESIAN_POINT('Ctrl Pts',(-4.17798698669991,-1.,0.0860600915552515));
#32846=CARTESIAN_POINT('Ctrl Pts',(-4.1851019532944,-1.,0.082764416438951));
#32847=CARTESIAN_POINT('Ctrl Pts',(-4.19078883322483,-1.,0.0801005887117603));
#32848=CARTESIAN_POINT('Ctrl Pts',(-4.19505112860624,-1.,0.0780873956244402));
#32849=CARTESIAN_POINT('Ctrl Pts',(-4.19789138621624,-1.,0.0767384596142195));
#32850=CARTESIAN_POINT('Ctrl Pts',(-4.19931119685982,-1.,0.0760622897878236));
#32851=CARTESIAN_POINT('',(-4.19931119685982,-1.,-0.0760622897878246));
#32852=CARTESIAN_POINT('',(-4.19931119685982,-1.,0.0760622897878236));
#32853=CARTESIAN_POINT('',(-3.74449296983004,-1.,-0.203156094896101));
#32854=CARTESIAN_POINT('Ctrl Pts',(-4.19931119685982,-1.,-0.0760622897878246));
#32855=CARTESIAN_POINT('Ctrl Pts',(-4.1978913862118,-1.,-0.0767384596141464));
#32856=CARTESIAN_POINT('Ctrl Pts',(-4.19505112859416,-1.,-0.0780873956242397));
#32857=CARTESIAN_POINT('Ctrl Pts',(-4.19078883320504,-1.,-0.080100588711432));
#32858=CARTESIAN_POINT('Ctrl Pts',(-4.18510195327123,-1.,-0.0827644164385679));
#32859=CARTESIAN_POINT('Ctrl Pts',(-4.17798698668094,-1.,-0.0860600915549397));
#32860=CARTESIAN_POINT('Ctrl Pts',(-4.17086566490794,-1.,-0.0893215560848649));
#32861=CARTESIAN_POINT('Ctrl Pts',(-4.16373802265839,-1.,-0.0925486672167531));
#32862=CARTESIAN_POINT('Ctrl Pts',(-4.15660412653577,-1.,-0.0957412403298007));
#32863=CARTESIAN_POINT('Ctrl Pts',(-4.14946408918485,-1.,-0.0988990478901226));
#32864=CARTESIAN_POINT('Ctrl Pts',(-4.14231804939538,-1.,-0.102021826577584));
#32865=CARTESIAN_POINT('Ctrl Pts',(-4.13516614458895,-1.,-0.105109286538945));
#32866=CARTESIAN_POINT('Ctrl Pts',(-4.12800848371504,-1.,-0.108161120528369));
#32867=CARTESIAN_POINT('Ctrl Pts',(-4.1208451250225,-1.,-0.111177012683347));
#32868=CARTESIAN_POINT('Ctrl Pts',(-4.11367603924961,-1.,-0.114156649609546));
#32869=CARTESIAN_POINT('Ctrl Pts',(-4.10650113381833,-1.,-0.117099722731648));
#32870=CARTESIAN_POINT('Ctrl Pts',(-4.09932031767002,-1.,-0.120005924388124));
#32871=CARTESIAN_POINT('Ctrl Pts',(-4.09213355850756,-1.,-0.122874946249107));
#32872=CARTESIAN_POINT('Ctrl Pts',(-4.08494093372377,-1.,-0.12570647682254));
#32873=CARTESIAN_POINT('Ctrl Pts',(-4.07774270738954,-1.,-0.128500200484838));
#32874=CARTESIAN_POINT('Ctrl Pts',(-4.0705393152874,-1.,-0.13125579354894));
#32875=CARTESIAN_POINT('Ctrl Pts',(-4.06333121018596,-1.,-0.133972916144245));
#32876=CARTESIAN_POINT('Ctrl Pts',(-4.05611873400172,-1.,-0.136651205046119));
#32877=CARTESIAN_POINT('Ctrl Pts',(-4.04890199238036,-1.,-0.139290267180057));
#32878=CARTESIAN_POINT('Ctrl Pts',(-4.04168069633781,-1.,-0.1418896714855));
#32879=CARTESIAN_POINT('Ctrl Pts',(-4.03445411510333,-1.,-0.144448947038345));
#32880=CARTESIAN_POINT('Ctrl Pts',(-4.02722143146994,-1.,-0.146967602878994));
#32881=CARTESIAN_POINT('Ctrl Pts',(-4.01998203715564,-1.,-0.149445144968707));
#32882=CARTESIAN_POINT('Ctrl Pts',(-4.01273584234689,-1.,-0.151881094022911));
#32883=CARTESIAN_POINT('Ctrl Pts',(-4.00548360245319,-1.,-0.154275004872311));
#32884=CARTESIAN_POINT('Ctrl Pts',(-3.99822717425893,-1.,-0.156626481393734));
#32885=CARTESIAN_POINT('Ctrl Pts',(-3.99096873945878,-1.,-0.158935123982793));
#32886=CARTESIAN_POINT('Ctrl Pts',(-3.98371010319872,-1.,-0.161200482186085));
#32887=CARTESIAN_POINT('Ctrl Pts',(-3.97645194630943,-1.,-0.163422004609999));
#32888=CARTESIAN_POINT('Ctrl Pts',(-3.96919313621407,-1.,-0.165598992851102));
#32889=CARTESIAN_POINT('Ctrl Pts',(-3.96192990160296,-1.,-0.167730547023319));
#32890=CARTESIAN_POINT('Ctrl Pts',(-3.95465744665268,-1.,-0.169815666374139));
#32891=CARTESIAN_POINT('Ctrl Pts',(-3.94737164900868,-1.,-0.17185335536924));
#32892=CARTESIAN_POINT('Ctrl Pts',(-3.94007083096217,-1.,-0.17384273497461));
#32893=CARTESIAN_POINT('Ctrl Pts',(-3.93275726771042,-1.,-0.175783136893868));
#32894=CARTESIAN_POINT('Ctrl Pts',(-3.92543942697655,-1.,-0.177674246152317));
#32895=CARTESIAN_POINT('Ctrl Pts',(-3.91812876180926,-1.,-0.179515885822882));
#32896=CARTESIAN_POINT('Ctrl Pts',(-3.91083557557175,-1.,-0.181307740731786));
#32897=CARTESIAN_POINT('Ctrl Pts',(-3.90356488555132,-1.,-0.183049081993191));
#32898=CARTESIAN_POINT('Ctrl Pts',(-3.89631300742646,-1.,-0.184738537728043));
#32899=CARTESIAN_POINT('Ctrl Pts',(-3.88906196725848,-1.,-0.18637372498528));
#32900=CARTESIAN_POINT('Ctrl Pts',(-3.88178563496228,-1.,-0.187951632512685));
#32901=CARTESIAN_POINT('Ctrl Pts',(-3.87445976418412,-1.,-0.189469253358272));
#32902=CARTESIAN_POINT('Ctrl Pts',(-3.86707158624783,-1.,-0.19092419041862));
#32903=CARTESIAN_POINT('Ctrl Pts',(-3.85962774407633,-1.,-0.192315153044971));
#32904=CARTESIAN_POINT('Ctrl Pts',(-3.85216762263966,-1.,-0.193642806777723));
#32905=CARTESIAN_POINT('Ctrl Pts',(-3.84475203346977,-1.,-0.194909009460221));
#32906=CARTESIAN_POINT('Ctrl Pts',(-3.83743910616195,-1.,-0.196115198971859));
#32907=CARTESIAN_POINT('Ctrl Pts',(-3.83026221776456,-1.,-0.197260935827361));
#32908=CARTESIAN_POINT('Ctrl Pts',(-3.82321127349016,-1.,-0.198342616900486));
#32909=CARTESIAN_POINT('Ctrl Pts',(-3.81620203429815,-1.,-0.199351525297447));
#32910=CARTESIAN_POINT('Ctrl Pts',(-3.80909529318669,-1.,-0.200274679433364));
#32911=CARTESIAN_POINT('Ctrl Pts',(-3.80175247447337,-1.,-0.201097756307326));
#32912=CARTESIAN_POINT('Ctrl Pts',(-3.7940835418736,-1.,-0.201807533800837));
#32913=CARTESIAN_POINT('Ctrl Pts',(-3.78609175019242,-1.,-0.20239426051216));
#32914=CARTESIAN_POINT('Ctrl Pts',(-3.77793553476614,-1.,-0.202854729699081));
#32915=CARTESIAN_POINT('Ctrl Pts',(-3.7699207159487,-1.,-0.203192390045164));
#32916=CARTESIAN_POINT('Ctrl Pts',(-3.76242717936885,-1.,-0.203414634707478));
#32917=CARTESIAN_POINT('Ctrl Pts',(-3.75585118707734,-1.,-0.203530796848322));
#32918=CARTESIAN_POINT('Ctrl Pts',(-3.75054693397875,-1.,-0.203550035479166));
#32919=CARTESIAN_POINT('Ctrl Pts',(-3.74703926501752,-1.,-0.203484186269415));
#32920=CARTESIAN_POINT('Ctrl Pts',(-3.74535749969115,-1.,-0.203375226874121));
#32921=CARTESIAN_POINT('Ctrl Pts',(-3.74471097893845,-1.,-0.203266610110531));
#32922=CARTESIAN_POINT('Ctrl Pts',(-3.74453008995092,-1.,-0.203188003946657));
#32923=CARTESIAN_POINT('Ctrl Pts',(-3.74449296983004,-1.,-0.203156094896101));
#32924=CARTESIAN_POINT('',(-3.73017266276651,-1.,-0.385112848330762));
#32925=CARTESIAN_POINT('Origin',(0.,-1.,0.));
#32926=CARTESIAN_POINT('',(-4.15950947128175,-1.,-0.581791163835815));
#32927=CARTESIAN_POINT('Ctrl Pts',(-3.73017266276651,-1.,-0.385112848330762));
#32928=CARTESIAN_POINT('Ctrl Pts',(-3.73021431755274,-1.,-0.385087139000374));
#32929=CARTESIAN_POINT('Ctrl Pts',(-3.73040527621055,-1.,-0.385037797881504));
#32930=CARTESIAN_POINT('Ctrl Pts',(-3.73106082862548,-1.,-0.385031656499164));
#32931=CARTESIAN_POINT('Ctrl Pts',(-3.73273893363406,-1.,-0.385187124634206));
#32932=CARTESIAN_POINT('Ctrl Pts',(-3.73621371845318,-1.,-0.385670806454566));
#32933=CARTESIAN_POINT('Ctrl Pts',(-3.74144965781276,-1.,-0.386519576222251));
#32934=CARTESIAN_POINT('Ctrl Pts',(-3.74792651696654,-1.,-0.387663020050836));
#32935=CARTESIAN_POINT('Ctrl Pts',(-3.75529302895152,-1.,-0.389054775898702));
#32936=CARTESIAN_POINT('Ctrl Pts',(-3.76315635033257,-1.,-0.39064207297956));
#32937=CARTESIAN_POINT('Ctrl Pts',(-3.77114011595967,-1.,-0.392372786223432));
#32938=CARTESIAN_POINT('Ctrl Pts',(-3.77894173114283,-1.,-0.394202481011499));
#32939=CARTESIAN_POINT('Ctrl Pts',(-3.78640521279313,-1.,-0.396103205334841));
#32940=CARTESIAN_POINT('Ctrl Pts',(-3.7935288716329,-1.,-0.398064818683969));
#32941=CARTESIAN_POINT('Ctrl Pts',(-3.80040370384546,-1.,-0.4000883465046));
#32942=CARTESIAN_POINT('Ctrl Pts',(-3.80716881962728,-1.,-0.402181320148436));
#32943=CARTESIAN_POINT('Ctrl Pts',(-3.81396374287793,-1.,-0.404352694628273));
#32944=CARTESIAN_POINT('Ctrl Pts',(-3.8208730391381,-1.,-0.406607038258985));
#32945=CARTESIAN_POINT('Ctrl Pts',(-3.82790724256471,-1.,-0.40894237144746));
#32946=CARTESIAN_POINT('Ctrl Pts',(-3.83503345578698,-1.,-0.411353038798518));
#32947=CARTESIAN_POINT('Ctrl Pts',(-3.84219403994762,-1.,-0.413831367016748));
#32948=CARTESIAN_POINT('Ctrl Pts',(-3.84932864157497,-1.,-0.416369678052907));
#32949=CARTESIAN_POINT('Ctrl Pts',(-3.85639825647996,-1.,-0.418962468086773));
#32950=CARTESIAN_POINT('Ctrl Pts',(-3.86339652542709,-1.,-0.421607423177534));
#32951=CARTESIAN_POINT('Ctrl Pts',(-3.87033643487851,-1.,-0.424304173195111));
#32952=CARTESIAN_POINT('Ctrl Pts',(-3.87724240306597,-1.,-0.427053541173457));
#32953=CARTESIAN_POINT('Ctrl Pts',(-3.88414070943341,-1.,-0.429856640579741));
#32954=CARTESIAN_POINT('Ctrl Pts',(-3.89104947940611,-1.,-0.432713929544458));
#32955=CARTESIAN_POINT('Ctrl Pts',(-3.89797256655462,-1.,-0.435624629433527));
#32956=CARTESIAN_POINT('Ctrl Pts',(-3.90490512938563,-1.,-0.438587235458249));
#32957=CARTESIAN_POINT('Ctrl Pts',(-3.91183704069153,-1.,-0.441599824524054));
#32958=CARTESIAN_POINT('Ctrl Pts',(-3.91875701610719,-1.,-0.444660430230591));
#32959=CARTESIAN_POINT('Ctrl Pts',(-3.92565674143416,-1.,-0.447767416837292));
#32960=CARTESIAN_POINT('Ctrl Pts',(-3.93253407403123,-1.,-0.450919768356348));
#32961=CARTESIAN_POINT('Ctrl Pts',(-3.93939080846298,-1.,-0.454116879027584));
#32962=CARTESIAN_POINT('Ctrl Pts',(-3.94623117206678,-1.,-0.457358410451683));
#32963=CARTESIAN_POINT('Ctrl Pts',(-3.95306005817364,-1.,-0.460644124429121));
#32964=CARTESIAN_POINT('Ctrl Pts',(-3.95988133243538,-1.,-0.463973722115733));
#32965=CARTESIAN_POINT('Ctrl Pts',(-3.9666962227393,-1.,-0.467346690880643));
#32966=CARTESIAN_POINT('Ctrl Pts',(-3.97350414289392,-1.,-0.470762379613439));
#32967=CARTESIAN_POINT('Ctrl Pts',(-3.98030338044409,-1.,-0.47422006101951));
#32968=CARTESIAN_POINT('Ctrl Pts',(-3.98709184306738,-1.,-0.477718999122027));
#32969=CARTESIAN_POINT('Ctrl Pts',(-3.99386775880679,-1.,-0.481258512209675));
#32970=CARTESIAN_POINT('Ctrl Pts',(-4.00063045119288,-1.,-0.484838042421835));
#32971=CARTESIAN_POINT('Ctrl Pts',(-4.0073800839099,-1.,-0.488457130424633));
#32972=CARTESIAN_POINT('Ctrl Pts',(-4.01411733503546,-1.,-0.492115383418018));
#32973=CARTESIAN_POINT('Ctrl Pts',(-4.02084308851832,-1.,-0.495812444326251));
#32974=CARTESIAN_POINT('Ctrl Pts',(-4.02755813980101,-1.,-0.499547962340821));
#32975=CARTESIAN_POINT('Ctrl Pts',(-4.03426284174272,-1.,-0.503321556915346));
#32976=CARTESIAN_POINT('Ctrl Pts',(-4.04095715148915,-1.,-0.507132823288136));
#32977=CARTESIAN_POINT('Ctrl Pts',(-4.04764078815447,-1.,-0.51098134921897));
#32978=CARTESIAN_POINT('Ctrl Pts',(-4.05431335771199,-1.,-0.514866728193017));
#32979=CARTESIAN_POINT('Ctrl Pts',(-4.06097448038013,-1.,-0.518788572336923));
#32980=CARTESIAN_POINT('Ctrl Pts',(-4.06762394471314,-1.,-0.522746528603107));
#32981=CARTESIAN_POINT('Ctrl Pts',(-4.07426172299847,-1.,-0.526740277227498));
#32982=CARTESIAN_POINT('Ctrl Pts',(-4.08088789536836,-1.,-0.530769518728571));
#32983=CARTESIAN_POINT('Ctrl Pts',(-4.08750259988885,-1.,-0.534833963477273));
#32984=CARTESIAN_POINT('Ctrl Pts',(-4.09410597627,-1.,-0.538933321179756));
#32985=CARTESIAN_POINT('Ctrl Pts',(-4.10069810243979,-1.,-0.543067286877757));
#32986=CARTESIAN_POINT('Ctrl Pts',(-4.10727897027977,-1.,-0.547235539485637));
#32987=CARTESIAN_POINT('Ctrl Pts',(-4.11384852024721,-1.,-0.551437758497032));
#32988=CARTESIAN_POINT('Ctrl Pts',(-4.12040666195664,-1.,-0.555673636129977));
#32989=CARTESIAN_POINT('Ctrl Pts',(-4.12695329951961,-1.,-0.559942890594773));
#32990=CARTESIAN_POINT('Ctrl Pts',(-4.13348835727104,-1.,-0.564245279537148));
#32991=CARTESIAN_POINT('Ctrl Pts',(-4.14001179830547,-1.,-0.568580610189774));
#32992=CARTESIAN_POINT('Ctrl Pts',(-4.14652361068081,-1.,-0.572948736069522));
#32993=CARTESIAN_POINT('Ctrl Pts',(-4.151723761217,-1.,-0.576469391676688));
#32994=CARTESIAN_POINT('Ctrl Pts',(-4.15561864788576,-1.,-0.579124568914235));
#32995=CARTESIAN_POINT('Ctrl Pts',(-4.1582129171283,-1.,-0.580901211463535));
#32996=CARTESIAN_POINT('Ctrl Pts',(-4.15950947128175,-1.,-0.581791163835815));
#32997=CARTESIAN_POINT('',(-4.13571194405636,-1.,-0.73204283740062));
#32998=CARTESIAN_POINT('',(-4.15950947128175,-1.,-0.581791163835815));
#32999=CARTESIAN_POINT('',(-3.66661143271685,-1.,-0.786422660831985));
#33000=CARTESIAN_POINT('Ctrl Pts',(-4.13571194405636,-1.,-0.73204283740062));
#33001=CARTESIAN_POINT('Ctrl Pts',(-4.1342038373684,-1.,-0.732488575135159));
#33002=CARTESIAN_POINT('Ctrl Pts',(-4.13118752795207,-1.,-0.733376589323546));
#33003=CARTESIAN_POINT('Ctrl Pts',(-4.12666277570844,-1.,-0.734698226764092));
#33004=CARTESIAN_POINT('Ctrl Pts',(-4.120629196238,-1.,-0.736439634331345));
#33005=CARTESIAN_POINT('Ctrl Pts',(-4.11308626951927,-1.,-0.738581708225844));
#33006=CARTESIAN_POINT('Ctrl Pts',(-4.10554241757547,-1.,-0.740688998553377));
#33007=CARTESIAN_POINT('Ctrl Pts',(-4.09799769702611,-1.,-0.742761369689841));
#33008=CARTESIAN_POINT('Ctrl Pts',(-4.09045220253573,-1.,-0.7447986497065));
#33009=CARTESIAN_POINT('Ctrl Pts',(-4.08290608095642,-1.,-0.746800631492315));
#33010=CARTESIAN_POINT('Ctrl Pts',(-4.07535951056152,-1.,-0.748767076680557));
#33011=CARTESIAN_POINT('Ctrl Pts',(-4.06781267242378,-1.,-0.750697720484036));
#33012=CARTESIAN_POINT('Ctrl Pts',(-4.06026572221515,-1.,-0.752592276483072));
#33013=CARTESIAN_POINT('Ctrl Pts',(-4.05271876687915,-1.,-0.754450441816078));
#33014=CARTESIAN_POINT('Ctrl Pts',(-4.04517182653997,-1.,-0.756271902369581));
#33015=CARTESIAN_POINT('Ctrl Pts',(-4.03762485803119,-1.,-0.758056338884944));
#33016=CARTESIAN_POINT('Ctrl Pts',(-4.03007781954412,-1.,-0.759803433243752));
#33017=CARTESIAN_POINT('Ctrl Pts',(-4.02253072741268,-1.,-0.761512875859804));
#33018=CARTESIAN_POINT('Ctrl Pts',(-4.01498370680496,-1.,-0.763184371182935));
#33019=CARTESIAN_POINT('Ctrl Pts',(-4.00743706791509,-1.,-0.764817648785197));
#33020=CARTESIAN_POINT('Ctrl Pts',(-3.99989129179622,-1.,-0.766412457136064));
#33021=CARTESIAN_POINT('Ctrl Pts',(-3.9923468788101,-1.,-0.767968531377915));
#33022=CARTESIAN_POINT('Ctrl Pts',(-3.98480422348451,-1.,-0.769485566245544));
#33023=CARTESIAN_POINT('Ctrl Pts',(-3.97726349165488,-1.,-0.770963190030471));
#33024=CARTESIAN_POINT('Ctrl Pts',(-3.96972446532772,-1.,-0.772400931772136));
#33025=CARTESIAN_POINT('Ctrl Pts',(-3.96218649639807,-1.,-0.773798212026565));
#33026=CARTESIAN_POINT('Ctrl Pts',(-3.9546488545231,-1.,-0.775154418039351));
#33027=CARTESIAN_POINT('Ctrl Pts',(-3.94711101619447,-1.,-0.776468966697921));
#33028=CARTESIAN_POINT('Ctrl Pts',(-3.93957296768103,-1.,-0.777741370568558));
#33029=CARTESIAN_POINT('Ctrl Pts',(-3.93203552473174,-1.,-0.778971308134821));
#33030=CARTESIAN_POINT('Ctrl Pts',(-3.92450058323823,-1.,-0.780158678615542));
#33031=CARTESIAN_POINT('Ctrl Pts',(-3.91697036054676,-1.,-0.781303428618366));
#33032=CARTESIAN_POINT('Ctrl Pts',(-3.90944671004542,-1.,-0.782405395622764));
#33033=CARTESIAN_POINT('Ctrl Pts',(-3.9019303904397,-1.,-0.783464141529081));
#33034=CARTESIAN_POINT('Ctrl Pts',(-3.89442039235103,-1.,-0.784478799358336));
#33035=CARTESIAN_POINT('Ctrl Pts',(-3.88691313167398,-1.,-0.78544789034073));
#33036=CARTESIAN_POINT('Ctrl Pts',(-3.8794040281819,-1.,-0.786369675812608));
#33037=CARTESIAN_POINT('Ctrl Pts',(-3.87188916600912,-1.,-0.787242527617999));
#33038=CARTESIAN_POINT('Ctrl Pts',(-3.86436702561345,-1.,-0.788065315093777));
#33039=CARTESIAN_POINT('Ctrl Pts',(-3.85683995872529,-1.,-0.788837734090672));
#33040=CARTESIAN_POINT('Ctrl Pts',(-3.84931637808894,-1.,-0.789560798155582));
#33041=CARTESIAN_POINT('Ctrl Pts',(-3.84180762342454,-1.,-0.790236124191242));
#33042=CARTESIAN_POINT('Ctrl Pts',(-3.83432392054786,-1.,-0.790865012705301));
#33043=CARTESIAN_POINT('Ctrl Pts',(-3.82687033899792,-1.,-0.791447528662369));
#33044=CARTESIAN_POINT('Ctrl Pts',(-3.81944345442249,-1.,-0.791981740718635));
#33045=CARTESIAN_POINT('Ctrl Pts',(-3.81202588694756,-1.,-0.792462483517634));
#33046=CARTESIAN_POINT('Ctrl Pts',(-3.80459229925637,-1.,-0.792882695234778));
#33047=CARTESIAN_POINT('Ctrl Pts',(-3.79711921389897,-1.,-0.793235612973273));
#33048=CARTESIAN_POINT('Ctrl Pts',(-3.78959439439235,-1.,-0.793516871680993));
#33049=CARTESIAN_POINT('Ctrl Pts',(-3.78202460377598,-1.,-0.7937262357813));
#33050=CARTESIAN_POINT('Ctrl Pts',(-3.77444863801212,-1.,-0.793870523787408));
#33051=CARTESIAN_POINT('Ctrl Pts',(-3.76692626931111,-1.,-0.793961083688991));
#33052=CARTESIAN_POINT('Ctrl Pts',(-3.75951468666257,-1.,-0.794008429134907));
#33053=CARTESIAN_POINT('Ctrl Pts',(-3.75224692493864,-1.,-0.794017347371377));
#33054=CARTESIAN_POINT('Ctrl Pts',(-3.74511357728861,-1.,-0.793982700459952));
#33055=CARTESIAN_POINT('Ctrl Pts',(-3.73803280541687,-1.,-0.793882700937017));
#33056=CARTESIAN_POINT('Ctrl Pts',(-3.73086914695805,-1.,-0.793682750269684));
#33057=CARTESIAN_POINT('Ctrl Pts',(-3.72348797293734,-1.,-0.793347023784205));
#33058=CARTESIAN_POINT('Ctrl Pts',(-3.71580242396124,-1.,-0.792848377370287));
#33059=CARTESIAN_POINT('Ctrl Pts',(-3.70781724021806,-1.,-0.792177688845818));
#33060=CARTESIAN_POINT('Ctrl Pts',(-3.69968940808721,-1.,-0.79135657569598));
#33061=CARTESIAN_POINT('Ctrl Pts',(-3.69172044327364,-1.,-0.790436284988787));
#33062=CARTESIAN_POINT('Ctrl Pts',(-3.68428439783905,-1.,-0.789483546064387));
#33063=CARTESIAN_POINT('Ctrl Pts',(-3.67777119516252,-1.,-0.788569566220285));
#33064=CARTESIAN_POINT('Ctrl Pts',(-3.67252923663655,-1.,-0.787758799995742));
#33065=CARTESIAN_POINT('Ctrl Pts',(-3.66907505398677,-1.,-0.787145041181545));
#33066=CARTESIAN_POINT('Ctrl Pts',(-3.66743103898702,-1.,-0.786774337198062));
#33067=CARTESIAN_POINT('Ctrl Pts',(-3.66680946938292,-1.,-0.786565919558984));
#33068=CARTESIAN_POINT('Ctrl Pts',(-3.6666431041522,-1.,-0.786459983895432));
#33069=CARTESIAN_POINT('Ctrl Pts',(-3.66661143271685,-1.,-0.786422660831985));
#33070=CARTESIAN_POINT('',(-3.62400312501245,-1.,-0.963899035117249));
#33071=CARTESIAN_POINT('Origin',(0.,-1.,0.));
#33072=CARTESIAN_POINT('',(-4.01728681790024,-1.,-1.22531898815164));
#33073=CARTESIAN_POINT('Ctrl Pts',(-3.62400312501245,-1.,-0.963899035117249));
#33074=CARTESIAN_POINT('Ctrl Pts',(-3.6240482887845,-1.,-0.963880158555582));
#33075=CARTESIAN_POINT('Ctrl Pts',(-3.62424461507588,-1.,-0.963861297423241));
#33076=CARTESIAN_POINT('Ctrl Pts',(-3.62489305727662,-1.,-0.963957782642843));
#33077=CARTESIAN_POINT('Ctrl Pts',(-3.62652618145335,-1.,-0.964373850166457));
#33078=CARTESIAN_POINT('Ctrl Pts',(-3.62988252139846,-1.,-0.965395153165293));
#33079=CARTESIAN_POINT('Ctrl Pts',(-3.63492122081143,-1.,-0.967052554541385));
#33080=CARTESIAN_POINT('Ctrl Pts',(-3.64113946505766,-1.,-0.969195124675865));
#33081=CARTESIAN_POINT('Ctrl Pts',(-3.64819756447455,-1.,-0.971722122061341));
#33082=CARTESIAN_POINT('Ctrl Pts',(-3.65571576735126,-1.,-0.974519971354848));
#33083=CARTESIAN_POINT('Ctrl Pts',(-3.66333049637475,-1.,-0.977478312751618));
#33084=CARTESIAN_POINT('Ctrl Pts',(-3.67074983340361,-1.,-0.980505922458267));
#33085=CARTESIAN_POINT('Ctrl Pts',(-3.67782408841715,-1.,-0.983550791470419));
#33086=CARTESIAN_POINT('Ctrl Pts',(-3.68455317926068,-1.,-0.986602639863837));
#33087=CARTESIAN_POINT('Ctrl Pts',(-3.69102682138846,-1.,-0.989676715398558));
#33088=CARTESIAN_POINT('Ctrl Pts',(-3.69738123415662,-1.,-0.99280221833201));
#33089=CARTESIAN_POINT('Ctrl Pts',(-3.70375282282138,-1.,-0.996009819772518));
#33090=CARTESIAN_POINT('Ctrl Pts',(-3.71022439713938,-1.,-0.99931726075653));
#33091=CARTESIAN_POINT('Ctrl Pts',(-3.71680667125118,-1.,-1.00272423396822));
#33092=CARTESIAN_POINT('Ctrl Pts',(-3.72346803750595,-1.,-1.0062200073571));
#33093=CARTESIAN_POINT('Ctrl Pts',(-3.73015276704426,-1.,-1.00978798539496));
#33094=CARTESIAN_POINT('Ctrl Pts',(-3.73680245055734,-1.,-1.01341114319903));
#33095=CARTESIAN_POINT('Ctrl Pts',(-3.74337942504959,-1.,-1.01707794311079));
#33096=CARTESIAN_POINT('Ctrl Pts',(-3.74987777155834,-1.,-1.02078510487428));
#33097=CARTESIAN_POINT('Ctrl Pts',(-3.75631037456194,-1.,-1.0245342944466));
#33098=CARTESIAN_POINT('Ctrl Pts',(-3.76270122291232,-1.,-1.02833014458181));
#33099=CARTESIAN_POINT('Ctrl Pts',(-3.76907609832522,-1.,-1.0321778660492));
#33100=CARTESIAN_POINT('Ctrl Pts',(-3.77545283140445,-1.,-1.03608074678013));
#33101=CARTESIAN_POINT('Ctrl Pts',(-3.78183535008192,-1.,-1.04003862055804));
#33102=CARTESIAN_POINT('Ctrl Pts',(-3.78821910787195,-1.,-1.04404924374426));
#33103=CARTESIAN_POINT('Ctrl Pts',(-3.79459440308793,-1.,-1.04810913267641));
#33104=CARTESIAN_POINT('Ctrl Pts',(-3.80095039790678,-1.,-1.05221457990015));
#33105=CARTESIAN_POINT('Ctrl Pts',(-3.80727913637784,-1.,-1.05636266918643));
#33106=CARTESIAN_POINT('Ctrl Pts',(-3.81357866117485,-1.,-1.06055206187298));
#33107=CARTESIAN_POINT('Ctrl Pts',(-3.81985083953012,-1.,-1.06478244038931));
#33108=CARTESIAN_POINT('Ctrl Pts',(-3.82609989967278,-1.,-1.0690541318036));
#33109=CARTESIAN_POINT('Ctrl Pts',(-3.83233071195145,-1.,-1.0733676663346));
#33110=CARTESIAN_POINT('Ctrl Pts',(-3.83854714117486,-1.,-1.07772335353856));
#33111=CARTESIAN_POINT('Ctrl Pts',(-3.84475048030615,-1.,-1.08212087917986));
#33112=CARTESIAN_POINT('Ctrl Pts',(-3.8509402522269,-1.,-1.08655950846377));
#33113=CARTESIAN_POINT('Ctrl Pts',(-3.85711487933911,-1.,-1.09103825516288));
#33114=CARTESIAN_POINT('Ctrl Pts',(-3.86327241021242,-1.,-1.09555606505012));
#33115=CARTESIAN_POINT('Ctrl Pts',(-3.86941120134872,-1.,-1.10011198761202));
#33116=CARTESIAN_POINT('Ctrl Pts',(-3.87553067187566,-1.,-1.10470536603303));
#33117=CARTESIAN_POINT('Ctrl Pts',(-3.88163105531791,-1.,-1.10933577224029));
#33118=CARTESIAN_POINT('Ctrl Pts',(-3.88771308285229,-1.,-1.11400292434447));
#33119=CARTESIAN_POINT('Ctrl Pts',(-3.89377768340362,-1.,-1.11870660794609));
#33120=CARTESIAN_POINT('Ctrl Pts',(-3.89982569749978,-1.,-1.12344660099029));
#33121=CARTESIAN_POINT('Ctrl Pts',(-3.90585753318622,-1.,-1.12822258281518));
#33122=CARTESIAN_POINT('Ctrl Pts',(-3.91187321145495,-1.,-1.13303414693849));
#33123=CARTESIAN_POINT('Ctrl Pts',(-3.91787251936688,-1.,-1.13788084225511));
#33124=CARTESIAN_POINT('Ctrl Pts',(-3.92385513133937,-1.,-1.14276220561575));
#33125=CARTESIAN_POINT('Ctrl Pts',(-3.92982073294334,-1.,-1.14767779451147));
#33126=CARTESIAN_POINT('Ctrl Pts',(-3.9357691705651,-1.,-1.1526272271639));
#33127=CARTESIAN_POINT('Ctrl Pts',(-3.94170046685542,-1.,-1.1576101834106));
#33128=CARTESIAN_POINT('Ctrl Pts',(-3.9476147478092,-1.,-1.16262637999261));
#33129=CARTESIAN_POINT('Ctrl Pts',(-3.95351219510062,-1.,-1.16767555244495));
#33130=CARTESIAN_POINT('Ctrl Pts',(-3.95939299213164,-1.,-1.17275743590327));
#33131=CARTESIAN_POINT('Ctrl Pts',(-3.96525726357682,-1.,-1.17787174135445));
#33132=CARTESIAN_POINT('Ctrl Pts',(-3.9711050516465,-1.,-1.18301815039596));
#33133=CARTESIAN_POINT('Ctrl Pts',(-3.97693634766926,-1.,-1.18819633715285));
#33134=CARTESIAN_POINT('Ctrl Pts',(-3.98275111052015,-1.,-1.19340598349307));
#33135=CARTESIAN_POINT('Ctrl Pts',(-3.98854928957287,-1.,-1.19864679609596));
#33136=CARTESIAN_POINT('Ctrl Pts',(-3.99433084800649,-1.,-1.2039185237544));
#33137=CARTESIAN_POINT('Ctrl Pts',(-4.00009577952534,-1.,-1.20922097030107));
#33138=CARTESIAN_POINT('Ctrl Pts',(-4.00584409524937,-1.,-1.21455398918813));
#33139=CARTESIAN_POINT('Ctrl Pts',(-4.01042947142681,-1.,-1.21884478244983));
#33140=CARTESIAN_POINT('Ctrl Pts',(-4.01386104434674,-1.,-1.22207656456199));
#33141=CARTESIAN_POINT('Ctrl Pts',(-4.0161454457032,-1.,-1.22423716681447));
#33142=CARTESIAN_POINT('Ctrl Pts',(-4.01728681790024,-1.,-1.22531898815164));
#33143=CARTESIAN_POINT('',(-3.97027773754922,-1.,-1.36999806084572));
#33144=CARTESIAN_POINT('',(-4.01728681790024,-1.,-1.22531898815164));
#33145=CARTESIAN_POINT('',(-3.4984457533445,-1.,-1.35032489087101));
#33146=CARTESIAN_POINT('Ctrl Pts',(-3.97027773754922,-1.,-1.36999806084572));
#33147=CARTESIAN_POINT('Ctrl Pts',(-3.9687184694131,-1.,-1.37020239094614));
#33148=CARTESIAN_POINT('Ctrl Pts',(-3.96560037974645,-1.,-1.37060761745635));
#33149=CARTESIAN_POINT('Ctrl Pts',(-3.96092458506535,-1.,-1.3712051561502));
#33150=CARTESIAN_POINT('Ctrl Pts',(-3.95469287280914,-1.,-1.37198126432386));
#33151=CARTESIAN_POINT('Ctrl Pts',(-3.94690771785133,-1.,-1.37291699202807));
#33152=CARTESIAN_POINT('Ctrl Pts',(-3.93912709040818,-1.,-1.37381821967165));
#33153=CARTESIAN_POINT('Ctrl Pts',(-3.93135106761844,-1.,-1.37468482215751));
#33154=CARTESIAN_POINT('Ctrl Pts',(-3.92357976987672,-1.,-1.37551664448242));
#33155=CARTESIAN_POINT('Ctrl Pts',(-3.91581337462644,-1.,-1.37631350505797));
#33156=CARTESIAN_POINT('Ctrl Pts',(-3.90805209523486,-1.,-1.3770751963402));
#33157=CARTESIAN_POINT('Ctrl Pts',(-3.90029615196727,-1.,-1.37780148512792));
#33158=CARTESIAN_POINT('Ctrl Pts',(-3.89254574338496,-1.,-1.3784921128802));
#33159=CARTESIAN_POINT('Ctrl Pts',(-3.88480102249277,-1.,-1.37914679719383));
#33160=CARTESIAN_POINT('Ctrl Pts',(-3.87706205830532,-1.,-1.37976523097073));
#33161=CARTESIAN_POINT('Ctrl Pts',(-3.86932885813068,-1.,-1.38034709213014));
#33162=CARTESIAN_POINT('Ctrl Pts',(-3.86160143043959,-1.,-1.38089205992989));
#33163=CARTESIAN_POINT('Ctrl Pts',(-3.85387983979481,-1.,-1.38139983115049));
#33164=CARTESIAN_POINT('Ctrl Pts',(-3.84616425605764,-1.,-1.38187013346109));
#33165=CARTESIAN_POINT('Ctrl Pts',(-3.83845502790746,-1.,-1.38230274828821));
#33166=CARTESIAN_POINT('Ctrl Pts',(-3.8307526698229,-1.,-1.38269750245138));
#33167=CARTESIAN_POINT('Ctrl Pts',(-3.82305771743829,-1.,-1.38305421262763));
#33168=CARTESIAN_POINT('Ctrl Pts',(-3.81537060817811,-1.,-1.38337263902782));
#33169=CARTESIAN_POINT('Ctrl Pts',(-3.80769156398411,-1.,-1.3836524404622));
#33170=CARTESIAN_POINT('Ctrl Pts',(-3.80002044322111,-1.,-1.38389311766682));
#33171=CARTESIAN_POINT('Ctrl Pts',(-3.79235669640841,-1.,-1.38409399694566));
#33172=CARTESIAN_POINT('Ctrl Pts',(-3.78469969805082,-1.,-1.38425435883756));
#33173=CARTESIAN_POINT('Ctrl Pts',(-3.77704902230418,-1.,-1.38437354551428));
#33174=CARTESIAN_POINT('Ctrl Pts',(-3.76940473185779,-1.,-1.38445107339518));
#33175=CARTESIAN_POINT('Ctrl Pts',(-3.76176768271367,-1.,-1.3844867525335));
#33176=CARTESIAN_POINT('Ctrl Pts',(-3.7541397631875,-1.,-1.38448077997163));
#33177=CARTESIAN_POINT('Ctrl Pts',(-3.74652317167876,-1.,-1.38443344984394));
#33178=CARTESIAN_POINT('Ctrl Pts',(-3.73891976418104,-1.,-1.38434489156458));
#33179=CARTESIAN_POINT('Ctrl Pts',(-3.73133035859282,-1.,-1.38421479111531));
#33180=CARTESIAN_POINT('Ctrl Pts',(-3.72375409358803,-1.,-1.3840421342895));
#33181=CARTESIAN_POINT('Ctrl Pts',(-3.7161876605181,-1.,-1.38382489984586));
#33182=CARTESIAN_POINT('Ctrl Pts',(-3.70862680753347,-1.,-1.38356065402124));
#33183=CARTESIAN_POINT('Ctrl Pts',(-3.701067921679,-1.,-1.38324717612865));
#33184=CARTESIAN_POINT('Ctrl Pts',(-3.69350967899526,-1.,-1.3828831117165));
#33185=CARTESIAN_POINT('Ctrl Pts',(-3.68595444983837,-1.,-1.38246852827182));
#33186=CARTESIAN_POINT('Ctrl Pts',(-3.67841038482414,-1.,-1.3820057429062));
#33187=CARTESIAN_POINT('Ctrl Pts',(-3.67088843112262,-1.,-1.38149812653868));
#33188=CARTESIAN_POINT('Ctrl Pts',(-3.66339848520857,-1.,-1.38094856333552));
#33189=CARTESIAN_POINT('Ctrl Pts',(-3.6559455440439,-1.,-1.38035791051212));
#33190=CARTESIAN_POINT('Ctrl Pts',(-3.64852652756456,-1.,-1.37972372481603));
#33191=CARTESIAN_POINT('Ctrl Pts',(-3.64112507791141,-1.,-1.37903818567359));
#33192=CARTESIAN_POINT('Ctrl Pts',(-3.63371727442486,-1.,-1.37829035457339));
#33193=CARTESIAN_POINT('Ctrl Pts',(-3.62628098665145,-1.,-1.37746987919881));
#33194=CARTESIAN_POINT('Ctrl Pts',(-3.6188048116042,-1.,-1.37657053403107));
#33195=CARTESIAN_POINT('Ctrl Pts',(-3.61129546591064,-1.,-1.37559314436634));
#33196=CARTESIAN_POINT('Ctrl Pts',(-3.60379020123988,-1.,-1.37455051379623));
#33197=CARTESIAN_POINT('Ctrl Pts',(-3.59634627869048,-1.,-1.37346320103157));
#33198=CARTESIAN_POINT('Ctrl Pts',(-3.58901853846365,-1.,-1.37235053660976));
#33199=CARTESIAN_POINT('Ctrl Pts',(-3.58183885982715,-1.,-1.37122241663062));
#33200=CARTESIAN_POINT('Ctrl Pts',(-3.57479875549486,-1.,-1.37007229485659));
#33201=CARTESIAN_POINT('Ctrl Pts',(-3.5678208030466,-1.,-1.36886584973389));
#33202=CARTESIAN_POINT('Ctrl Pts',(-3.56077662028649,-1.,-1.36754771771233));
#33203=CARTESIAN_POINT('Ctrl Pts',(-3.55353883995949,-1.,-1.3660614545677));
#33204=CARTESIAN_POINT('Ctrl Pts',(-3.54602591832973,-1.,-1.36436666257597));
#33205=CARTESIAN_POINT('Ctrl Pts',(-3.53824396424961,-1.,-1.36245507339307));
#33206=CARTESIAN_POINT('Ctrl Pts',(-3.530344649616,-1.,-1.36037259643734));
#33207=CARTESIAN_POINT('Ctrl Pts',(-3.52261776116748,-1.,-1.35821701528836));
#33208=CARTESIAN_POINT('Ctrl Pts',(-3.51542230699556,-1.,-1.35611275237152));
#33209=CARTESIAN_POINT('Ctrl Pts',(-3.50913227059999,-1.,-1.35419113575956));
#33210=CARTESIAN_POINT('Ctrl Pts',(-3.50408168106261,-1.,-1.35257032843486));
#33211=CARTESIAN_POINT('Ctrl Pts',(-3.5007660381649,-1.,-1.35142377279517));
#33212=CARTESIAN_POINT('Ctrl Pts',(-3.49920025459723,-1.,-1.35080045218587));
#33213=CARTESIAN_POINT('Ctrl Pts',(-3.49861894124827,-1.,-1.35049736560527));
#33214=CARTESIAN_POINT('Ctrl Pts',(-3.49847119623846,-1.,-1.35036670892966));
#33215=CARTESIAN_POINT('Ctrl Pts',(-3.4984457533445,-1.,-1.35032489087101));
#33216=CARTESIAN_POINT('',(-3.42859860294378,-1.,-1.51895082866166));
#33217=CARTESIAN_POINT('Origin',(0.,-1.,0.));
#33218=CARTESIAN_POINT('',(-3.77614523045147,-1.,-1.83867539237861));
#33219=CARTESIAN_POINT('Ctrl Pts',(-3.42859860294378,-1.,-1.51895082866166));
#33220=CARTESIAN_POINT('Ctrl Pts',(-3.42864616361967,-1.,-1.51893924967231));
#33221=CARTESIAN_POINT('Ctrl Pts',(-3.42884302333978,-1.,-1.51895133295017));
#33222=CARTESIAN_POINT('Ctrl Pts',(-3.42946838852728,-1.,-1.51914806898539));
#33223=CARTESIAN_POINT('Ctrl Pts',(-3.43101631893491,-1.,-1.5198144909343));
#33224=CARTESIAN_POINT('Ctrl Pts',(-3.43417156977749,-1.,-1.52134826724227));
#33225=CARTESIAN_POINT('Ctrl Pts',(-3.43888895974182,-1.,-1.52377348950429));
#33226=CARTESIAN_POINT('Ctrl Pts',(-3.44469547527,-1.,-1.52686242875717));
#33227=CARTESIAN_POINT('Ctrl Pts',(-3.45127136828667,-1.,-1.530462444618));
#33228=CARTESIAN_POINT('Ctrl Pts',(-3.45825932955273,-1.,-1.53440195378902));
#33229=CARTESIAN_POINT('Ctrl Pts',(-3.46531752207222,-1.,-1.53851507915533));
#33230=CARTESIAN_POINT('Ctrl Pts',(-3.47217189224576,-1.,-1.54266605398152));
#33231=CARTESIAN_POINT('Ctrl Pts',(-3.47868272898599,-1.,-1.54678009290206));
#33232=CARTESIAN_POINT('Ctrl Pts',(-3.48485155928414,-1.,-1.55084702970382));
#33233=CARTESIAN_POINT('Ctrl Pts',(-3.49076460877317,-1.,-1.5548959590107));
#33234=CARTESIAN_POINT('Ctrl Pts',(-3.49655185179623,-1.,-1.55897703097859));
#33235=CARTESIAN_POINT('Ctrl Pts',(-3.50234321621607,-1.,-1.56314187758689));
#33236=CARTESIAN_POINT('Ctrl Pts',(-3.50821771695427,-1.,-1.56742097575041));
#33237=CARTESIAN_POINT('Ctrl Pts',(-3.51418598431733,-1.,-1.57181569799774));
#33238=CARTESIAN_POINT('Ctrl Pts',(-3.52021847865961,-1.,-1.5763104998818));
#33239=CARTESIAN_POINT('Ctrl Pts',(-3.52626275334899,-1.,-1.58088027227856));
#33240=CARTESIAN_POINT('Ctrl Pts',(-3.53226378147068,-1.,-1.58549906268083));
#33241=CARTESIAN_POINT('Ctrl Pts',(-3.53818616861045,-1.,-1.59014958368725));
#33242=CARTESIAN_POINT('Ctrl Pts',(-3.544024581823,-1.,-1.5948276694975));
#33243=CARTESIAN_POINT('Ctrl Pts',(-3.54979148634426,-1.,-1.59953698113444));
#33244=CARTESIAN_POINT('Ctrl Pts',(-3.55550985096117,-1.,-1.60428584699848));
#33245=CARTESIAN_POINT('Ctrl Pts',(-3.56120432482986,-1.,-1.60908344685459));
#33246=CARTESIAN_POINT('Ctrl Pts',(-3.56689200468404,-1.,-1.61393581747522));
#33247=CARTESIAN_POINT('Ctrl Pts',(-3.57257679609826,-1.,-1.61884340915412));
#33248=CARTESIAN_POINT('Ctrl Pts',(-3.57825455954405,-1.,-1.62380329464851));
#33249=CARTESIAN_POINT('Ctrl Pts',(-3.5839162577435,-1.,-1.62881051550748));
#33250=CARTESIAN_POINT('Ctrl Pts',(-3.58955176627876,-1.,-1.63385971451259));
#33251=CARTESIAN_POINT('Ctrl Pts',(-3.59515368334887,-1.,-1.63894676675349));
#33252=CARTESIAN_POINT('Ctrl Pts',(-3.6007202851384,-1.,-1.6440700438558));
#33253=CARTESIAN_POINT('Ctrl Pts',(-3.60625346556992,-1.,-1.64922952425833));
#33254=CARTESIAN_POINT('Ctrl Pts',(-3.61175734965129,-1.,-1.65442619244327));
#33255=CARTESIAN_POINT('Ctrl Pts',(-3.61723666482457,-1.,-1.65966133399186));
#33256=CARTESIAN_POINT('Ctrl Pts',(-3.62269517989104,-1.,-1.66493585923853));
#33257=CARTESIAN_POINT('Ctrl Pts',(-3.62813422105257,-1.,-1.67024966008037));
#33258=CARTESIAN_POINT('Ctrl Pts',(-3.63355343201211,-1.,-1.67560193613145));
#33259=CARTESIAN_POINT('Ctrl Pts',(-3.63895140887443,-1.,-1.68099146651577));
#33260=CARTESIAN_POINT('Ctrl Pts',(-3.64432638915199,-1.,-1.68641690471455));
#33261=CARTESIAN_POINT('Ctrl Pts',(-3.64967689827393,-1.,-1.691877054817));
#33262=CARTESIAN_POINT('Ctrl Pts',(-3.65500246526798,-1.,-1.69737117722558));
#33263=CARTESIAN_POINT('Ctrl Pts',(-3.6603033877491,-1.,-1.70289888566904));
#33264=CARTESIAN_POINT('Ctrl Pts',(-3.6655804319893,-1.,-1.70846001610983));
#33265=CARTESIAN_POINT('Ctrl Pts',(-3.67083454901629,-1.,-1.71405450210392));
#33266=CARTESIAN_POINT('Ctrl Pts',(-3.67606660374665,-1.,-1.71968225581787));
#33267=CARTESIAN_POINT('Ctrl Pts',(-3.68127704936472,-1.,-1.72534302437003));
#33268=CARTESIAN_POINT('Ctrl Pts',(-3.68646597019188,-1.,-1.73103640956647));
#33269=CARTESIAN_POINT('Ctrl Pts',(-3.69163322647906,-1.,-1.73676193254493));
#33270=CARTESIAN_POINT('Ctrl Pts',(-3.6967785691046,-1.,-1.74251908492589));
#33271=CARTESIAN_POINT('Ctrl Pts',(-3.70190175673422,-1.,-1.74830738046092));
#33272=CARTESIAN_POINT('Ctrl Pts',(-3.70700269736876,-1.,-1.75412641804148));
#33273=CARTESIAN_POINT('Ctrl Pts',(-3.71208146346454,-1.,-1.75997588499021));
#33274=CARTESIAN_POINT('Ctrl Pts',(-3.71713822377675,-1.,-1.76585552124549));
#33275=CARTESIAN_POINT('Ctrl Pts',(-3.72217319911429,-1.,-1.77176509401846));
#33276=CARTESIAN_POINT('Ctrl Pts',(-3.72718661205504,-1.,-1.77770437039606));
#33277=CARTESIAN_POINT('Ctrl Pts',(-3.73217863095022,-1.,-1.78367308442682));
#33278=CARTESIAN_POINT('Ctrl Pts',(-3.73714934729962,-1.,-1.78967092823139));
#33279=CARTESIAN_POINT('Ctrl Pts',(-3.74209880351667,-1.,-1.79569757859041));
#33280=CARTESIAN_POINT('Ctrl Pts',(-3.74702700874954,-1.,-1.80175271485519));
#33281=CARTESIAN_POINT('Ctrl Pts',(-3.75193395888069,-1.,-1.80783603939662));
#33282=CARTESIAN_POINT('Ctrl Pts',(-3.75681965683995,-1.,-1.81394729834032));
#33283=CARTESIAN_POINT('Ctrl Pts',(-3.76168412709652,-1.,-1.82008629694924));
#33284=CARTESIAN_POINT('Ctrl Pts',(-3.76652740355856,-1.,-1.82625289221933));
#33285=CARTESIAN_POINT('Ctrl Pts',(-3.77038509819777,-1.,-1.83120816956515));
#33286=CARTESIAN_POINT('Ctrl Pts',(-3.77326886065484,-1.,-1.83493697935064));
#33287=CARTESIAN_POINT('Ctrl Pts',(-3.77518714458232,-1.,-1.83742834010821));
#33288=CARTESIAN_POINT('Ctrl Pts',(-3.77614523045147,-1.,-1.83867539237861));
#33289=CARTESIAN_POINT('',(-3.70708211654725,-1.,-1.97421938526992));
#33290=CARTESIAN_POINT('',(-3.77614523045147,-1.,-1.83867539237861));
#33291=CARTESIAN_POINT('',(-3.24413672884902,-1.,-1.88097764062542));
#33292=CARTESIAN_POINT('Ctrl Pts',(-3.70708211654725,-1.,-1.97421938526992));
#33293=CARTESIAN_POINT('Ctrl Pts',(-3.7055100813194,-1.,-1.974177276451));
#33294=CARTESIAN_POINT('Ctrl Pts',(-3.70236698911837,-1.,-1.97408973726149));
#33295=CARTESIAN_POINT('Ctrl Pts',(-3.69765528558292,-1.,-1.97394846382288));
#33296=CARTESIAN_POINT('Ctrl Pts',(-3.69137888597855,-1.,-1.97374016224397));
#33297=CARTESIAN_POINT('Ctrl Pts',(-3.68354319913416,-1.,-1.9734465030363));
#33298=CARTESIAN_POINT('Ctrl Pts',(-3.67571738106175,-1.,-1.97311947678035));
#33299=CARTESIAN_POINT('Ctrl Pts',(-3.66790152751984,-1.,-1.9727589719863));
#33300=CARTESIAN_POINT('Ctrl Pts',(-3.66009578166865,-1.,-1.97236485439317));
#33301=CARTESIAN_POINT('Ctrl Pts',(-3.65230034717364,-1.,-1.97193697240645));
#33302=CARTESIAN_POINT('Ctrl Pts',(-3.64451546724221,-1.,-1.97147515441539));
#33303=CARTESIAN_POINT('Ctrl Pts',(-3.63674139590853,-1.,-1.97097920454698));
#33304=CARTESIAN_POINT('Ctrl Pts',(-3.62897836973397,-1.,-1.97044889850518));
#33305=CARTESIAN_POINT('Ctrl Pts',(-3.62122658401722,-1.,-1.96988398129888));
#33306=CARTESIAN_POINT('Ctrl Pts',(-3.61348615496393,-1.,-1.96928416040712));
#33307=CARTESIAN_POINT('Ctrl Pts',(-3.60575714017676,-1.,-1.96864911885775));
#33308=CARTESIAN_POINT('Ctrl Pts',(-3.59803959819725,-1.,-1.96797854118257));
#33309=CARTESIAN_POINT('Ctrl Pts',(-3.5903336402273,-1.,-1.96727213799507));
#33310=CARTESIAN_POINT('Ctrl Pts',(-3.58263947663884,-1.,-1.9665296668894));
#33311=CARTESIAN_POINT('Ctrl Pts',(-3.57495748601088,-1.,-1.96575096652857));
#33312=CARTESIAN_POINT('Ctrl Pts',(-3.56728820357933,-1.,-1.96493594634643));
#33313=CARTESIAN_POINT('Ctrl Pts',(-3.55963218706201,-1.,-1.96408450906868));
#33314=CARTESIAN_POINT('Ctrl Pts',(-3.55198990600929,-1.,-1.96319648628667));
#33315=CARTESIAN_POINT('Ctrl Pts',(-3.54436163300425,-1.,-1.96227157573058));
#33316=CARTESIAN_POINT('Ctrl Pts',(-3.53674730625759,-1.,-1.96130926212661));
#33317=CARTESIAN_POINT('Ctrl Pts',(-3.52914648844289,-1.,-1.96030879411534));
#33318=CARTESIAN_POINT('Ctrl Pts',(-3.52155867431438,-1.,-1.95926936324436));
#33319=CARTESIAN_POINT('Ctrl Pts',(-3.51398354617772,-1.,-1.95819025316768));
#33320=CARTESIAN_POINT('Ctrl Pts',(-3.50642124159913,-1.,-1.95707099606513));
#33321=CARTESIAN_POINT('Ctrl Pts',(-3.49887263575602,-1.,-1.9559115382367));
#33322=CARTESIAN_POINT('Ctrl Pts',(-3.49133956289154,-1.,-1.95471236969653));
#33323=CARTESIAN_POINT('Ctrl Pts',(-3.48382414832648,-1.,-1.95347412486316));
#33324=CARTESIAN_POINT('Ctrl Pts',(-3.47632820495926,-1.,-1.95219722189878));
#33325=CARTESIAN_POINT('Ctrl Pts',(-3.4688525897419,-1.,-1.95088147859876));
#33326=CARTESIAN_POINT('Ctrl Pts',(-3.46139661060959,-1.,-1.94952575850196));
#33327=CARTESIAN_POINT('Ctrl Pts',(-3.45395731584051,-1.,-1.94812754766524));
#33328=CARTESIAN_POINT('Ctrl Pts',(-3.44653088665685,-1.,-1.94668377715332));
#33329=CARTESIAN_POINT('Ctrl Pts',(-3.43911410197693,-1.,-1.94519168842883));
#33330=CARTESIAN_POINT('Ctrl Pts',(-3.43170586602436,-1.,-1.94364973660285));
#33331=CARTESIAN_POINT('Ctrl Pts',(-3.42430850941497,-1.,-1.94205835913692));
#33332=CARTESIAN_POINT('Ctrl Pts',(-3.41692971994082,-1.,-1.94042111965237));
#33333=CARTESIAN_POINT('Ctrl Pts',(-3.40957978266622,-1.,-1.93874306008132));
#33334=CARTESIAN_POINT('Ctrl Pts',(-3.40226802104093,-1.,-1.93702857723089));
#33335=CARTESIAN_POINT('Ctrl Pts',(-3.39499923640789,-1.,-1.93527929945982));
#33336=CARTESIAN_POINT('Ctrl Pts',(-3.38777076883267,-1.,-1.93349233176794));
#33337=CARTESIAN_POINT('Ctrl Pts',(-3.38056768525577,-1.,-1.93165739093292));
#33338=CARTESIAN_POINT('Ctrl Pts',(-3.37336807068078,-1.,-1.92975993109897));
#33339=CARTESIAN_POINT('Ctrl Pts',(-3.36615168657597,-1.,-1.92778626543803));
#33340=CARTESIAN_POINT('Ctrl Pts',(-3.35890824422976,-1.,-1.92572846125763));
#33341=CARTESIAN_POINT('Ctrl Pts',(-3.35164424847206,-1.,-1.92358838440518));
#33342=CARTESIAN_POINT('Ctrl Pts',(-3.34439448941915,-1.,-1.92138450828378));
#33343=CARTESIAN_POINT('Ctrl Pts',(-3.33721230709948,-1.,-1.91914609610173));
#33344=CARTESIAN_POINT('Ctrl Pts',(-3.33014884257812,-1.,-1.91690081930297));
#33345=CARTESIAN_POINT('Ctrl Pts',(-3.32323403454507,-1.,-1.91466343916612));
#33346=CARTESIAN_POINT('Ctrl Pts',(-3.31646052426395,-1.,-1.91242616234459));
#33347=CARTESIAN_POINT('Ctrl Pts',(-3.30975721158694,-1.,-1.91014297830502));
#33348=CARTESIAN_POINT('Ctrl Pts',(-3.30300595568341,-1.,-1.90773912171424));
#33349=CARTESIAN_POINT('Ctrl Pts',(-3.29608978722258,-1.,-1.9051389186417));
#33350=CARTESIAN_POINT('Ctrl Pts',(-3.28893448600364,-1.,-1.9022897124757));
#33351=CARTESIAN_POINT('Ctrl Pts',(-3.28154737912287,-1.,-1.89918429230424));
#33352=CARTESIAN_POINT('Ctrl Pts',(-3.27407108932908,-1.,-1.89589172903662));
#33353=CARTESIAN_POINT('Ctrl Pts',(-3.2667765388833,-1.,-1.89255393500769));
#33354=CARTESIAN_POINT('Ctrl Pts',(-3.2599988519361,-1.,-1.88934996203508));
#33355=CARTESIAN_POINT('Ctrl Pts',(-3.25408686339298,-1.,-1.88646802523372));
#33356=CARTESIAN_POINT('Ctrl Pts',(-3.24935200512055,-1.,-1.88407708646435));
#33357=CARTESIAN_POINT('Ctrl Pts',(-3.24625654410705,-1.,-1.88242596600422));
#33358=CARTESIAN_POINT('Ctrl Pts',(-3.24480754675942,-1.,-1.88156537699118));
#33359=CARTESIAN_POINT('Ctrl Pts',(-3.24428080352952,-1.,-1.88117508446657));
#33360=CARTESIAN_POINT('Ctrl Pts',(-3.24415531671311,-1.,-1.88102292397987));
#33361=CARTESIAN_POINT('Ctrl Pts',(-3.24413672884902,-1.,-1.88097764062542));
#33362=CARTESIAN_POINT('',(-3.14877060440425,-1.,-2.03660101169564));
#33363=CARTESIAN_POINT('Origin',(0.,-1.,0.));
#33364=CARTESIAN_POINT('',(-3.44202241512147,-1.,-2.40675750623143));
#33365=CARTESIAN_POINT('Ctrl Pts',(-3.14877060440425,-1.,-2.03660101169564));
#33366=CARTESIAN_POINT('Ctrl Pts',(-3.1488193908823,-1.,-2.03659701539175));
#33367=CARTESIAN_POINT('Ctrl Pts',(-3.14901193669147,-1.,-2.03663974554941));
#33368=CARTESIAN_POINT('Ctrl Pts',(-3.14959882629936,-1.,-2.03693188810614));
#33369=CARTESIAN_POINT('Ctrl Pts',(-3.15102344775396,-1.,-2.03783225496023));
#33370=CARTESIAN_POINT('Ctrl Pts',(-3.1538999167466,-1.,-2.03984073791432));
#33371=CARTESIAN_POINT('Ctrl Pts',(-3.15817983946525,-1.,-2.04297406404132));
#33372=CARTESIAN_POINT('Ctrl Pts',(-3.16343165059235,-1.,-2.0469333124766));
#33373=CARTESIAN_POINT('Ctrl Pts',(-3.16936341689859,-1.,-2.05151770247452));
#33374=CARTESIAN_POINT('Ctrl Pts',(-3.17564906975592,-1.,-2.05650186773279));
#33375=CARTESIAN_POINT('Ctrl Pts',(-3.18197692964677,-1.,-2.06166849827143));
#33376=CARTESIAN_POINT('Ctrl Pts',(-3.18809755562297,-1.,-2.06684062744065));
#33377=CARTESIAN_POINT('Ctrl Pts',(-3.19388465568113,-1.,-2.07192253497765));
#33378=CARTESIAN_POINT('Ctrl Pts',(-3.19934132835879,-1.,-2.0769044187063));
#33379=CARTESIAN_POINT('Ctrl Pts',(-3.20454818630635,-1.,-2.08182850370816));
#33380=CARTESIAN_POINT('Ctrl Pts',(-3.20962575845433,-1.,-2.08676465517435));
#33381=CARTESIAN_POINT('Ctrl Pts',(-3.2146942960168,-1.,-2.0917841946046));
#33382=CARTESIAN_POINT('Ctrl Pts',(-3.21982707347067,-1.,-2.09692958434933));
#33383=CARTESIAN_POINT('Ctrl Pts',(-3.22503437553496,-1.,-2.10220384298533));
#33384=CARTESIAN_POINT('Ctrl Pts',(-3.23028945793334,-1.,-2.1075869964248));
#33385=CARTESIAN_POINT('Ctrl Pts',(-3.23554444767115,-1.,-2.11304604021784));
#33386=CARTESIAN_POINT('Ctrl Pts',(-3.24074905517282,-1.,-2.11854673326972));
#33387=CARTESIAN_POINT('Ctrl Pts',(-3.24587102613347,-1.,-2.12406646410943));
#33388=CARTESIAN_POINT('Ctrl Pts',(-3.25090574493994,-1.,-2.1296002839681));
#33389=CARTESIAN_POINT('Ctrl Pts',(-3.25586495065027,-1.,-2.13515375878786));
#33390=CARTESIAN_POINT('Ctrl Pts',(-3.26077002641868,-1.,-2.14073870754257));
#33391=CARTESIAN_POINT('Ctrl Pts',(-3.26564388189764,-1.,-2.14636805295663));
#33392=CARTESIAN_POINT('Ctrl Pts',(-3.27050245897244,-1.,-2.15205043199818));
#33393=CARTESIAN_POINT('Ctrl Pts',(-3.27534954469206,-1.,-2.15778690038359));
#33394=CARTESIAN_POINT('Ctrl Pts',(-3.28018150841414,-1.,-2.16357391934434));
#33395=CARTESIAN_POINT('Ctrl Pts',(-3.2849901997973,-1.,-2.16940517773459));
#33396=CARTESIAN_POINT('Ctrl Pts',(-3.28976645712566,-1.,-2.17527380048422));
#33397=CARTESIAN_POINT('Ctrl Pts',(-3.29450361500484,-1.,-2.18117455557062));
#33398=CARTESIAN_POINT('Ctrl Pts',(-3.29920022557635,-1.,-2.18710556500325));
#33399=CARTESIAN_POINT('Ctrl Pts',(-3.30385816281831,-1.,-2.19306710376112));
#33400=CARTESIAN_POINT('Ctrl Pts',(-3.30848134694596,-1.,-2.19906078949924));
#33401=CARTESIAN_POINT('Ctrl Pts',(-3.3130742460895,-1.,-2.20508863150608));
#33402=CARTESIAN_POINT('Ctrl Pts',(-3.31764044024231,-1.,-2.21115211847872));
#33403=CARTESIAN_POINT('Ctrl Pts',(-3.32218125618955,-1.,-2.21725135110889));
#33404=CARTESIAN_POINT('Ctrl Pts',(-3.32669646722871,-1.,-2.22338548312758));
#33405=CARTESIAN_POINT('Ctrl Pts',(-3.33118487773593,-1.,-2.22955308907221));
#33406=CARTESIAN_POINT('Ctrl Pts',(-3.33564495756478,-1.,-2.2357525632881));
#33407=CARTESIAN_POINT('Ctrl Pts',(-3.34007543738044,-1.,-2.24198249391437));
#33408=CARTESIAN_POINT('Ctrl Pts',(-3.34447596770768,-1.,-2.24824207678288));
#33409=CARTESIAN_POINT('Ctrl Pts',(-3.34884690292342,-1.,-2.25453097693524));
#33410=CARTESIAN_POINT('Ctrl Pts',(-3.35318902552676,-1.,-2.26084915222484));
#33411=CARTESIAN_POINT('Ctrl Pts',(-3.35750328523077,-1.,-2.26719668579921));
#33412=CARTESIAN_POINT('Ctrl Pts',(-3.36179055004369,-1.,-2.27357362620902));
#33413=CARTESIAN_POINT('Ctrl Pts',(-3.36605130712978,-1.,-2.27997979457968));
#33414=CARTESIAN_POINT('Ctrl Pts',(-3.37028570206357,-1.,-2.28641481081045));
#33415=CARTESIAN_POINT('Ctrl Pts',(-3.37449367172707,-1.,-2.2928781800731));
#33416=CARTESIAN_POINT('Ctrl Pts',(-3.37867504959382,-1.,-2.29936936127588));
#33417=CARTESIAN_POINT('Ctrl Pts',(-3.38282967336676,-1.,-2.30588783640389));
#33418=CARTESIAN_POINT('Ctrl Pts',(-3.38695751492659,-1.,-2.31243319489505));
#33419=CARTESIAN_POINT('Ctrl Pts',(-3.39105869475112,-1.,-2.31900513925627));
#33420=CARTESIAN_POINT('Ctrl Pts',(-3.39513342020045,-1.,-2.32560343902683));
#33421=CARTESIAN_POINT('Ctrl Pts',(-3.39918194578115,-1.,-2.33222789882601));
#33422=CARTESIAN_POINT('Ctrl Pts',(-3.40320452776646,-1.,-2.33887832342715));
#33423=CARTESIAN_POINT('Ctrl Pts',(-3.40720137403888,-1.,-2.34555447648901));
#33424=CARTESIAN_POINT('Ctrl Pts',(-3.41117262313464,-1.,-2.35225606823649));
#33425=CARTESIAN_POINT('Ctrl Pts',(-3.4151183675076,-1.,-2.35898278606449));
#33426=CARTESIAN_POINT('Ctrl Pts',(-3.41903866635384,-1.,-2.36573431470314));
#33427=CARTESIAN_POINT('Ctrl Pts',(-3.42293356216595,-1.,-2.37251035954351));
#33428=CARTESIAN_POINT('Ctrl Pts',(-3.42680309755241,-1.,-2.37931067029517));
#33429=CARTESIAN_POINT('Ctrl Pts',(-3.43064732714472,-1.,-2.38613505844641));
#33430=CARTESIAN_POINT('Ctrl Pts',(-3.43446630680436,-1.,-2.39298338805823));
#33431=CARTESIAN_POINT('Ctrl Pts',(-3.43750133066036,-1.,-2.39848113411429));
#33432=CARTESIAN_POINT('Ctrl Pts',(-3.43976627485223,-1.,-2.40261515590099));
#33433=CARTESIAN_POINT('Ctrl Pts',(-3.44127120683402,-1.,-2.40537592959345));
#33434=CARTESIAN_POINT('Ctrl Pts',(-3.44202241512147,-1.,-2.40675750623143));
#33435=CARTESIAN_POINT('',(-3.35260583073571,-1.,-2.52982887637028));
#33436=CARTESIAN_POINT('',(-3.44202241512147,-1.,-2.40675750623143));
#33437=CARTESIAN_POINT('',(-2.90994629141676,-1.,-2.36531447826073));
#33438=CARTESIAN_POINT('Ctrl Pts',(-3.35260583073571,-1.,-2.52982887637028));
#33439=CARTESIAN_POINT('Ctrl Pts',(-3.35105973714071,-1.,-2.5295413654909));
#33440=CARTESIAN_POINT('Ctrl Pts',(-3.34796903576663,-1.,-2.52896321610703));
#33441=CARTESIAN_POINT('Ctrl Pts',(-3.34333744115511,-1.,-2.52808660915689));
#33442=CARTESIAN_POINT('Ctrl Pts',(-3.33717089999103,-1.,-2.52689902690158));
#33443=CARTESIAN_POINT('Ctrl Pts',(-3.32947762187533,-1.,-2.52538321164634));
#33444=CARTESIAN_POINT('Ctrl Pts',(-3.32179931078699,-1.,-2.5238359839626));
#33445=CARTESIAN_POINT('Ctrl Pts',(-3.31413607874645,-1.,-2.52225724871313));
#33446=CARTESIAN_POINT('Ctrl Pts',(-3.30648808815442,-1.,-2.52064689568511));
#33447=CARTESIAN_POINT('Ctrl Pts',(-3.29885556388352,-1.,-2.51900480701069));
#33448=CARTESIAN_POINT('Ctrl Pts',(-3.2912387729927,-1.,-2.51733085123797));
#33449=CARTESIAN_POINT('Ctrl Pts',(-3.28363799702982,-1.,-2.51562487464514));
#33450=CARTESIAN_POINT('Ctrl Pts',(-3.27605350473142,-1.,-2.513886692704));
#33451=CARTESIAN_POINT('Ctrl Pts',(-3.26848552888115,-1.,-2.51211608411423));
#33452=CARTESIAN_POINT('Ctrl Pts',(-3.26093423001434,-1.,-2.51031277813486));
#33453=CARTESIAN_POINT('Ctrl Pts',(-3.25339971460982,-1.,-2.50847647070723));
#33454=CARTESIAN_POINT('Ctrl Pts',(-3.24588208983849,-1.,-2.506606859405));
#33455=CARTESIAN_POINT('Ctrl Pts',(-3.23838151080319,-1.,-2.5047036758003));
#33456=CARTESIAN_POINT('Ctrl Pts',(-3.23089822320646,-1.,-2.50276671338111));
#33457=CARTESIAN_POINT('Ctrl Pts',(-3.22343262620503,-1.,-2.50079587201957));
#33458=CARTESIAN_POINT('Ctrl Pts',(-3.21598526261286,-1.,-2.4987911459939));
#33459=CARTESIAN_POINT('Ctrl Pts',(-3.20855669849836,-1.,-2.4967525264737));
#33460=CARTESIAN_POINT('Ctrl Pts',(-3.20114742397588,-1.,-2.49467992057755));
#33461=CARTESIAN_POINT('Ctrl Pts',(-3.19375775555798,-1.,-2.49257307239848));
#33462=CARTESIAN_POINT('Ctrl Pts',(-3.18638771282266,-1.,-2.49043146334059));
#33463=CARTESIAN_POINT('Ctrl Pts',(-3.17903698136622,-1.,-2.48825428288201));
#33464=CARTESIAN_POINT('Ctrl Pts',(-3.17170518863313,-1.,-2.48604065348587));
#33465=CARTESIAN_POINT('Ctrl Pts',(-3.16439213290161,-1.,-2.48378981792725));
#33466=CARTESIAN_POINT('Ctrl Pts',(-3.15709802322739,-1.,-2.48150133566571));
#33467=CARTESIAN_POINT('Ctrl Pts',(-3.14982373241352,-1.,-2.47917529057029));
#33468=CARTESIAN_POINT('Ctrl Pts',(-3.1425709954655,-1.,-2.47681245356109));
#33469=CARTESIAN_POINT('Ctrl Pts',(-3.13534181229295,-1.,-2.47441378371932));
#33470=CARTESIAN_POINT('Ctrl Pts',(-3.12813790805952,-1.,-2.47197997765871));
#33471=CARTESIAN_POINT('Ctrl Pts',(-3.12096015766983,-1.,-2.46951098947469));
#33472=CARTESIAN_POINT('Ctrl Pts',(-3.11380805536122,-1.,-2.46700558843506));
#33473=CARTESIAN_POINT('Ctrl Pts',(-3.1066790790198,-1.,-2.46446082979646));
#33474=CARTESIAN_POINT('Ctrl Pts',(-3.09956993697052,-1.,-2.46187308501884));
#33475=CARTESIAN_POINT('Ctrl Pts',(-3.09247787931887,-1.,-2.4592391256388));
#33476=CARTESIAN_POINT('Ctrl Pts',(-3.08540206545315,-1.,-2.45655725437039));
#33477=CARTESIAN_POINT('Ctrl Pts',(-3.07834472886139,-1.,-2.4538282678779));
#33478=CARTESIAN_POINT('Ctrl Pts',(-3.07131290521297,-1.,-2.45105688854422));
#33479=CARTESIAN_POINT('Ctrl Pts',(-3.06431596421405,-1.,-2.44824970516544));
#33480=CARTESIAN_POINT('Ctrl Pts',(-3.05736242671506,-1.,-2.44541251892556));
#33481=CARTESIAN_POINT('Ctrl Pts',(-3.05045678021504,-1.,-2.44254768923105));
#33482=CARTESIAN_POINT('Ctrl Pts',(-3.04359685040555,-1.,-2.43965194061857));
#33483=CARTESIAN_POINT('Ctrl Pts',(-3.03676949672821,-1.,-2.43671278042414));
#33484=CARTESIAN_POINT('Ctrl Pts',(-3.02995534946978,-1.,-2.43371241361488));
#33485=CARTESIAN_POINT('Ctrl Pts',(-3.02313656036004,-1.,-2.43063415586637));
#33486=CARTESIAN_POINT('Ctrl Pts',(-3.01630420830504,-1.,-2.42746856264168));
#33487=CARTESIAN_POINT('Ctrl Pts',(-3.00946442616658,-1.,-2.42421849439613));
#33488=CARTESIAN_POINT('Ctrl Pts',(-3.00264868585996,-1.,-2.42090763946779));
#33489=CARTESIAN_POINT('Ctrl Pts',(-2.99590509293503,-1.,-2.41757324500514));
#33490=CARTESIAN_POINT('Ctrl Pts',(-2.98927983005796,-1.,-2.41425064199586));
#33491=CARTESIAN_POINT('Ctrl Pts',(-2.98280015815107,-1.,-2.41095909342571));
#33492=CARTESIAN_POINT('Ctrl Pts',(-2.97646002822422,-1.,-2.40768975073713));
#33493=CARTESIAN_POINT('Ctrl Pts',(-2.9701964131236,-1.,-2.40438604734919));
#33494=CARTESIAN_POINT('Ctrl Pts',(-2.96390432240312,-1.,-2.4009556571164));
#33495=CARTESIAN_POINT('Ctrl Pts',(-2.95748006482942,-1.,-2.39730553974517));
#33496=CARTESIAN_POINT('Ctrl Pts',(-2.95085857128439,-1.,-2.39337207631667));
#33497=CARTESIAN_POINT('Ctrl Pts',(-2.94404820669076,-1.,-2.38914929090759));
#33498=CARTESIAN_POINT('Ctrl Pts',(-2.93717903280391,-1.,-2.38472771516311));
#33499=CARTESIAN_POINT('Ctrl Pts',(-2.93049643640206,-1.,-2.38028989582073));
#33500=CARTESIAN_POINT('Ctrl Pts',(-2.92430340582608,-1.,-2.3760651052403));
#33501=CARTESIAN_POINT('Ctrl Pts',(-2.91891503791411,-1.,-2.37229381109821));
#33502=CARTESIAN_POINT('Ctrl Pts',(-2.9146124988314,-1.,-2.36919161373173));
#33503=CARTESIAN_POINT('Ctrl Pts',(-2.91181344022549,-1.,-2.36707658451664));
#33504=CARTESIAN_POINT('Ctrl Pts',(-2.91051690822156,-1.,-2.36599991765749));
#33505=CARTESIAN_POINT('Ctrl Pts',(-2.91005770527719,-1.,-2.36553202948613));
#33506=CARTESIAN_POINT('Ctrl Pts',(-2.90995756655606,-1.,-2.36536211188453));
#33507=CARTESIAN_POINT('Ctrl Pts',(-2.90994629141676,-1.,-2.36531447826074));
#33508=CARTESIAN_POINT('',(-2.79140942341378,-1.,-2.50410331873042));
#33509=CARTESIAN_POINT('Origin',(0.,-1.,0.));
#33510=CARTESIAN_POINT('',(-3.02314558451372,-1.,-2.91557726271063));
#33511=CARTESIAN_POINT('Ctrl Pts',(-2.79140942341378,-1.,-2.50410331873042));
#33512=CARTESIAN_POINT('Ctrl Pts',(-2.79145823440899,-1.,-2.50410700351426));
#33513=CARTESIAN_POINT('Ctrl Pts',(-2.79164172519039,-1.,-2.50417932839343));
#33514=CARTESIAN_POINT('Ctrl Pts',(-2.79217568804874,-1.,-2.50455968395235));
#33515=CARTESIAN_POINT('Ctrl Pts',(-2.79344192164204,-1.,-2.50567182569153));
#33516=CARTESIAN_POINT('Ctrl Pts',(-2.7959687805717,-1.,-2.50810555977564));
#33517=CARTESIAN_POINT('Ctrl Pts',(-2.79970585014308,-1.,-2.51186983687947));
#33518=CARTESIAN_POINT('Ctrl Pts',(-2.80427363984939,-1.,-2.51660190466067));
#33519=CARTESIAN_POINT('Ctrl Pts',(-2.80941521967234,-1.,-2.52205778589922));
#33520=CARTESIAN_POINT('Ctrl Pts',(-2.8148437904867,-1.,-2.52796388055457));
#33521=CARTESIAN_POINT('Ctrl Pts',(-2.82028550483744,-1.,-2.53405679667463));
#33522=CARTESIAN_POINT('Ctrl Pts',(-2.82552167649157,-1.,-2.54012272520141));
#33523=CARTESIAN_POINT('Ctrl Pts',(-2.83044254225794,-1.,-2.54604736792542));
#33524=CARTESIAN_POINT('Ctrl Pts',(-2.83505269592412,-1.,-2.55182152806964));
#33525=CARTESIAN_POINT('Ctrl Pts',(-2.83942515220699,-1.,-2.55749952145165));
#33526=CARTESIAN_POINT('Ctrl Pts',(-2.84366802680211,-1.,-2.56316920798489));
#33527=CARTESIAN_POINT('Ctrl Pts',(-2.84788893329091,-1.,-2.56891984251743));
#33528=CARTESIAN_POINT('Ctrl Pts',(-2.85215360144483,-1.,-2.57480482727128));
#33529=CARTESIAN_POINT('Ctrl Pts',(-2.85647171715147,-1.,-2.58082875254407));
#33530=CARTESIAN_POINT('Ctrl Pts',(-2.86081999003668,-1.,-2.5869677064356));
#33531=CARTESIAN_POINT('Ctrl Pts',(-2.86515629953528,-1.,-2.59318160184921));
#33532=CARTESIAN_POINT('Ctrl Pts',(-2.86943633170712,-1.,-2.59942875223202));
#33533=CARTESIAN_POINT('Ctrl Pts',(-2.87363176656475,-1.,-2.6056817788128));
#33534=CARTESIAN_POINT('Ctrl Pts',(-2.87773881947885,-1.,-2.61193507170928));
#33535=CARTESIAN_POINT('Ctrl Pts',(-2.88176821427502,-1.,-2.61819596473087));
#33536=CARTESIAN_POINT('Ctrl Pts',(-2.88573922195049,-1.,-2.62447947640253));
#33537=CARTESIAN_POINT('Ctrl Pts',(-2.88967244854243,-1.,-2.63080195420771));
#33538=CARTESIAN_POINT('Ctrl Pts',(-2.89358228854557,-1.,-2.63717442263944));
#33539=CARTESIAN_POINT('Ctrl Pts',(-2.89747231723361,-1.,-2.64359851684146));
#33540=CARTESIAN_POINT('Ctrl Pts',(-2.90133950224879,-1.,-2.65007017365576));
#33541=CARTESIAN_POINT('Ctrl Pts',(-2.90517678087467,-1.,-2.65658188464287));
#33542=CARTESIAN_POINT('Ctrl Pts',(-2.90897617968921,-1.,-2.66312542616808));
#33543=CARTESIAN_POINT('Ctrl Pts',(-2.91273193382876,-1.,-2.66969458792627));
#33544=CARTESIAN_POINT('Ctrl Pts',(-2.91644290704281,-1.,-2.67628728855309));
#33545=CARTESIAN_POINT('Ctrl Pts',(-2.92011090722152,-1.,-2.68290409279689));
#33546=CARTESIAN_POINT('Ctrl Pts',(-2.92373955325876,-1.,-2.68954721165342));
#33547=CARTESIAN_POINT('Ctrl Pts',(-2.92733294395268,-1.,-2.69621932864302));
#33548=CARTESIAN_POINT('Ctrl Pts',(-2.93089438233746,-1.,-2.70292247416881));
#33549=CARTESIAN_POINT('Ctrl Pts',(-2.93442516311168,-1.,-2.70965695523776));
#33550=CARTESIAN_POINT('Ctrl Pts',(-2.93792519474955,-1.,-2.71642190053575));
#33551=CARTESIAN_POINT('Ctrl Pts',(-2.94139351933882,-1.,-2.72321571511322));
#33552=CARTESIAN_POINT('Ctrl Pts',(-2.94482887675139,-1.,-2.73003657371613));
#33553=CARTESIAN_POINT('Ctrl Pts',(-2.94823023414381,-1.,-2.73688288329825));
#33554=CARTESIAN_POINT('Ctrl Pts',(-2.95159737214305,-1.,-2.7437537949221));
#33555=CARTESIAN_POINT('Ctrl Pts',(-2.95493069316211,-1.,-2.75064903318996));
#33556=CARTESIAN_POINT('Ctrl Pts',(-2.9582309766594,-1.,-2.75756867888393));
#33557=CARTESIAN_POINT('Ctrl Pts',(-2.96149914764832,-1.,-2.76451296269571));
#33558=CARTESIAN_POINT('Ctrl Pts',(-2.96473605585548,-1.,-2.77148206836464));
#33559=CARTESIAN_POINT('Ctrl Pts',(-2.9679422104295,-1.,-2.77847589542767));
#33560=CARTESIAN_POINT('Ctrl Pts',(-2.97111781461349,-1.,-2.78549409123657));
#33561=CARTESIAN_POINT('Ctrl Pts',(-2.97426288347475,-1.,-2.79253615718147));
#33562=CARTESIAN_POINT('Ctrl Pts',(-2.97737733718242,-1.,-2.79960153278186));
#33563=CARTESIAN_POINT('Ctrl Pts',(-2.98046109647299,-1.,-2.80668968101162));
#33564=CARTESIAN_POINT('Ctrl Pts',(-2.9835141977994,-1.,-2.81380019196454));
#33565=CARTESIAN_POINT('Ctrl Pts',(-2.98653680669434,-1.,-2.82093279065704));
#33566=CARTESIAN_POINT('Ctrl Pts',(-2.98952916401699,-1.,-2.82808728190402));
#33567=CARTESIAN_POINT('Ctrl Pts',(-2.99249155170479,-1.,-2.83526351254383));
#33568=CARTESIAN_POINT('Ctrl Pts',(-2.995424253416,-1.,-2.84246132984334));
#33569=CARTESIAN_POINT('Ctrl Pts',(-2.99832751144566,-1.,-2.84968053289104));
#33570=CARTESIAN_POINT('Ctrl Pts',(-3.0012015079552,-1.,-2.85692085715129));
#33571=CARTESIAN_POINT('Ctrl Pts',(-3.00404638316245,-1.,-2.86418200833065));
#33572=CARTESIAN_POINT('Ctrl Pts',(-3.00686224485374,-1.,-2.87146368430104));
#33573=CARTESIAN_POINT('Ctrl Pts',(-3.0096491810855,-1.,-2.87876560072799));
#33574=CARTESIAN_POINT('Ctrl Pts',(-3.01240727309568,-1.,-2.88608751706796));
#33575=CARTESIAN_POINT('Ctrl Pts',(-3.01513660433291,-1.,-2.8934292556764));
#33576=CARTESIAN_POINT('Ctrl Pts',(-3.01783725123646,-1.,-2.90079069102661));
#33577=CARTESIAN_POINT('Ctrl Pts',(-3.01997487194926,-1.,-2.90669553303902));
#33578=CARTESIAN_POINT('Ctrl Pts',(-3.02156522743299,-1.,-2.91113297349052));
#33579=CARTESIAN_POINT('Ctrl Pts',(-3.02261975104912,-1.,-2.91409518070707));
#33580=CARTESIAN_POINT('Ctrl Pts',(-3.02314558451372,-1.,-2.91557726271063));
#33581=CARTESIAN_POINT('',(-2.91557726271063,-1.,-3.02314558451372));
#33582=CARTESIAN_POINT('',(-3.02314558451372,-1.,-2.91557726271063));
#33583=CARTESIAN_POINT('',(-2.50410331873176,-1.,-2.79140942341258));
#33584=CARTESIAN_POINT('Ctrl Pts',(-2.91557726271063,-1.,-3.02314558451372));
#33585=CARTESIAN_POINT('Ctrl Pts',(-2.91409518070399,-1.,-3.02261975104593));
#33586=CARTESIAN_POINT('Ctrl Pts',(-2.91113297348212,-1.,-3.02156522742431));
#33587=CARTESIAN_POINT('Ctrl Pts',(-2.90669553302526,-1.,-3.01997487193503));
#33588=CARTESIAN_POINT('Ctrl Pts',(-2.9007906910105,-1.,-3.01783725121981));
#33589=CARTESIAN_POINT('Ctrl Pts',(-2.89342925566321,-1.,-3.01513660431928));
#33590=CARTESIAN_POINT('Ctrl Pts',(-2.8860875170608,-1.,-3.01240727308829));
#33591=CARTESIAN_POINT('Ctrl Pts',(-2.87876560072727,-1.,-3.00964918108476));
#33592=CARTESIAN_POINT('Ctrl Pts',(-2.87146368430502,-1.,-3.00686224485784));
#33593=CARTESIAN_POINT('Ctrl Pts',(-2.86418200833667,-1.,-3.00404638316867));
#33594=CARTESIAN_POINT('Ctrl Pts',(-2.85692085715686,-1.,-3.00120150796095));
#33595=CARTESIAN_POINT('Ctrl Pts',(-2.84968053289451,-1.,-2.99832751144925));
#33596=CARTESIAN_POINT('Ctrl Pts',(-2.84246132984415,-1.,-2.99542425341685));
#33597=CARTESIAN_POINT('Ctrl Pts',(-2.83526351254248,-1.,-2.99249155170339));
#33598=CARTESIAN_POINT('Ctrl Pts',(-2.82808728190157,-1.,-2.98952916401446));
#33599=CARTESIAN_POINT('Ctrl Pts',(-2.82093279065457,-1.,-2.9865368066918));
#33600=CARTESIAN_POINT('Ctrl Pts',(-2.81380019196286,-1.,-2.98351419779767));
#33601=CARTESIAN_POINT('Ctrl Pts',(-2.80668968101106,-1.,-2.98046109647241));
#33602=CARTESIAN_POINT('Ctrl Pts',(-2.7996015327823,-1.,-2.97737733718287));
#33603=CARTESIAN_POINT('Ctrl Pts',(-2.79253615718248,-1.,-2.9742628834758));
#33604=CARTESIAN_POINT('Ctrl Pts',(-2.78549409123769,-1.,-2.97111781461465));
#33605=CARTESIAN_POINT('Ctrl Pts',(-2.7784758954285,-1.,-2.96794221043036));
#33606=CARTESIAN_POINT('Ctrl Pts',(-2.77148206836498,-1.,-2.96473605585583));
#33607=CARTESIAN_POINT('Ctrl Pts',(-2.76451296269557,-1.,-2.96149914764818));
#33608=CARTESIAN_POINT('Ctrl Pts',(-2.7575686788835,-1.,-2.95823097665896));
#33609=CARTESIAN_POINT('Ctrl Pts',(-2.75064903318947,-1.,-2.95493069316161));
#33610=CARTESIAN_POINT('Ctrl Pts',(-2.74375379492172,-1.,-2.95159737214266));
#33611=CARTESIAN_POINT('Ctrl Pts',(-2.73688288329808,-1.,-2.94823023414364));
#33612=CARTESIAN_POINT('Ctrl Pts',(-2.73003657371617,-1.,-2.94482887675143));
#33613=CARTESIAN_POINT('Ctrl Pts',(-2.72321571511337,-1.,-2.94139351933897));
#33614=CARTESIAN_POINT('Ctrl Pts',(-2.71642190053592,-1.,-2.93792519474972));
#33615=CARTESIAN_POINT('Ctrl Pts',(-2.70965695523787,-1.,-2.93442516311179));
#33616=CARTESIAN_POINT('Ctrl Pts',(-2.70292247416885,-1.,-2.93089438233749));
#33617=CARTESIAN_POINT('Ctrl Pts',(-2.69621932864301,-1.,-2.92733294395267));
#33618=CARTESIAN_POINT('Ctrl Pts',(-2.68954721165339,-1.,-2.92373955325875));
#33619=CARTESIAN_POINT('Ctrl Pts',(-2.68290409279688,-1.,-2.92011090722152));
#33620=CARTESIAN_POINT('Ctrl Pts',(-2.67628728855312,-1.,-2.91644290704285));
#33621=CARTESIAN_POINT('Ctrl Pts',(-2.66969458792631,-1.,-2.91273193382882));
#33622=CARTESIAN_POINT('Ctrl Pts',(-2.6631254261681,-1.,-2.90897617968923));
#33623=CARTESIAN_POINT('Ctrl Pts',(-2.65658188464282,-1.,-2.90517678087461));
#33624=CARTESIAN_POINT('Ctrl Pts',(-2.65007017365564,-1.,-2.90133950224867));
#33625=CARTESIAN_POINT('Ctrl Pts',(-2.64359851684131,-1.,-2.89747231723345));
#33626=CARTESIAN_POINT('Ctrl Pts',(-2.63717442263932,-1.,-2.89358228854544));
#33627=CARTESIAN_POINT('Ctrl Pts',(-2.63080195420767,-1.,-2.88967244854239));
#33628=CARTESIAN_POINT('Ctrl Pts',(-2.62447947640262,-1.,-2.88573922195059));
#33629=CARTESIAN_POINT('Ctrl Pts',(-2.61819596473108,-1.,-2.88176821427525));
#33630=CARTESIAN_POINT('Ctrl Pts',(-2.61193507170955,-1.,-2.87773881947915));
#33631=CARTESIAN_POINT('Ctrl Pts',(-2.60568177881303,-1.,-2.87363176656501));
#33632=CARTESIAN_POINT('Ctrl Pts',(-2.5994287522321,-1.,-2.86943633170722));
#33633=CARTESIAN_POINT('Ctrl Pts',(-2.59318160184908,-1.,-2.86515629953513));
#33634=CARTESIAN_POINT('Ctrl Pts',(-2.58696770643524,-1.,-2.86081999003629));
#33635=CARTESIAN_POINT('Ctrl Pts',(-2.58082875254357,-1.,-2.85647171715092));
#33636=CARTESIAN_POINT('Ctrl Pts',(-2.57480482727081,-1.,-2.85215360144431));
#33637=CARTESIAN_POINT('Ctrl Pts',(-2.56891984251721,-1.,-2.84788893329067));
#33638=CARTESIAN_POINT('Ctrl Pts',(-2.56316920798513,-1.,-2.84366802680237));
#33639=CARTESIAN_POINT('Ctrl Pts',(-2.55749952145241,-1.,-2.83942515220782));
#33640=CARTESIAN_POINT('Ctrl Pts',(-2.55182152807077,-1.,-2.83505269592536));
#33641=CARTESIAN_POINT('Ctrl Pts',(-2.54604736792655,-1.,-2.83044254225917));
#33642=CARTESIAN_POINT('Ctrl Pts',(-2.54012272520199,-1.,-2.8255216764922));
#33643=CARTESIAN_POINT('Ctrl Pts',(-2.53405679667412,-1.,-2.82028550483689));
#33644=CARTESIAN_POINT('Ctrl Pts',(-2.52796388055278,-1.,-2.81484379048475));
#33645=CARTESIAN_POINT('Ctrl Pts',(-2.52205778589653,-1.,-2.80941521966941));
#33646=CARTESIAN_POINT('Ctrl Pts',(-2.51660190465805,-1.,-2.80427363984653));
#33647=CARTESIAN_POINT('Ctrl Pts',(-2.51186983687818,-1.,-2.79970585014168));
#33648=CARTESIAN_POINT('Ctrl Pts',(-2.50810555977671,-1.,-2.79596878057287));
#33649=CARTESIAN_POINT('Ctrl Pts',(-2.50567182569081,-1.,-2.79344192164147));
#33650=CARTESIAN_POINT('Ctrl Pts',(-2.50455968395146,-1.,-2.79217568804755));
#33651=CARTESIAN_POINT('Ctrl Pts',(-2.50417932839313,-1.,-2.79164172518905));
#33652=CARTESIAN_POINT('Ctrl Pts',(-2.50410700351493,-1.,-2.79145823440781));
#33653=CARTESIAN_POINT('Ctrl Pts',(-2.50410331873176,-1.,-2.79140942341258));
#33654=CARTESIAN_POINT('',(-2.36531447826213,-1.,-2.90994629141562));
#33655=CARTESIAN_POINT('Origin',(0.,-1.,0.));
#33656=CARTESIAN_POINT('',(-2.52982887637028,-1.,-3.35260583073571));
#33657=CARTESIAN_POINT('Ctrl Pts',(-2.36531447826213,-1.,-2.90994629141562));
#33658=CARTESIAN_POINT('Ctrl Pts',(-2.3653621118858,-1.,-2.90995756655558));
#33659=CARTESIAN_POINT('Ctrl Pts',(-2.36553202948741,-1.,-2.9100577052777));
#33660=CARTESIAN_POINT('Ctrl Pts',(-2.36599991765853,-1.,-2.91051690822262));
#33661=CARTESIAN_POINT('Ctrl Pts',(-2.36707658451709,-1.,-2.91181344022628));
#33662=CARTESIAN_POINT('Ctrl Pts',(-2.36919161373074,-1.,-2.91461249883016));
#33663=CARTESIAN_POINT('Ctrl Pts',(-2.37229381109939,-1.,-2.9189150379156));
#33664=CARTESIAN_POINT('Ctrl Pts',(-2.37606510524271,-1.,-2.92430340582912));
#33665=CARTESIAN_POINT('Ctrl Pts',(-2.3802898958232,-1.,-2.93049643640517));
#33666=CARTESIAN_POINT('Ctrl Pts',(-2.38472771516476,-1.,-2.93717903280599));
#33667=CARTESIAN_POINT('Ctrl Pts',(-2.38914929090806,-1.,-2.94404820669135));
#33668=CARTESIAN_POINT('Ctrl Pts',(-2.39337207631613,-1.,-2.95085857128372));
#33669=CARTESIAN_POINT('Ctrl Pts',(-2.39730553974412,-1.,-2.95748006482811));
#33670=CARTESIAN_POINT('Ctrl Pts',(-2.40095565711535,-1.,-2.96390432240181));
#33671=CARTESIAN_POINT('Ctrl Pts',(-2.40438604734848,-1.,-2.97019641312272));
#33672=CARTESIAN_POINT('Ctrl Pts',(-2.40768975073691,-1.,-2.97646002822395));
#33673=CARTESIAN_POINT('Ctrl Pts',(-2.41095909342591,-1.,-2.98280015815132));
#33674=CARTESIAN_POINT('Ctrl Pts',(-2.4142506419963,-1.,-2.98927983005851));
#33675=CARTESIAN_POINT('Ctrl Pts',(-2.4175732450056,-1.,-2.99590509293561));
#33676=CARTESIAN_POINT('Ctrl Pts',(-2.42090763946812,-1.,-3.00264868586038));
#33677=CARTESIAN_POINT('Ctrl Pts',(-2.42421849439625,-1.,-3.00946442616674));
#33678=CARTESIAN_POINT('Ctrl Pts',(-2.4274685626416,-1.,-3.01630420830494));
#33679=CARTESIAN_POINT('Ctrl Pts',(-2.43063415586615,-1.,-3.02313656035977));
#33680=CARTESIAN_POINT('Ctrl Pts',(-2.43371241361462,-1.,-3.02995534946946));
#33681=CARTESIAN_POINT('Ctrl Pts',(-2.43671278042394,-1.,-3.03676949672797));
#33682=CARTESIAN_POINT('Ctrl Pts',(-2.43965194061849,-1.,-3.04359685040545));
#33683=CARTESIAN_POINT('Ctrl Pts',(-2.44254768923109,-1.,-3.05045678021509));
#33684=CARTESIAN_POINT('Ctrl Pts',(-2.44541251892568,-1.,-3.05736242671521));
#33685=CARTESIAN_POINT('Ctrl Pts',(-2.44824970516558,-1.,-3.06431596421422));
#33686=CARTESIAN_POINT('Ctrl Pts',(-2.45105688854432,-1.,-3.0713129052131));
#33687=CARTESIAN_POINT('Ctrl Pts',(-2.45382826787795,-1.,-3.07834472886145));
#33688=CARTESIAN_POINT('Ctrl Pts',(-2.45655725437037,-1.,-3.08540206545313));
#33689=CARTESIAN_POINT('Ctrl Pts',(-2.45923912563875,-1.,-3.09247787931881));
#33690=CARTESIAN_POINT('Ctrl Pts',(-2.4618730850188,-1.,-3.09956993697048));
#33691=CARTESIAN_POINT('Ctrl Pts',(-2.46446082979645,-1.,-3.10667907901981));
#33692=CARTESIAN_POINT('Ctrl Pts',(-2.46700558843507,-1.,-3.11380805536124));
#33693=CARTESIAN_POINT('Ctrl Pts',(-2.4695109894747,-1.,-3.12096015766984));
#33694=CARTESIAN_POINT('Ctrl Pts',(-2.47197997765868,-1.,-3.12813790805948));
#33695=CARTESIAN_POINT('Ctrl Pts',(-2.47441378371923,-1.,-3.13534181229282));
#33696=CARTESIAN_POINT('Ctrl Pts',(-2.47681245356095,-1.,-3.14257099546531));
#33697=CARTESIAN_POINT('Ctrl Pts',(-2.47917529057016,-1.,-3.14982373241335));
#33698=CARTESIAN_POINT('Ctrl Pts',(-2.48150133566568,-1.,-3.15709802322735));
#33699=CARTESIAN_POINT('Ctrl Pts',(-2.48378981792739,-1.,-3.16439213290181));
#33700=CARTESIAN_POINT('Ctrl Pts',(-2.48604065348619,-1.,-3.17170518863357));
#33701=CARTESIAN_POINT('Ctrl Pts',(-2.48825428288243,-1.,-3.17903698136679));
#33702=CARTESIAN_POINT('Ctrl Pts',(-2.49043146334095,-1.,-3.18638771282315));
#33703=CARTESIAN_POINT('Ctrl Pts',(-2.4925730723986,-1.,-3.19375775555814));
#33704=CARTESIAN_POINT('Ctrl Pts',(-2.49467992057726,-1.,-3.20114742397549));
#33705=CARTESIAN_POINT('Ctrl Pts',(-2.49675252647298,-1.,-3.2085566984974));
#33706=CARTESIAN_POINT('Ctrl Pts',(-2.49879114599293,-1.,-3.21598526261157));
#33707=CARTESIAN_POINT('Ctrl Pts',(-2.5007958720187,-1.,-3.22343262620387));
#33708=CARTESIAN_POINT('Ctrl Pts',(-2.50276671338074,-1.,-3.23089822320596));
#33709=CARTESIAN_POINT('Ctrl Pts',(-2.50470367580078,-1.,-3.23838151080383));
#33710=CARTESIAN_POINT('Ctrl Pts',(-2.50660685940645,-1.,-3.24588208984042));
#33711=CARTESIAN_POINT('Ctrl Pts',(-2.50847647070936,-1.,-3.25339971461265));
#33712=CARTESIAN_POINT('Ctrl Pts',(-2.51031277813697,-1.,-3.26093423001716));
#33713=CARTESIAN_POINT('Ctrl Pts',(-2.51211608411539,-1.,-3.26848552888271));
#33714=CARTESIAN_POINT('Ctrl Pts',(-2.51388669270329,-1.,-3.27605350473048));
#33715=CARTESIAN_POINT('Ctrl Pts',(-2.51562487464215,-1.,-3.28363799702583));
#33716=CARTESIAN_POINT('Ctrl Pts',(-2.51733085123316,-1.,-3.2912387729863));
#33717=CARTESIAN_POINT('Ctrl Pts',(-2.51900480700548,-1.,-3.29885556387661));
#33718=CARTESIAN_POINT('Ctrl Pts',(-2.52064689568167,-1.,-3.30648808814986));
#33719=CARTESIAN_POINT('Ctrl Pts',(-2.52225724871375,-1.,-3.31413607874727));
#33720=CARTESIAN_POINT('Ctrl Pts',(-2.52383598396878,-1.,-3.32179931079521));
#33721=CARTESIAN_POINT('Ctrl Pts',(-2.52538321165774,-1.,-3.32947762189049));
#33722=CARTESIAN_POINT('Ctrl Pts',(-2.52689902691551,-1.,-3.33717090000955));
#33723=CARTESIAN_POINT('Ctrl Pts',(-2.52808660916879,-1.,-3.34333744117093));
#33724=CARTESIAN_POINT('Ctrl Pts',(-2.5289632161143,-1.,-3.34796903577628));
#33725=CARTESIAN_POINT('Ctrl Pts',(-2.52954136549357,-1.,-3.35105973714426));
#33726=CARTESIAN_POINT('Ctrl Pts',(-2.52982887637028,-1.,-3.35260583073571));
#33727=CARTESIAN_POINT('',(-2.40675750623143,-1.,-3.44202241512147));
#33728=CARTESIAN_POINT('',(-2.52982887637028,-1.,-3.35260583073571));
#33729=CARTESIAN_POINT('',(-2.03660101169715,-1.,-3.14877060440327));
#33730=CARTESIAN_POINT('Ctrl Pts',(-2.40675750623143,-1.,-3.44202241512147));
#33731=CARTESIAN_POINT('Ctrl Pts',(-2.4053759295909,-1.,-3.44127120683039));
#33732=CARTESIAN_POINT('Ctrl Pts',(-2.40261515589405,-1.,-3.43976627484234));
#33733=CARTESIAN_POINT('Ctrl Pts',(-2.39848113410292,-1.,-3.43750133064416));
#33734=CARTESIAN_POINT('Ctrl Pts',(-2.39298338804493,-1.,-3.4344663067854));
#33735=CARTESIAN_POINT('Ctrl Pts',(-2.38613505843552,-1.,-3.4306473271292));
#33736=CARTESIAN_POINT('Ctrl Pts',(-2.37931067028926,-1.,-3.42680309754399));
#33737=CARTESIAN_POINT('Ctrl Pts',(-2.37251035954292,-1.,-3.42293356216511));
#33738=CARTESIAN_POINT('Ctrl Pts',(-2.36573431470642,-1.,-3.41903866635852));
#33739=CARTESIAN_POINT('Ctrl Pts',(-2.35898278606946,-1.,-3.41511836751469));
#33740=CARTESIAN_POINT('Ctrl Pts',(-2.35225606824109,-1.,-3.41117262314119));
#33741=CARTESIAN_POINT('Ctrl Pts',(-2.34555447649188,-1.,-3.40720137404297));
#33742=CARTESIAN_POINT('Ctrl Pts',(-2.33887832342782,-1.,-3.40320452776743));
#33743=CARTESIAN_POINT('Ctrl Pts',(-2.33222789882489,-1.,-3.39918194577956));
#33744=CARTESIAN_POINT('Ctrl Pts',(-2.3256034390248,-1.,-3.39513342019756));
#33745=CARTESIAN_POINT('Ctrl Pts',(-2.31900513925424,-1.,-3.39105869474822));
#33746=CARTESIAN_POINT('Ctrl Pts',(-2.31243319489367,-1.,-3.38695751492462));
#33747=CARTESIAN_POINT('Ctrl Pts',(-2.30588783640343,-1.,-3.3828296733661));
#33748=CARTESIAN_POINT('Ctrl Pts',(-2.29936936127624,-1.,-3.37867504959433));
#33749=CARTESIAN_POINT('Ctrl Pts',(-2.29287818007393,-1.,-3.37449367172826));
#33750=CARTESIAN_POINT('Ctrl Pts',(-2.28641481081137,-1.,-3.37028570206488));
#33751=CARTESIAN_POINT('Ctrl Pts',(-2.27997979458037,-1.,-3.36605130713076));
#33752=CARTESIAN_POINT('Ctrl Pts',(-2.2735736262093,-1.,-3.36179055004409));
#33753=CARTESIAN_POINT('Ctrl Pts',(-2.2671966857991,-1.,-3.35750328523061));
#33754=CARTESIAN_POINT('Ctrl Pts',(-2.26084915222449,-1.,-3.35318902552626));
#33755=CARTESIAN_POINT('Ctrl Pts',(-2.25453097693483,-1.,-3.34884690292285));
#33756=CARTESIAN_POINT('Ctrl Pts',(-2.24824207678256,-1.,-3.34447596770723));
#33757=CARTESIAN_POINT('Ctrl Pts',(-2.24198249391422,-1.,-3.34007543738025));
#33758=CARTESIAN_POINT('Ctrl Pts',(-2.23575256328812,-1.,-3.33564495756482));
#33759=CARTESIAN_POINT('Ctrl Pts',(-2.22955308907233,-1.,-3.33118487773611));
#33760=CARTESIAN_POINT('Ctrl Pts',(-2.22338548312772,-1.,-3.3266964672289));
#33761=CARTESIAN_POINT('Ctrl Pts',(-2.21725135110898,-1.,-3.32218125618968));
#33762=CARTESIAN_POINT('Ctrl Pts',(-2.21115211847875,-1.,-3.31764044024235));
#33763=CARTESIAN_POINT('Ctrl Pts',(-2.20508863150607,-1.,-3.31307424608949));
#33764=CARTESIAN_POINT('Ctrl Pts',(-2.19906078949923,-1.,-3.30848134694595));
#33765=CARTESIAN_POINT('Ctrl Pts',(-2.19306710376111,-1.,-3.30385816281831));
#33766=CARTESIAN_POINT('Ctrl Pts',(-2.18710556500327,-1.,-3.29920022557639));
#33767=CARTESIAN_POINT('Ctrl Pts',(-2.18117455557065,-1.,-3.2945036150049));
#33768=CARTESIAN_POINT('Ctrl Pts',(-2.17527380048423,-1.,-3.28976645712568));
#33769=CARTESIAN_POINT('Ctrl Pts',(-2.16940517773455,-1.,-3.28499019979724));
#33770=CARTESIAN_POINT('Ctrl Pts',(-2.16357391934425,-1.,-3.280181508414));
#33771=CARTESIAN_POINT('Ctrl Pts',(-2.15778690038347,-1.,-3.27534954469187));
#33772=CARTESIAN_POINT('Ctrl Pts',(-2.15205043199808,-1.,-3.27050245897228));
#33773=CARTESIAN_POINT('Ctrl Pts',(-2.1463680529566,-1.,-3.26564388189759));
#33774=CARTESIAN_POINT('Ctrl Pts',(-2.14073870754264,-1.,-3.26077002641879));
#33775=CARTESIAN_POINT('Ctrl Pts',(-2.13515375878803,-1.,-3.25586495065054));
#33776=CARTESIAN_POINT('Ctrl Pts',(-2.12960028396832,-1.,-3.25090574494028));
#33777=CARTESIAN_POINT('Ctrl Pts',(-2.12406646410962,-1.,-3.24587102613376));
#33778=CARTESIAN_POINT('Ctrl Pts',(-2.11854673326979,-1.,-3.24074905517293));
#33779=CARTESIAN_POINT('Ctrl Pts',(-2.11304604021773,-1.,-3.23554444767099));
#33780=CARTESIAN_POINT('Ctrl Pts',(-2.10758699642451,-1.,-3.23028945793289));
#33781=CARTESIAN_POINT('Ctrl Pts',(-2.10220384298492,-1.,-3.22503437553434));
#33782=CARTESIAN_POINT('Ctrl Pts',(-2.09692958434895,-1.,-3.21982707347009));
#33783=CARTESIAN_POINT('Ctrl Pts',(-2.09178419460443,-1.,-3.21469429601654));
#33784=CARTESIAN_POINT('Ctrl Pts',(-2.08676465517455,-1.,-3.20962575845463));
#33785=CARTESIAN_POINT('Ctrl Pts',(-2.08182850370878,-1.,-3.2045481863073));
#33786=CARTESIAN_POINT('Ctrl Pts',(-2.07690441870722,-1.,-3.19934132836019));
#33787=CARTESIAN_POINT('Ctrl Pts',(-2.07192253497857,-1.,-3.19388465568252));
#33788=CARTESIAN_POINT('Ctrl Pts',(-2.06684062744112,-1.,-3.18809755562368));
#33789=CARTESIAN_POINT('Ctrl Pts',(-2.06166849827101,-1.,-3.18197692964614));
#33790=CARTESIAN_POINT('Ctrl Pts',(-2.05650186773132,-1.,-3.17564906975371));
#33791=CARTESIAN_POINT('Ctrl Pts',(-2.05151770247233,-1.,-3.16936341689527));
#33792=CARTESIAN_POINT('Ctrl Pts',(-2.04693331247446,-1.,-3.16343165058912));
#33793=CARTESIAN_POINT('Ctrl Pts',(-2.04297406404027,-1.,-3.15817983946367));
#33794=CARTESIAN_POINT('Ctrl Pts',(-2.03984073791519,-1.,-3.15389991674792));
#33795=CARTESIAN_POINT('Ctrl Pts',(-2.03783225495961,-1.,-3.15102344775328));
#33796=CARTESIAN_POINT('Ctrl Pts',(-2.03693188810544,-1.,-3.14959882629805));
#33797=CARTESIAN_POINT('Ctrl Pts',(-2.03663974554932,-1.,-3.1490119366901));
#33798=CARTESIAN_POINT('Ctrl Pts',(-2.03659701539259,-1.,-3.14881939088124));
#33799=CARTESIAN_POINT('Ctrl Pts',(-2.03660101169715,-1.,-3.14877060440328));
#33800=CARTESIAN_POINT('',(-1.88097764062697,-1.,-3.24413672884812));
#33801=CARTESIAN_POINT('Origin',(0.,-1.,0.));
#33802=CARTESIAN_POINT('',(-1.97421938526992,-1.,-3.70708211654725));
#33803=CARTESIAN_POINT('Ctrl Pts',(-1.88097764062697,-1.,-3.24413672884812));
#33804=CARTESIAN_POINT('Ctrl Pts',(-1.8810229239812,-1.,-3.24415531671284));
#33805=CARTESIAN_POINT('Ctrl Pts',(-1.88117508446775,-1.,-3.24428080353022));
#33806=CARTESIAN_POINT('Ctrl Pts',(-1.88156537699203,-1.,-3.24480754676064));
#33807=CARTESIAN_POINT('Ctrl Pts',(-1.88242596600454,-1.,-3.2462565441079));
#33808=CARTESIAN_POINT('Ctrl Pts',(-1.88407708646357,-1.,-3.24935200511918));
#33809=CARTESIAN_POINT('Ctrl Pts',(-1.88646802523466,-1.,-3.25408686339463));
#33810=CARTESIAN_POINT('Ctrl Pts',(-1.88934996203698,-1.,-3.25999885193947));
#33811=CARTESIAN_POINT('Ctrl Pts',(-1.89255393500965,-1.,-3.26677653888676));
#33812=CARTESIAN_POINT('Ctrl Pts',(-1.89589172903793,-1.,-3.27407108933139));
#33813=CARTESIAN_POINT('Ctrl Pts',(-1.89918429230462,-1.,-3.28154737912352));
#33814=CARTESIAN_POINT('Ctrl Pts',(-1.90228971247527,-1.,-3.2889344860029));
#33815=CARTESIAN_POINT('Ctrl Pts',(-1.90513891864087,-1.,-3.29608978722113));
#33816=CARTESIAN_POINT('Ctrl Pts',(-1.90773912171341,-1.,-3.30300595568195));
#33817=CARTESIAN_POINT('Ctrl Pts',(-1.91014297830446,-1.,-3.30975721158596));
#33818=CARTESIAN_POINT('Ctrl Pts',(-1.91242616234442,-1.,-3.31646052426364));
#33819=CARTESIAN_POINT('Ctrl Pts',(-1.91466343916628,-1.,-3.32323403454535));
#33820=CARTESIAN_POINT('Ctrl Pts',(-1.91690081930331,-1.,-3.33014884257873));
#33821=CARTESIAN_POINT('Ctrl Pts',(-1.9191460961021,-1.,-3.33721230710012));
#33822=CARTESIAN_POINT('Ctrl Pts',(-1.92138450828404,-1.,-3.34439448941961));
#33823=CARTESIAN_POINT('Ctrl Pts',(-1.92358838440528,-1.,-3.35164424847223));
#33824=CARTESIAN_POINT('Ctrl Pts',(-1.92572846125756,-1.,-3.35890824422965));
#33825=CARTESIAN_POINT('Ctrl Pts',(-1.92778626543786,-1.,-3.36615168657567));
#33826=CARTESIAN_POINT('Ctrl Pts',(-1.92975993109877,-1.,-3.37336807068043));
#33827=CARTESIAN_POINT('Ctrl Pts',(-1.93165739093276,-1.,-3.3805676852555));
#33828=CARTESIAN_POINT('Ctrl Pts',(-1.93349233176788,-1.,-3.38777076883256));
#33829=CARTESIAN_POINT('Ctrl Pts',(-1.93527929945985,-1.,-3.39499923640795));
#33830=CARTESIAN_POINT('Ctrl Pts',(-1.93702857723098,-1.,-3.40226802104109));
#33831=CARTESIAN_POINT('Ctrl Pts',(-1.93874306008143,-1.,-3.40957978266642));
#33832=CARTESIAN_POINT('Ctrl Pts',(-1.94042111965246,-1.,-3.41692971994096));
#33833=CARTESIAN_POINT('Ctrl Pts',(-1.94205835913696,-1.,-3.42430850941503));
#33834=CARTESIAN_POINT('Ctrl Pts',(-1.94364973660284,-1.,-3.43170586602434));
#33835=CARTESIAN_POINT('Ctrl Pts',(-1.94519168842879,-1.,-3.43911410197687));
#33836=CARTESIAN_POINT('Ctrl Pts',(-1.94668377715329,-1.,-3.44653088665681));
#33837=CARTESIAN_POINT('Ctrl Pts',(-1.94812754766524,-1.,-3.45395731584051));
#33838=CARTESIAN_POINT('Ctrl Pts',(-1.94952575850197,-1.,-3.46139661060962));
#33839=CARTESIAN_POINT('Ctrl Pts',(-1.95088147859877,-1.,-3.46885258974191));
#33840=CARTESIAN_POINT('Ctrl Pts',(-1.95219722189876,-1.,-3.47632820495921));
#33841=CARTESIAN_POINT('Ctrl Pts',(-1.95347412486309,-1.,-3.48382414832634));
#33842=CARTESIAN_POINT('Ctrl Pts',(-1.95471236969643,-1.,-3.49133956289133));
#33843=CARTESIAN_POINT('Ctrl Pts',(-1.95591153823661,-1.,-3.49887263575583));
#33844=CARTESIAN_POINT('Ctrl Pts',(-1.95707099606511,-1.,-3.50642124159909));
#33845=CARTESIAN_POINT('Ctrl Pts',(-1.95819025316779,-1.,-3.51398354617794));
#33846=CARTESIAN_POINT('Ctrl Pts',(-1.95926936324461,-1.,-3.52155867431486));
#33847=CARTESIAN_POINT('Ctrl Pts',(-1.96030879411566,-1.,-3.52914648844351));
#33848=CARTESIAN_POINT('Ctrl Pts',(-1.96130926212689,-1.,-3.53674730625813));
#33849=CARTESIAN_POINT('Ctrl Pts',(-1.96227157573067,-1.,-3.54436163300443));
#33850=CARTESIAN_POINT('Ctrl Pts',(-1.96319648628644,-1.,-3.55198990600886));
#33851=CARTESIAN_POINT('Ctrl Pts',(-1.96408450906812,-1.,-3.55963218706096));
#33852=CARTESIAN_POINT('Ctrl Pts',(-1.96493594634567,-1.,-3.56728820357791));
#33853=CARTESIAN_POINT('Ctrl Pts',(-1.96575096652789,-1.,-3.57495748600959));
#33854=CARTESIAN_POINT('Ctrl Pts',(-1.96652966688911,-1.,-3.58263947663829));
#33855=CARTESIAN_POINT('Ctrl Pts',(-1.96727213799544,-1.,-3.59033364022801));
#33856=CARTESIAN_POINT('Ctrl Pts',(-1.96797854118369,-1.,-3.59803959819938));
#33857=CARTESIAN_POINT('Ctrl Pts',(-1.9686491188594,-1.,-3.60575714017989));
#33858=CARTESIAN_POINT('Ctrl Pts',(-1.96928416040877,-1.,-3.61348615496704));
#33859=CARTESIAN_POINT('Ctrl Pts',(-1.96988398129978,-1.,-3.62122658401893));
#33860=CARTESIAN_POINT('Ctrl Pts',(-1.97044889850463,-1.,-3.62897836973293));
#33861=CARTESIAN_POINT('Ctrl Pts',(-1.97097920454464,-1.,-3.63674139590412));
#33862=CARTESIAN_POINT('Ctrl Pts',(-1.97147515441164,-1.,-3.64451546723514));
#33863=CARTESIAN_POINT('Ctrl Pts',(-1.9719369724024,-1.,-3.652300347166));
#33864=CARTESIAN_POINT('Ctrl Pts',(-1.9723648543905,-1.,-3.6600957816636));
#33865=CARTESIAN_POINT('Ctrl Pts',(-1.97275897198678,-1.,-3.66790152752075));
#33866=CARTESIAN_POINT('Ctrl Pts',(-1.97311947678517,-1.,-3.67571738107084));
#33867=CARTESIAN_POINT('Ctrl Pts',(-1.97344650304519,-1.,-3.68354319915092));
#33868=CARTESIAN_POINT('Ctrl Pts',(-1.97374016225483,-1.,-3.69137888599902));
#33869=CARTESIAN_POINT('Ctrl Pts',(-1.97394846383216,-1.,-3.6976552856004));
#33870=CARTESIAN_POINT('Ctrl Pts',(-1.97408973726715,-1.,-3.70236698912904));
#33871=CARTESIAN_POINT('Ctrl Pts',(-1.97417727645308,-1.,-3.70551008132332));
#33872=CARTESIAN_POINT('Ctrl Pts',(-1.97421938526992,-1.,-3.70708211654725));
#33873=CARTESIAN_POINT('',(-1.83867539237861,-1.,-3.77614523045147));
#33874=CARTESIAN_POINT('',(-1.97421938526992,-1.,-3.70708211654725));
#33875=CARTESIAN_POINT('',(-1.5189508286633,-1.,-3.42859860294306));
#33876=CARTESIAN_POINT('Ctrl Pts',(-1.83867539237861,-1.,-3.77614523045147));
#33877=CARTESIAN_POINT('Ctrl Pts',(-1.83742834010626,-1.,-3.77518714457833));
#33878=CARTESIAN_POINT('Ctrl Pts',(-1.83493697934534,-1.,-3.77326886064398));
#33879=CARTESIAN_POINT('Ctrl Pts',(-1.83120816955645,-1.,-3.77038509817999));
#33880=CARTESIAN_POINT('Ctrl Pts',(-1.82625289220915,-1.,-3.76652740353775));
#33881=CARTESIAN_POINT('Ctrl Pts',(-1.82008629694091,-1.,-3.76168412707948));
#33882=CARTESIAN_POINT('Ctrl Pts',(-1.8139472983358,-1.,-3.75681965683071));
#33883=CARTESIAN_POINT('Ctrl Pts',(-1.80783603939617,-1.,-3.75193395887977));
#33884=CARTESIAN_POINT('Ctrl Pts',(-1.8017527148577,-1.,-3.74702700875467));
#33885=CARTESIAN_POINT('Ctrl Pts',(-1.79569757859422,-1.,-3.74209880352445));
#33886=CARTESIAN_POINT('Ctrl Pts',(-1.78967092823491,-1.,-3.73714934730681));
#33887=CARTESIAN_POINT('Ctrl Pts',(-1.78367308442901,-1.,-3.7321786309547));
#33888=CARTESIAN_POINT('Ctrl Pts',(-1.77770437039658,-1.,-3.72718661205609));
#33889=CARTESIAN_POINT('Ctrl Pts',(-1.77176509401761,-1.,-3.72217319911254));
#33890=CARTESIAN_POINT('Ctrl Pts',(-1.76585552124394,-1.,-3.71713822377359));
#33891=CARTESIAN_POINT('Ctrl Pts',(-1.75997588498865,-1.,-3.71208146346136));
#33892=CARTESIAN_POINT('Ctrl Pts',(-1.75412641804042,-1.,-3.70700269736659));
#33893=CARTESIAN_POINT('Ctrl Pts',(-1.74830738046057,-1.,-3.7019017567335));
#33894=CARTESIAN_POINT('Ctrl Pts',(-1.74251908492617,-1.,-3.69677856910517));
#33895=CARTESIAN_POINT('Ctrl Pts',(-1.73676193254557,-1.,-3.69163322648036));
#33896=CARTESIAN_POINT('Ctrl Pts',(-1.73103640956717,-1.,-3.68646597019332));
#33897=CARTESIAN_POINT('Ctrl Pts',(-1.72534302437056,-1.,-3.68127704936579));
#33898=CARTESIAN_POINT('Ctrl Pts',(-1.71968225581808,-1.,-3.67606660374709));
#33899=CARTESIAN_POINT('Ctrl Pts',(-1.71405450210384,-1.,-3.67083454901611));
#33900=CARTESIAN_POINT('Ctrl Pts',(-1.70846001610956,-1.,-3.66558043198876));
#33901=CARTESIAN_POINT('Ctrl Pts',(-1.70289888566873,-1.,-3.66030338774847));
#33902=CARTESIAN_POINT('Ctrl Pts',(-1.69737117722534,-1.,-3.65500246526749));
#33903=CARTESIAN_POINT('Ctrl Pts',(-1.69187705481689,-1.,-3.64967689827371));
#33904=CARTESIAN_POINT('Ctrl Pts',(-1.68641690471457,-1.,-3.64432638915203));
#33905=CARTESIAN_POINT('Ctrl Pts',(-1.68099146651586,-1.,-3.63895140887462));
#33906=CARTESIAN_POINT('Ctrl Pts',(-1.67560193613156,-1.,-3.63355343201232));
#33907=CARTESIAN_POINT('Ctrl Pts',(-1.67024966008045,-1.,-3.62813422105271));
#33908=CARTESIAN_POINT('Ctrl Pts',(-1.66493585923855,-1.,-3.62269517989109));
#33909=CARTESIAN_POINT('Ctrl Pts',(-1.65966133399186,-1.,-3.61723666482456));
#33910=CARTESIAN_POINT('Ctrl Pts',(-1.65442619244325,-1.,-3.61175734965127));
#33911=CARTESIAN_POINT('Ctrl Pts',(-1.64922952425832,-1.,-3.60625346556992));
#33912=CARTESIAN_POINT('Ctrl Pts',(-1.64407004385582,-1.,-3.60072028513845));
#33913=CARTESIAN_POINT('Ctrl Pts',(-1.63894676675352,-1.,-3.59515368334893));
#33914=CARTESIAN_POINT('Ctrl Pts',(-1.6338597145126,-1.,-3.58955176627879));
#33915=CARTESIAN_POINT('Ctrl Pts',(-1.62881051550745,-1.,-3.58391625774343));
#33916=CARTESIAN_POINT('Ctrl Pts',(-1.62380329464844,-1.,-3.5782545595439));
#33917=CARTESIAN_POINT('Ctrl Pts',(-1.61884340915404,-1.,-3.57257679609806));
#33918=CARTESIAN_POINT('Ctrl Pts',(-1.61393581747514,-1.,-3.56689200468387));
#33919=CARTESIAN_POINT('Ctrl Pts',(-1.60908344685457,-1.,-3.5612043248298));
#33920=CARTESIAN_POINT('Ctrl Pts',(-1.60428584699853,-1.,-3.55550985096129));
#33921=CARTESIAN_POINT('Ctrl Pts',(-1.59953698113457,-1.,-3.54979148634454));
#33922=CARTESIAN_POINT('Ctrl Pts',(-1.59482766949766,-1.,-3.54402458182337));
#33923=CARTESIAN_POINT('Ctrl Pts',(-1.59014958368739,-1.,-3.53818616861077));
#33924=CARTESIAN_POINT('Ctrl Pts',(-1.58549906268088,-1.,-3.5322637814708));
#33925=CARTESIAN_POINT('Ctrl Pts',(-1.58088027227848,-1.,-3.52626275334881));
#33926=CARTESIAN_POINT('Ctrl Pts',(-1.57631049988158,-1.,-3.52021847865912));
#33927=CARTESIAN_POINT('Ctrl Pts',(-1.57181569799743,-1.,-3.51418598431665));
#33928=CARTESIAN_POINT('Ctrl Pts',(-1.56742097575012,-1.,-3.50821771695363));
#33929=CARTESIAN_POINT('Ctrl Pts',(-1.56314187758675,-1.,-3.50234321621578));
#33930=CARTESIAN_POINT('Ctrl Pts',(-1.55897703097874,-1.,-3.49655185179655));
#33931=CARTESIAN_POINT('Ctrl Pts',(-1.55489595901116,-1.,-3.4907646087742));
#33932=CARTESIAN_POINT('Ctrl Pts',(-1.55084702970452,-1.,-3.48485155928567));
#33933=CARTESIAN_POINT('Ctrl Pts',(-1.54678009290276,-1.,-3.47868272898751));
#33934=CARTESIAN_POINT('Ctrl Pts',(-1.54266605398187,-1.,-3.47217189224653));
#33935=CARTESIAN_POINT('Ctrl Pts',(-1.53851507915502,-1.,-3.46531752207153));
#33936=CARTESIAN_POINT('Ctrl Pts',(-1.53440195378792,-1.,-3.45825932955032));
#33937=CARTESIAN_POINT('Ctrl Pts',(-1.53046244461635,-1.,-3.45127136828305));
#33938=CARTESIAN_POINT('Ctrl Pts',(-1.52686242875556,-1.,-3.44469547526647));
#33939=CARTESIAN_POINT('Ctrl Pts',(-1.5237734895035,-1.,-3.4388889597401));
#33940=CARTESIAN_POINT('Ctrl Pts',(-1.52134826724293,-1.,-3.43417156977893));
#33941=CARTESIAN_POINT('Ctrl Pts',(-1.5198144909338,-1.,-3.43101631893414));
#33942=CARTESIAN_POINT('Ctrl Pts',(-1.51914806898491,-1.,-3.42946838852587));
#33943=CARTESIAN_POINT('Ctrl Pts',(-1.5189513329503,-1.,-3.42884302333841));
#33944=CARTESIAN_POINT('Ctrl Pts',(-1.51893924967331,-1.,-3.42864616361875));
#33945=CARTESIAN_POINT('Ctrl Pts',(-1.5189508286633,-1.,-3.42859860294306));
#33946=CARTESIAN_POINT('',(-1.35032489087269,-1.,-3.49844575334386));
#33947=CARTESIAN_POINT('Origin',(0.,-1.,0.));
#33948=CARTESIAN_POINT('',(-1.36999806084572,-1.,-3.97027773754922));
#33949=CARTESIAN_POINT('Ctrl Pts',(-1.35032489087269,-1.,-3.49844575334386));
#33950=CARTESIAN_POINT('Ctrl Pts',(-1.35036670893102,-1.,-3.49847119623841));
#33951=CARTESIAN_POINT('Ctrl Pts',(-1.35049736560633,-1.,-3.49861894124915));
#33952=CARTESIAN_POINT('Ctrl Pts',(-1.35080045218652,-1.,-3.49920025459856));
#33953=CARTESIAN_POINT('Ctrl Pts',(-1.35142377279535,-1.,-3.5007660381658));
#33954=CARTESIAN_POINT('Ctrl Pts',(-1.3525703284343,-1.,-3.50408168106113));
#33955=CARTESIAN_POINT('Ctrl Pts',(-1.35419113576022,-1.,-3.50913227060177));
#33956=CARTESIAN_POINT('Ctrl Pts',(-1.35611275237288,-1.,-3.51542230699919));
#33957=CARTESIAN_POINT('Ctrl Pts',(-1.35821701528975,-1.,-3.52261776117121));
#33958=CARTESIAN_POINT('Ctrl Pts',(-1.36037259643827,-1.,-3.53034464961849));
#33959=CARTESIAN_POINT('Ctrl Pts',(-1.36245507339334,-1.,-3.53824396425032));
#33960=CARTESIAN_POINT('Ctrl Pts',(-1.36436666257567,-1.,-3.54602591832893));
#33961=CARTESIAN_POINT('Ctrl Pts',(-1.36606145456711,-1.,-3.55353883995793));
#33962=CARTESIAN_POINT('Ctrl Pts',(-1.36754771771174,-1.,-3.56077662028492));
#33963=CARTESIAN_POINT('Ctrl Pts',(-1.36886584973349,-1.,-3.56782080304554));
#33964=CARTESIAN_POINT('Ctrl Pts',(-1.37007229485646,-1.,-3.57479875549453));
#33965=CARTESIAN_POINT('Ctrl Pts',(-1.37122241663073,-1.,-3.58183885982745));
#33966=CARTESIAN_POINT('Ctrl Pts',(-1.37235053661,-1.,-3.5890185384643));
#33967=CARTESIAN_POINT('Ctrl Pts',(-1.37346320103184,-1.,-3.59634627869117));
#33968=CARTESIAN_POINT('Ctrl Pts',(-1.37455051379642,-1.,-3.60379020124038));
#33969=CARTESIAN_POINT('Ctrl Pts',(-1.37559314436641,-1.,-3.61129546591082));
#33970=CARTESIAN_POINT('Ctrl Pts',(-1.37657053403102,-1.,-3.61880481160408));
#33971=CARTESIAN_POINT('Ctrl Pts',(-1.37746987919868,-1.,-3.62628098665112));
#33972=CARTESIAN_POINT('Ctrl Pts',(-1.37829035457324,-1.,-3.63371727442448));
#33973=CARTESIAN_POINT('Ctrl Pts',(-1.37903818567347,-1.,-3.64112507791112));
#33974=CARTESIAN_POINT('Ctrl Pts',(-1.37972372481598,-1.,-3.64852652756444));
#33975=CARTESIAN_POINT('Ctrl Pts',(-1.38035791051215,-1.,-3.65594554404396));
#33976=CARTESIAN_POINT('Ctrl Pts',(-1.38094856333558,-1.,-3.66339848520874));
#33977=CARTESIAN_POINT('Ctrl Pts',(-1.38149812653876,-1.,-3.67088843112282));
#33978=CARTESIAN_POINT('Ctrl Pts',(-1.38200574290626,-1.,-3.6784103848243));
#33979=CARTESIAN_POINT('Ctrl Pts',(-1.38246852827185,-1.,-3.68595444983844));
#33980=CARTESIAN_POINT('Ctrl Pts',(-1.38288311171649,-1.,-3.69350967899523));
#33981=CARTESIAN_POINT('Ctrl Pts',(-1.38324717612862,-1.,-3.70106792167894));
#33982=CARTESIAN_POINT('Ctrl Pts',(-1.38356065402122,-1.,-3.70862680753343));
#33983=CARTESIAN_POINT('Ctrl Pts',(-1.38382489984585,-1.,-3.7161876605181));
#33984=CARTESIAN_POINT('Ctrl Pts',(-1.3840421342895,-1.,-3.72375409358805));
#33985=CARTESIAN_POINT('Ctrl Pts',(-1.38421479111531,-1.,-3.73133035859283));
#33986=CARTESIAN_POINT('Ctrl Pts',(-1.38434489156456,-1.,-3.73891976418099));
#33987=CARTESIAN_POINT('Ctrl Pts',(-1.38443344984389,-1.,-3.7465231716786));
#33988=CARTESIAN_POINT('Ctrl Pts',(-1.38448077997155,-1.,-3.75413976318727));
#33989=CARTESIAN_POINT('Ctrl Pts',(-1.38448675253343,-1.,-3.76176768271347));
#33990=CARTESIAN_POINT('Ctrl Pts',(-1.38445107339517,-1.,-3.76940473185775));
#33991=CARTESIAN_POINT('Ctrl Pts',(-1.38437354551435,-1.,-3.77704902230441));
#33992=CARTESIAN_POINT('Ctrl Pts',(-1.38425435883773,-1.,-3.78469969805134));
#33993=CARTESIAN_POINT('Ctrl Pts',(-1.38409399694589,-1.,-3.79235669640907));
#33994=CARTESIAN_POINT('Ctrl Pts',(-1.38389311766701,-1.,-3.80002044322169));
#33995=CARTESIAN_POINT('Ctrl Pts',(-1.38365244046226,-1.,-3.80769156398429));
#33996=CARTESIAN_POINT('Ctrl Pts',(-1.38337263902766,-1.,-3.81537060817765));
#33997=CARTESIAN_POINT('Ctrl Pts',(-1.38305421262724,-1.,-3.82305771743715));
#33998=CARTESIAN_POINT('Ctrl Pts',(-1.38269750245086,-1.,-3.83075266982138));
#33999=CARTESIAN_POINT('Ctrl Pts',(-1.38230274828774,-1.,-3.83845502790609));
#34000=CARTESIAN_POINT('Ctrl Pts',(-1.38187013346089,-1.,-3.84616425605705));
#34001=CARTESIAN_POINT('Ctrl Pts',(-1.38139983115075,-1.,-3.85387983979557));
#34002=CARTESIAN_POINT('Ctrl Pts',(-1.38089205993067,-1.,-3.86160143044187));
#34003=CARTESIAN_POINT('Ctrl Pts',(-1.38034709213129,-1.,-3.86932885813403));
#34004=CARTESIAN_POINT('Ctrl Pts',(-1.37976523097187,-1.,-3.87706205830865));
#34005=CARTESIAN_POINT('Ctrl Pts',(-1.37914679719446,-1.,-3.88480102249461));
#34006=CARTESIAN_POINT('Ctrl Pts',(-1.37849211287981,-1.,-3.89254574338385));
#34007=CARTESIAN_POINT('Ctrl Pts',(-1.3778014851263,-1.,-3.90029615196255));
#34008=CARTESIAN_POINT('Ctrl Pts',(-1.3770751963376,-1.,-3.90805209522729));
#34009=CARTESIAN_POINT('Ctrl Pts',(-1.37631350505516,-1.,-3.91581337461825));
#34010=CARTESIAN_POINT('Ctrl Pts',(-1.37551664448057,-1.,-3.92357976987132));
#34011=CARTESIAN_POINT('Ctrl Pts',(-1.37468482215784,-1.,-3.93135106761941));
#34012=CARTESIAN_POINT('Ctrl Pts',(-1.37381821967499,-1.,-3.93912709041791));
#34013=CARTESIAN_POINT('Ctrl Pts',(-1.37291699203423,-1.,-3.94690771786926));
#34014=CARTESIAN_POINT('Ctrl Pts',(-1.37198126433139,-1.,-3.95469287283105));
#34015=CARTESIAN_POINT('Ctrl Pts',(-1.37120515615663,-1.,-3.96092458508407));
#34016=CARTESIAN_POINT('Ctrl Pts',(-1.37060761746027,-1.,-3.96560037975788));
#34017=CARTESIAN_POINT('Ctrl Pts',(-1.37020239094758,-1.,-3.9687184694173));
#34018=CARTESIAN_POINT('Ctrl Pts',(-1.36999806084572,-1.,-3.97027773754922));
#34019=CARTESIAN_POINT('',(-1.22531898815164,-1.,-4.01728681790024));
#34020=CARTESIAN_POINT('',(-1.36999806084572,-1.,-3.97027773754922));
#34021=CARTESIAN_POINT('',(-0.963899035118986,-1.,-3.62400312501199));
#34022=CARTESIAN_POINT('Ctrl Pts',(-1.22531898815164,-1.,-4.01728681790024));
#34023=CARTESIAN_POINT('Ctrl Pts',(-1.22423716681317,-1.,-4.01614544569895));
#34024=CARTESIAN_POINT('Ctrl Pts',(-1.22207656455845,-1.,-4.01386104433519));
#34025=CARTESIAN_POINT('Ctrl Pts',(-1.21884478244403,-1.,-4.01042947140789));
#34026=CARTESIAN_POINT('Ctrl Pts',(-1.21455398918133,-1.,-4.00584409522722));
#34027=CARTESIAN_POINT('Ctrl Pts',(-1.20922097029551,-1.,-4.00009577950721));
#34028=CARTESIAN_POINT('Ctrl Pts',(-1.20391852375139,-1.,-3.99433084799666));
#34029=CARTESIAN_POINT('Ctrl Pts',(-1.19864679609566,-1.,-3.98854928957189));
#34030=CARTESIAN_POINT('Ctrl Pts',(-1.19340598349475,-1.,-3.98275111052561));
#34031=CARTESIAN_POINT('Ctrl Pts',(-1.18819633715539,-1.,-3.97693634767754));
#34032=CARTESIAN_POINT('Ctrl Pts',(-1.18301815039831,-1.,-3.97110505165415));
#34033=CARTESIAN_POINT('Ctrl Pts',(-1.17787174135592,-1.,-3.96525726358159));
#34034=CARTESIAN_POINT('Ctrl Pts',(-1.17275743590361,-1.,-3.95939299213276));
#34035=CARTESIAN_POINT('Ctrl Pts',(-1.16767555244438,-1.,-3.95351219509876));
#34036=CARTESIAN_POINT('Ctrl Pts',(-1.16262637999157,-1.,-3.94761474780583));
#34037=CARTESIAN_POINT('Ctrl Pts',(-1.15761018340956,-1.,-3.94170046685203));
#34038=CARTESIAN_POINT('Ctrl Pts',(-1.1526272271632,-1.,-3.9357691705628));
#34039=CARTESIAN_POINT('Ctrl Pts',(-1.14767779451123,-1.,-3.92982073294257));
#34040=CARTESIAN_POINT('Ctrl Pts',(-1.14276220561593,-1.,-3.92385513133997));
#34041=CARTESIAN_POINT('Ctrl Pts',(-1.13788084225554,-1.,-3.91787251936827));
#34042=CARTESIAN_POINT('Ctrl Pts',(-1.13303414693896,-1.,-3.91187321145649));
#34043=CARTESIAN_POINT('Ctrl Pts',(-1.12822258281553,-1.,-3.90585753318737));
#34044=CARTESIAN_POINT('Ctrl Pts',(-1.12344660099043,-1.,-3.89982569750025));
#34045=CARTESIAN_POINT('Ctrl Pts',(-1.11870660794603,-1.,-3.89377768340344));
#34046=CARTESIAN_POINT('Ctrl Pts',(-1.11400292434429,-1.,-3.88771308285171));
#34047=CARTESIAN_POINT('Ctrl Pts',(-1.10933577224008,-1.,-3.88163105531724));
#34048=CARTESIAN_POINT('Ctrl Pts',(-1.10470536603287,-1.,-3.87553067187514));
#34049=CARTESIAN_POINT('Ctrl Pts',(-1.10011198761195,-1.,-3.86941120134849));
#34050=CARTESIAN_POINT('Ctrl Pts',(-1.09555606505013,-1.,-3.86327241021247));
#34051=CARTESIAN_POINT('Ctrl Pts',(-1.09103825516294,-1.,-3.85711487933931));
#34052=CARTESIAN_POINT('Ctrl Pts',(-1.08655950846384,-1.,-3.85094025222713));
#34053=CARTESIAN_POINT('Ctrl Pts',(-1.08212087917991,-1.,-3.8447504803063));
#34054=CARTESIAN_POINT('Ctrl Pts',(-1.07772335353858,-1.,-3.83854714117491));
#34055=CARTESIAN_POINT('Ctrl Pts',(-1.07336766633459,-1.,-3.83233071195144));
#34056=CARTESIAN_POINT('Ctrl Pts',(-1.06905413180359,-1.,-3.82609989967276));
#34057=CARTESIAN_POINT('Ctrl Pts',(-1.0647824403893,-1.,-3.81985083953012));
#34058=CARTESIAN_POINT('Ctrl Pts',(-1.06055206187299,-1.,-3.8135786611749));
#34059=CARTESIAN_POINT('Ctrl Pts',(-1.05636266918644,-1.,-3.80727913637791));
#34060=CARTESIAN_POINT('Ctrl Pts',(-1.05221457990016,-1.,-3.80095039790681));
#34061=CARTESIAN_POINT('Ctrl Pts',(-1.04810913267639,-1.,-3.79459440308786));
#34062=CARTESIAN_POINT('Ctrl Pts',(-1.04404924374422,-1.,-3.78821910787179));
#34063=CARTESIAN_POINT('Ctrl Pts',(-1.04003862055798,-1.,-3.7818353500817));
#34064=CARTESIAN_POINT('Ctrl Pts',(-1.03608074678008,-1.,-3.77545283140427));
#34065=CARTESIAN_POINT('Ctrl Pts',(-1.03217786604919,-1.,-3.76907609832516));
#34066=CARTESIAN_POINT('Ctrl Pts',(-1.02833014458184,-1.,-3.76270122291245));
#34067=CARTESIAN_POINT('Ctrl Pts',(-1.02453429444668,-1.,-3.75631037456224));
#34068=CARTESIAN_POINT('Ctrl Pts',(-1.02078510487439,-1.,-3.74987777155873));
#34069=CARTESIAN_POINT('Ctrl Pts',(-1.01707794311088,-1.,-3.74337942504993));
#34070=CARTESIAN_POINT('Ctrl Pts',(-1.01341114319906,-1.,-3.73680245055747));
#34071=CARTESIAN_POINT('Ctrl Pts',(-1.00978798539491,-1.,-3.73015276704407));
#34072=CARTESIAN_POINT('Ctrl Pts',(-1.00622000735696,-1.,-3.72346803750544));
#34073=CARTESIAN_POINT('Ctrl Pts',(-1.00272423396802,-1.,-3.71680667125047));
#34074=CARTESIAN_POINT('Ctrl Pts',(-0.999317260756344,-1.,-3.7102243971387));
#34075=CARTESIAN_POINT('Ctrl Pts',(-0.996009819772432,-1.,-3.70375282282107));
#34076=CARTESIAN_POINT('Ctrl Pts',(-0.992802218332104,-1.,-3.69738123415696));
#34077=CARTESIAN_POINT('Ctrl Pts',(-0.989676715398858,-1.,-3.69102682138955));
#34078=CARTESIAN_POINT('Ctrl Pts',(-0.986602639864286,-1.,-3.6845531792623));
#34079=CARTESIAN_POINT('Ctrl Pts',(-0.983550791470864,-1.,-3.67782408841876));
#34080=CARTESIAN_POINT('Ctrl Pts',(-0.980505922458494,-1.,-3.67074983340444));
#34081=CARTESIAN_POINT('Ctrl Pts',(-0.977478312751416,-1.,-3.66333049637403));
#34082=CARTESIAN_POINT('Ctrl Pts',(-0.974519971354139,-1.,-3.6557157673487));
#34083=CARTESIAN_POINT('Ctrl Pts',(-0.971722122060277,-1.,-3.64819756447072));
#34084=CARTESIAN_POINT('Ctrl Pts',(-0.969195124674829,-1.,-3.64113946505393));
#34085=CARTESIAN_POINT('Ctrl Pts',(-0.967052554540877,-1.,-3.6349212208096));
#34086=CARTESIAN_POINT('Ctrl Pts',(-0.965395153165716,-1.,-3.62988252139998));
#34087=CARTESIAN_POINT('Ctrl Pts',(-0.964373850166081,-1.,-3.62652618145252));
#34088=CARTESIAN_POINT('Ctrl Pts',(-0.963957782642589,-1.,-3.62489305727516));
#34089=CARTESIAN_POINT('Ctrl Pts',(-0.963861297423579,-1.,-3.62424461507455));
#34090=CARTESIAN_POINT('Ctrl Pts',(-0.963880158556713,-1.,-3.62404828878374));
#34091=CARTESIAN_POINT('Ctrl Pts',(-0.963899035118986,-1.,-3.62400312501199));
#34092=CARTESIAN_POINT('',(-0.786422660833743,-1.,-3.66661143271648));
#34093=CARTESIAN_POINT('Origin',(0.,-1.,0.));
#34094=CARTESIAN_POINT('',(-0.732042837400619,-1.,-4.13571194405636));
#34095=CARTESIAN_POINT('Ctrl Pts',(-0.786422660833743,-1.,-3.66661143271648));
#34096=CARTESIAN_POINT('Ctrl Pts',(-0.786459983896781,-1.,-3.66664310415236));
#34097=CARTESIAN_POINT('Ctrl Pts',(-0.78656591955989,-1.,-3.66680946938396));
#34098=CARTESIAN_POINT('Ctrl Pts',(-0.786774337198499,-1.,-3.66743103898844));
#34099=CARTESIAN_POINT('Ctrl Pts',(-0.787145041181589,-1.,-3.66907505398769));
#34100=CARTESIAN_POINT('Ctrl Pts',(-0.787758799995426,-1.,-3.672529236635));
#34101=CARTESIAN_POINT('Ctrl Pts',(-0.788569566220662,-1.,-3.67777119516438));
#34102=CARTESIAN_POINT('Ctrl Pts',(-0.789483546065158,-1.,-3.68428439784285));
#34103=CARTESIAN_POINT('Ctrl Pts',(-0.79043628498958,-1.,-3.69172044327754));
#34104=CARTESIAN_POINT('Ctrl Pts',(-0.791356575696509,-1.,-3.69968940808982));
#34105=CARTESIAN_POINT('Ctrl Pts',(-0.792177688845968,-1.,-3.70781724021879));
#34106=CARTESIAN_POINT('Ctrl Pts',(-0.792848377370115,-1.,-3.7158024239604));
#34107=CARTESIAN_POINT('Ctrl Pts',(-0.79334702378387,-1.,-3.7234879729357));
#34108=CARTESIAN_POINT('Ctrl Pts',(-0.793682750269347,-1.,-3.7308691469564));
#34109=CARTESIAN_POINT('Ctrl Pts',(-0.79388270093679,-1.,-3.73803280541576));
#34110=CARTESIAN_POINT('Ctrl Pts',(-0.79398270045988,-1.,-3.74511357728827));
#34111=CARTESIAN_POINT('Ctrl Pts',(-0.794017347371441,-1.,-3.75224692493895));
#34112=CARTESIAN_POINT('Ctrl Pts',(-0.794008429135047,-1.,-3.75951468666325));
#34113=CARTESIAN_POINT('Ctrl Pts',(-0.793961083689141,-1.,-3.76692626931184));
#34114=CARTESIAN_POINT('Ctrl Pts',(-0.793870523787515,-1.,-3.77444863801264));
#34115=CARTESIAN_POINT('Ctrl Pts',(-0.793726235781339,-1.,-3.78202460377617));
#34116=CARTESIAN_POINT('Ctrl Pts',(-0.793516871680966,-1.,-3.78959439439222));
#34117=CARTESIAN_POINT('Ctrl Pts',(-0.7932356129732,-1.,-3.79711921389862));
#34118=CARTESIAN_POINT('Ctrl Pts',(-0.792882695234693,-1.,-3.80459229925598));
#34119=CARTESIAN_POINT('Ctrl Pts',(-0.792462483517568,-1.,-3.81202588694726));
#34120=CARTESIAN_POINT('Ctrl Pts',(-0.791981740718606,-1.,-3.81944345442237));
#34121=CARTESIAN_POINT('Ctrl Pts',(-0.791447528662381,-1.,-3.82687033899799));
#34122=CARTESIAN_POINT('Ctrl Pts',(-0.79086501270534,-1.,-3.83432392054804));
#34123=CARTESIAN_POINT('Ctrl Pts',(-0.790236124191289,-1.,-3.84180762342476));
#34124=CARTESIAN_POINT('Ctrl Pts',(-0.789560798155619,-1.,-3.8493163780891));
#34125=CARTESIAN_POINT('Ctrl Pts',(-0.788837734090688,-1.,-3.85683995872536));
#34126=CARTESIAN_POINT('Ctrl Pts',(-0.788065315093771,-1.,-3.86436702561342));
#34127=CARTESIAN_POINT('Ctrl Pts',(-0.78724252761798,-1.,-3.87188916600905));
#34128=CARTESIAN_POINT('Ctrl Pts',(-0.786369675812592,-1.,-3.87940402818186));
#34129=CARTESIAN_POINT('Ctrl Pts',(-0.785447890340723,-1.,-3.88691313167399));
#34130=CARTESIAN_POINT('Ctrl Pts',(-0.784478799358336,-1.,-3.89442039235105));
#34131=CARTESIAN_POINT('Ctrl Pts',(-0.783464141529082,-1.,-3.90193039043971));
#34132=CARTESIAN_POINT('Ctrl Pts',(-0.782405395622759,-1.,-3.90944671004536));
#34133=CARTESIAN_POINT('Ctrl Pts',(-0.781303428618344,-1.,-3.9169703605466));
#34134=CARTESIAN_POINT('Ctrl Pts',(-0.780158678615507,-1.,-3.92450058323799));
#34135=CARTESIAN_POINT('Ctrl Pts',(-0.778971308134786,-1.,-3.93203552473153));
#34136=CARTESIAN_POINT('Ctrl Pts',(-0.77774137056855,-1.,-3.93957296768098));
#34137=CARTESIAN_POINT('Ctrl Pts',(-0.77646896669796,-1.,-3.94711101619471));
#34138=CARTESIAN_POINT('Ctrl Pts',(-0.775154418039441,-1.,-3.95464885452364));
#34139=CARTESIAN_POINT('Ctrl Pts',(-0.773798212026683,-1.,-3.96218649639876));
#34140=CARTESIAN_POINT('Ctrl Pts',(-0.772400931772239,-1.,-3.96972446532832));
#34141=CARTESIAN_POINT('Ctrl Pts',(-0.770963190030504,-1.,-3.97726349165507));
#34142=CARTESIAN_POINT('Ctrl Pts',(-0.769485566245459,-1.,-3.98480422348403));
#34143=CARTESIAN_POINT('Ctrl Pts',(-0.767968531377708,-1.,-3.99234687880892));
#34144=CARTESIAN_POINT('Ctrl Pts',(-0.766412457135786,-1.,-3.99989129179464));
#34145=CARTESIAN_POINT('Ctrl Pts',(-0.764817648784946,-1.,-4.00743706791366));
#34146=CARTESIAN_POINT('Ctrl Pts',(-0.763184371182827,-1.,-4.01498370680434));
#34147=CARTESIAN_POINT('Ctrl Pts',(-0.761512875859942,-1.,-4.02253072741347));
#34148=CARTESIAN_POINT('Ctrl Pts',(-0.759803433244166,-1.,-4.0300778195465));
#34149=CARTESIAN_POINT('Ctrl Pts',(-0.758056338885554,-1.,-4.03762485803468));
#34150=CARTESIAN_POINT('Ctrl Pts',(-0.756271902370187,-1.,-4.04517182654344));
#34151=CARTESIAN_POINT('Ctrl Pts',(-0.754450441816412,-1.,-4.05271876688106));
#34152=CARTESIAN_POINT('Ctrl Pts',(-0.752592276482869,-1.,-4.06026572221399));
#34153=CARTESIAN_POINT('Ctrl Pts',(-0.750697720483176,-1.,-4.06781267241886));
#34154=CARTESIAN_POINT('Ctrl Pts',(-0.748767076679177,-1.,-4.07535951055363));
#34155=CARTESIAN_POINT('Ctrl Pts',(-0.746800631490822,-1.,-4.08290608094789));
#34156=CARTESIAN_POINT('Ctrl Pts',(-0.744798649705514,-1.,-4.09045220253011));
#34157=CARTESIAN_POINT('Ctrl Pts',(-0.742761369690018,-1.,-4.09799769702712));
#34158=CARTESIAN_POINT('Ctrl Pts',(-0.740688998555152,-1.,-4.1055424175856));
#34159=CARTESIAN_POINT('Ctrl Pts',(-0.738581708229119,-1.,-4.11308626953795));
#34160=CARTESIAN_POINT('Ctrl Pts',(-0.736439634335347,-1.,-4.12062919626082));
#34161=CARTESIAN_POINT('Ctrl Pts',(-0.734698226767512,-1.,-4.12666277572794));
#34162=CARTESIAN_POINT('Ctrl Pts',(-0.733376589325634,-1.,-4.13118752796397));
#34163=CARTESIAN_POINT('Ctrl Pts',(-0.732488575135926,-1.,-4.13420383737278));
#34164=CARTESIAN_POINT('Ctrl Pts',(-0.732042837400619,-1.,-4.13571194405636));
#34165=CARTESIAN_POINT('',(-0.581791163835814,-1.,-4.15950947128175));
#34166=CARTESIAN_POINT('',(-0.732042837400619,-1.,-4.13571194405636));
#34167=CARTESIAN_POINT('',(-0.385112848332549,-1.,-3.73017266276632));
#34168=CARTESIAN_POINT('Ctrl Pts',(-0.581791163835814,-1.,-4.15950947128175));
#34169=CARTESIAN_POINT('Ctrl Pts',(-0.580901211462913,-1.,-4.15821291712391));
#34170=CARTESIAN_POINT('Ctrl Pts',(-0.579124568912543,-1.,-4.15561864787379));
#34171=CARTESIAN_POINT('Ctrl Pts',(-0.576469391673917,-1.,-4.1517237611974));
#34172=CARTESIAN_POINT('Ctrl Pts',(-0.572948736066277,-1.,-4.14652361065787));
#34173=CARTESIAN_POINT('Ctrl Pts',(-0.568580610187116,-1.,-4.14001179828669));
#34174=CARTESIAN_POINT('Ctrl Pts',(-0.564245279535705,-1.,-4.13348835726086));
#34175=CARTESIAN_POINT('Ctrl Pts',(-0.559942890594628,-1.,-4.12695329951859));
#34176=CARTESIAN_POINT('Ctrl Pts',(-0.555673636130778,-1.,-4.1204066619623));
#34177=CARTESIAN_POINT('Ctrl Pts',(-0.551437758498247,-1.,-4.11384852025578));
#34178=CARTESIAN_POINT('Ctrl Pts',(-0.54723553948676,-1.,-4.1072789702877));
#34179=CARTESIAN_POINT('Ctrl Pts',(-0.543067286878457,-1.,-4.10069810244473));
#34180=CARTESIAN_POINT('Ctrl Pts',(-0.538933321179921,-1.,-4.09410597627116));
#34181=CARTESIAN_POINT('Ctrl Pts',(-0.534833963476999,-1.,-4.08750259988693));
#34182=CARTESIAN_POINT('Ctrl Pts',(-0.530769518728075,-1.,-4.08088789536488));
#34183=CARTESIAN_POINT('Ctrl Pts',(-0.526740277227,-1.,-4.07426172299496));
#34184=CARTESIAN_POINT('Ctrl Pts',(-0.522746528602768,-1.,-4.06762394471075));
#34185=CARTESIAN_POINT('Ctrl Pts',(-0.51878857233681,-1.,-4.06097448037934));
#34186=CARTESIAN_POINT('Ctrl Pts',(-0.514866728193104,-1.,-4.05431335771261));
#34187=CARTESIAN_POINT('Ctrl Pts',(-0.510981349219174,-1.,-4.04764078815591));
#34188=CARTESIAN_POINT('Ctrl Pts',(-0.507132823288362,-1.,-4.04095715149074));
#34189=CARTESIAN_POINT('Ctrl Pts',(-0.503321556915514,-1.,-4.0342628417439));
#34190=CARTESIAN_POINT('Ctrl Pts',(-0.49954796234089,-1.,-4.0275581398015));
#34191=CARTESIAN_POINT('Ctrl Pts',(-0.495812444326223,-1.,-4.02084308851813));
#34192=CARTESIAN_POINT('Ctrl Pts',(-0.492115383417931,-1.,-4.01411733503486));
#34193=CARTESIAN_POINT('Ctrl Pts',(-0.488457130424531,-1.,-4.0073800839092));
#34194=CARTESIAN_POINT('Ctrl Pts',(-0.484838042421754,-1.,-4.00063045119234));
#34195=CARTESIAN_POINT('Ctrl Pts',(-0.481258512209638,-1.,-3.99386775880655));
#34196=CARTESIAN_POINT('Ctrl Pts',(-0.477718999122033,-1.,-3.98709184306743));
#34197=CARTESIAN_POINT('Ctrl Pts',(-0.474220061019542,-1.,-3.9803033804443));
#34198=CARTESIAN_POINT('Ctrl Pts',(-0.470762379613477,-1.,-3.97350414289415));
#34199=CARTESIAN_POINT('Ctrl Pts',(-0.467346690880672,-1.,-3.96669622273946));
#34200=CARTESIAN_POINT('Ctrl Pts',(-0.463973722115744,-1.,-3.95988133243543));
#34201=CARTESIAN_POINT('Ctrl Pts',(-0.460644124429119,-1.,-3.95306005817363));
#34202=CARTESIAN_POINT('Ctrl Pts',(-0.457358410451674,-1.,-3.94623117206675));
#34203=CARTESIAN_POINT('Ctrl Pts',(-0.454116879027576,-1.,-3.93939080846298));
#34204=CARTESIAN_POINT('Ctrl Pts',(-0.450919768356347,-1.,-3.93253407403128));
#34205=CARTESIAN_POINT('Ctrl Pts',(-0.447767416837297,-1.,-3.92565674143424));
#34206=CARTESIAN_POINT('Ctrl Pts',(-0.444660430230593,-1.,-3.91875701610721));
#34207=CARTESIAN_POINT('Ctrl Pts',(-0.441599824524047,-1.,-3.91183704069146));
#34208=CARTESIAN_POINT('Ctrl Pts',(-0.438587235458233,-1.,-3.90490512938546));
#34209=CARTESIAN_POINT('Ctrl Pts',(-0.435624629433506,-1.,-3.8979725665544));
#34210=CARTESIAN_POINT('Ctrl Pts',(-0.432713929544439,-1.,-3.89104947940592));
#34211=CARTESIAN_POINT('Ctrl Pts',(-0.429856640579734,-1.,-3.88414070943334));
#34212=CARTESIAN_POINT('Ctrl Pts',(-0.427053541173469,-1.,-3.87724240306609));
#34213=CARTESIAN_POINT('Ctrl Pts',(-0.424304173195142,-1.,-3.87033643487882));
#34214=CARTESIAN_POINT('Ctrl Pts',(-0.421607423177576,-1.,-3.86339652542749));
#34215=CARTESIAN_POINT('Ctrl Pts',(-0.41896246808681,-1.,-3.85639825648031));
#34216=CARTESIAN_POINT('Ctrl Pts',(-0.41636967805292,-1.,-3.8493286415751));
#34217=CARTESIAN_POINT('Ctrl Pts',(-0.413831367016727,-1.,-3.84219403994742));
#34218=CARTESIAN_POINT('Ctrl Pts',(-0.41135303879846,-1.,-3.83503345578645));
#34219=CARTESIAN_POINT('Ctrl Pts',(-0.408942371447377,-1.,-3.82790724256397));
#34220=CARTESIAN_POINT('Ctrl Pts',(-0.406607038258906,-1.,-3.82087303913741));
#34221=CARTESIAN_POINT('Ctrl Pts',(-0.404352694628236,-1.,-3.81396374287762));
#34222=CARTESIAN_POINT('Ctrl Pts',(-0.402181320148475,-1.,-3.80716881962763));
#34223=CARTESIAN_POINT('Ctrl Pts',(-0.400088346504727,-1.,-3.80040370384659));
#34224=CARTESIAN_POINT('Ctrl Pts',(-0.398064818684158,-1.,-3.79352887163457));
#34225=CARTESIAN_POINT('Ctrl Pts',(-0.396103205335029,-1.,-3.78640521279479));
#34226=CARTESIAN_POINT('Ctrl Pts',(-0.394202481011595,-1.,-3.77894173114368));
#34227=CARTESIAN_POINT('Ctrl Pts',(-0.392372786223347,-1.,-3.77114011595892));
#34228=CARTESIAN_POINT('Ctrl Pts',(-0.390642072979259,-1.,-3.76315635032993));
#34229=CARTESIAN_POINT('Ctrl Pts',(-0.389054775898251,-1.,-3.75529302894757));
#34230=CARTESIAN_POINT('Ctrl Pts',(-0.387663020050396,-1.,-3.74792651696269));
#34231=CARTESIAN_POINT('Ctrl Pts',(-0.386519576222035,-1.,-3.74144965781088));
#34232=CARTESIAN_POINT('Ctrl Pts',(-0.385670806454744,-1.,-3.73621371845475));
#34233=CARTESIAN_POINT('Ctrl Pts',(-0.385187124633965,-1.,-3.73273893363318));
#34234=CARTESIAN_POINT('Ctrl Pts',(-0.385031656499141,-1.,-3.73106082862399));
#34235=CARTESIAN_POINT('Ctrl Pts',(-0.385037797882046,-1.,-3.73040527620929));
#34236=CARTESIAN_POINT('Ctrl Pts',(-0.385087139001609,-1.,-3.73021431755218));
#34237=CARTESIAN_POINT('Ctrl Pts',(-0.385112848332549,-1.,-3.73017266276632));
#34238=CARTESIAN_POINT('',(-0.203156094897896,-1.,-3.74449296982994));
#34239=CARTESIAN_POINT('Origin',(0.,-1.,0.));
#34240=CARTESIAN_POINT('',(-0.0760622897878238,-1.,-4.19931119685982));
#34241=CARTESIAN_POINT('Ctrl Pts',(-0.203156094897896,-1.,-3.74449296982994));
#34242=CARTESIAN_POINT('Ctrl Pts',(-0.203188003947965,-1.,-3.74453008995129));
#34243=CARTESIAN_POINT('Ctrl Pts',(-0.203266610111264,-1.,-3.74471097893961));
#34244=CARTESIAN_POINT('Ctrl Pts',(-0.203375226874331,-1.,-3.74535749969262));
#34245=CARTESIAN_POINT('Ctrl Pts',(-0.203484186269315,-1.,-3.74703926501843));
#34246=CARTESIAN_POINT('Ctrl Pts',(-0.203550035479097,-1.,-3.75054693397716));
#34247=CARTESIAN_POINT('Ctrl Pts',(-0.203530796848404,-1.,-3.75585118707924));
#34248=CARTESIAN_POINT('Ctrl Pts',(-0.203414634707646,-1.,-3.76242717937273));
#34249=CARTESIAN_POINT('Ctrl Pts',(-0.203192390045337,-1.,-3.76992071595267));
#34250=CARTESIAN_POINT('Ctrl Pts',(-0.202854729699197,-1.,-3.77793553476879));
#34251=CARTESIAN_POINT('Ctrl Pts',(-0.202394260512193,-1.,-3.78609175019317));
#34252=CARTESIAN_POINT('Ctrl Pts',(-0.201807533800799,-1.,-3.79408354187274));
#34253=CARTESIAN_POINT('Ctrl Pts',(-0.201097756307252,-1.,-3.80175247447171));
#34254=CARTESIAN_POINT('Ctrl Pts',(-0.20027467943329,-1.,-3.80909529318501));
#34255=CARTESIAN_POINT('Ctrl Pts',(-0.199351525297396,-1.,-3.81620203429702));
#34256=CARTESIAN_POINT('Ctrl Pts',(-0.19834261690047,-1.,-3.82321127348981));
#34257=CARTESIAN_POINT('Ctrl Pts',(-0.197260935827375,-1.,-3.83026221776488));
#34258=CARTESIAN_POINT('Ctrl Pts',(-0.19611519897189,-1.,-3.83743910616265));
#34259=CARTESIAN_POINT('Ctrl Pts',(-0.194909009460255,-1.,-3.84475203347052));
#34260=CARTESIAN_POINT('Ctrl Pts',(-0.193642806777748,-1.,-3.85216762264019));
#34261=CARTESIAN_POINT('Ctrl Pts',(-0.19231515304498,-1.,-3.85962774407652));
#34262=CARTESIAN_POINT('Ctrl Pts',(-0.190924190418613,-1.,-3.8670715862477));
#34263=CARTESIAN_POINT('Ctrl Pts',(-0.189469253358254,-1.,-3.87445976418377));
#34264=CARTESIAN_POINT('Ctrl Pts',(-0.187951632512663,-1.,-3.88178563496187));
#34265=CARTESIAN_POINT('Ctrl Pts',(-0.186373724985263,-1.,-3.88906196725817));
#34266=CARTESIAN_POINT('Ctrl Pts',(-0.184738537728035,-1.,-3.89631300742633));
#34267=CARTESIAN_POINT('Ctrl Pts',(-0.183049081993193,-1.,-3.90356488555138));
#34268=CARTESIAN_POINT('Ctrl Pts',(-0.181307740731796,-1.,-3.91083557557193));
#34269=CARTESIAN_POINT('Ctrl Pts',(-0.179515885822895,-1.,-3.91812876180948));
#34270=CARTESIAN_POINT('Ctrl Pts',(-0.177674246152328,-1.,-3.92543942697672));
#34271=CARTESIAN_POINT('Ctrl Pts',(-0.175783136893873,-1.,-3.93275726771049));
#34272=CARTESIAN_POINT('Ctrl Pts',(-0.173842734974607,-1.,-3.94007083096214));
#34273=CARTESIAN_POINT('Ctrl Pts',(-0.171853355369233,-1.,-3.94737164900861));
#34274=CARTESIAN_POINT('Ctrl Pts',(-0.16981566637413,-1.,-3.95465744665263));
#34275=CARTESIAN_POINT('Ctrl Pts',(-0.167730547023312,-1.,-3.96192990160296));
#34276=CARTESIAN_POINT('Ctrl Pts',(-0.165598992851098,-1.,-3.9691931362141));
#34277=CARTESIAN_POINT('Ctrl Pts',(-0.163422004609999,-1.,-3.97645194630944));
#34278=CARTESIAN_POINT('Ctrl Pts',(-0.161200482186088,-1.,-3.98371010319866));
#34279=CARTESIAN_POINT('Ctrl Pts',(-0.158935123982796,-1.,-3.99096873945862));
#34280=CARTESIAN_POINT('Ctrl Pts',(-0.156626481393736,-1.,-3.99822717425869));
#34281=CARTESIAN_POINT('Ctrl Pts',(-0.15427500487231,-1.,-4.00548360245297));
#34282=CARTESIAN_POINT('Ctrl Pts',(-0.151881094022909,-1.,-4.01273584234684));
#34283=CARTESIAN_POINT('Ctrl Pts',(-0.149445144968708,-1.,-4.01998203715588));
#34284=CARTESIAN_POINT('Ctrl Pts',(-0.146967602878999,-1.,-4.02722143147048));
#34285=CARTESIAN_POINT('Ctrl Pts',(-0.144448947038352,-1.,-4.03445411510403));
#34286=CARTESIAN_POINT('Ctrl Pts',(-0.141889671485508,-1.,-4.04168069633842));
#34287=CARTESIAN_POINT('Ctrl Pts',(-0.13929026718006,-1.,-4.04890199238056));
#34288=CARTESIAN_POINT('Ctrl Pts',(-0.136651205046111,-1.,-4.05611873400122));
#34289=CARTESIAN_POINT('Ctrl Pts',(-0.133972916144225,-1.,-4.06333121018476));
#34290=CARTESIAN_POINT('Ctrl Pts',(-0.131255793548914,-1.,-4.07053931528579));
#34291=CARTESIAN_POINT('Ctrl Pts',(-0.128500200484814,-1.,-4.07774270738809));
#34292=CARTESIAN_POINT('Ctrl Pts',(-0.125706476822529,-1.,-4.08494093372315));
#34293=CARTESIAN_POINT('Ctrl Pts',(-0.122874946249119,-1.,-4.09213355850836));
#34294=CARTESIAN_POINT('Ctrl Pts',(-0.120005924388162,-1.,-4.09932031767243));
#34295=CARTESIAN_POINT('Ctrl Pts',(-0.117099722731705,-1.,-4.10650113382187));
#34296=CARTESIAN_POINT('Ctrl Pts',(-0.114156649609602,-1.,-4.11367603925313));
#34297=CARTESIAN_POINT('Ctrl Pts',(-0.111177012683377,-1.,-4.12084512502444));
#34298=CARTESIAN_POINT('Ctrl Pts',(-0.10816112052835,-1.,-4.12800848371386));
#34299=CARTESIAN_POINT('Ctrl Pts',(-0.105109286538864,-1.,-4.13516614458396));
#34300=CARTESIAN_POINT('Ctrl Pts',(-0.102021826577454,-1.,-4.14231804938737));
#34301=CARTESIAN_POINT('Ctrl Pts',(-0.0988990478899814,-1.,-4.1494640891762));
#34302=CARTESIAN_POINT('Ctrl Pts',(-0.095741240329707,-1.,-4.15660412653006));
#34303=CARTESIAN_POINT('Ctrl Pts',(-0.0925486672167692,-1.,-4.16373802265942));
#34304=CARTESIAN_POINT('Ctrl Pts',(-0.089321556085033,-1.,-4.17086566491823));
#34305=CARTESIAN_POINT('Ctrl Pts',(-0.0860600915552517,-1.,-4.17798698669991));
#34306=CARTESIAN_POINT('Ctrl Pts',(-0.0827644164389512,-1.,-4.1851019532944));
#34307=CARTESIAN_POINT('Ctrl Pts',(-0.0801005887117605,-1.,-4.19078883322483));
#34308=CARTESIAN_POINT('Ctrl Pts',(-0.0780873956244405,-1.,-4.19505112860624));
#34309=CARTESIAN_POINT('Ctrl Pts',(-0.0767384596142197,-1.,-4.19789138621624));
#34310=CARTESIAN_POINT('Ctrl Pts',(-0.0760622897878238,-1.,-4.19931119685982));
#34311=CARTESIAN_POINT('',(0.0760622897878244,-1.,-4.19931119685982));
#34312=CARTESIAN_POINT('',(-0.0760622897878238,-1.,-4.19931119685982));
#34313=CARTESIAN_POINT('',(0.2031560948961,-1.,-3.74449296983004));
#34314=CARTESIAN_POINT('Ctrl Pts',(0.0760622897878244,-1.,-4.19931119685982));
#34315=CARTESIAN_POINT('Ctrl Pts',(0.0767384596141462,-1.,-4.1978913862118));
#34316=CARTESIAN_POINT('Ctrl Pts',(0.0780873956242395,-1.,-4.19505112859416));
#34317=CARTESIAN_POINT('Ctrl Pts',(0.0801005887114317,-1.,-4.19078883320504));
#34318=CARTESIAN_POINT('Ctrl Pts',(0.0827644164385676,-1.,-4.18510195327123));
#34319=CARTESIAN_POINT('Ctrl Pts',(0.0860600915549394,-1.,-4.17798698668094));
#34320=CARTESIAN_POINT('Ctrl Pts',(0.0893215560848647,-1.,-4.17086566490794));
#34321=CARTESIAN_POINT('Ctrl Pts',(0.0925486672167528,-1.,-4.16373802265839));
#34322=CARTESIAN_POINT('Ctrl Pts',(0.0957412403298004,-1.,-4.15660412653577));
#34323=CARTESIAN_POINT('Ctrl Pts',(0.0988990478901223,-1.,-4.14946408918485));
#34324=CARTESIAN_POINT('Ctrl Pts',(0.102021826577584,-1.,-4.14231804939538));
#34325=CARTESIAN_POINT('Ctrl Pts',(0.105109286538945,-1.,-4.13516614458895));
#34326=CARTESIAN_POINT('Ctrl Pts',(0.108161120528369,-1.,-4.12800848371504));
#34327=CARTESIAN_POINT('Ctrl Pts',(0.111177012683346,-1.,-4.1208451250225));
#34328=CARTESIAN_POINT('Ctrl Pts',(0.114156649609545,-1.,-4.11367603924961));
#34329=CARTESIAN_POINT('Ctrl Pts',(0.117099722731648,-1.,-4.10650113381833));
#34330=CARTESIAN_POINT('Ctrl Pts',(0.120005924388124,-1.,-4.09932031767002));
#34331=CARTESIAN_POINT('Ctrl Pts',(0.122874946249107,-1.,-4.09213355850756));
#34332=CARTESIAN_POINT('Ctrl Pts',(0.12570647682254,-1.,-4.08494093372377));
#34333=CARTESIAN_POINT('Ctrl Pts',(0.128500200484837,-1.,-4.07774270738954));
#34334=CARTESIAN_POINT('Ctrl Pts',(0.13125579354894,-1.,-4.0705393152874));
#34335=CARTESIAN_POINT('Ctrl Pts',(0.133972916144245,-1.,-4.06333121018596));
#34336=CARTESIAN_POINT('Ctrl Pts',(0.136651205046119,-1.,-4.05611873400172));
#34337=CARTESIAN_POINT('Ctrl Pts',(0.139290267180057,-1.,-4.04890199238036));
#34338=CARTESIAN_POINT('Ctrl Pts',(0.1418896714855,-1.,-4.04168069633781));
#34339=CARTESIAN_POINT('Ctrl Pts',(0.144448947038344,-1.,-4.03445411510333));
#34340=CARTESIAN_POINT('Ctrl Pts',(0.146967602878994,-1.,-4.02722143146994));
#34341=CARTESIAN_POINT('Ctrl Pts',(0.149445144968707,-1.,-4.01998203715564));
#34342=CARTESIAN_POINT('Ctrl Pts',(0.15188109402291,-1.,-4.01273584234689));
#34343=CARTESIAN_POINT('Ctrl Pts',(0.15427500487231,-1.,-4.00548360245319));
#34344=CARTESIAN_POINT('Ctrl Pts',(0.156626481393734,-1.,-3.99822717425893));
#34345=CARTESIAN_POINT('Ctrl Pts',(0.158935123982793,-1.,-3.99096873945878));
#34346=CARTESIAN_POINT('Ctrl Pts',(0.161200482186084,-1.,-3.98371010319872));
#34347=CARTESIAN_POINT('Ctrl Pts',(0.163422004609999,-1.,-3.97645194630943));
#34348=CARTESIAN_POINT('Ctrl Pts',(0.165598992851102,-1.,-3.96919313621407));
#34349=CARTESIAN_POINT('Ctrl Pts',(0.167730547023319,-1.,-3.96192990160296));
#34350=CARTESIAN_POINT('Ctrl Pts',(0.169815666374139,-1.,-3.95465744665268));
#34351=CARTESIAN_POINT('Ctrl Pts',(0.17185335536924,-1.,-3.94737164900868));
#34352=CARTESIAN_POINT('Ctrl Pts',(0.173842734974609,-1.,-3.94007083096217));
#34353=CARTESIAN_POINT('Ctrl Pts',(0.175783136893868,-1.,-3.93275726771042));
#34354=CARTESIAN_POINT('Ctrl Pts',(0.177674246152317,-1.,-3.92543942697655));
#34355=CARTESIAN_POINT('Ctrl Pts',(0.179515885822881,-1.,-3.91812876180926));
#34356=CARTESIAN_POINT('Ctrl Pts',(0.181307740731785,-1.,-3.91083557557175));
#34357=CARTESIAN_POINT('Ctrl Pts',(0.18304908199319,-1.,-3.90356488555132));
#34358=CARTESIAN_POINT('Ctrl Pts',(0.184738537728043,-1.,-3.89631300742646));
#34359=CARTESIAN_POINT('Ctrl Pts',(0.18637372498528,-1.,-3.88906196725848));
#34360=CARTESIAN_POINT('Ctrl Pts',(0.187951632512685,-1.,-3.88178563496228));
#34361=CARTESIAN_POINT('Ctrl Pts',(0.189469253358272,-1.,-3.87445976418412));
#34362=CARTESIAN_POINT('Ctrl Pts',(0.19092419041862,-1.,-3.86707158624783));
#34363=CARTESIAN_POINT('Ctrl Pts',(0.19231515304497,-1.,-3.85962774407633));
#34364=CARTESIAN_POINT('Ctrl Pts',(0.193642806777723,-1.,-3.85216762263966));
#34365=CARTESIAN_POINT('Ctrl Pts',(0.19490900946022,-1.,-3.84475203346977));
#34366=CARTESIAN_POINT('Ctrl Pts',(0.196115198971859,-1.,-3.83743910616195));
#34367=CARTESIAN_POINT('Ctrl Pts',(0.197260935827361,-1.,-3.83026221776456));
#34368=CARTESIAN_POINT('Ctrl Pts',(0.198342616900486,-1.,-3.82321127349016));
#34369=CARTESIAN_POINT('Ctrl Pts',(0.199351525297447,-1.,-3.81620203429815));
#34370=CARTESIAN_POINT('Ctrl Pts',(0.200274679433364,-1.,-3.80909529318669));
#34371=CARTESIAN_POINT('Ctrl Pts',(0.201097756307326,-1.,-3.80175247447337));
#34372=CARTESIAN_POINT('Ctrl Pts',(0.201807533800837,-1.,-3.7940835418736));
#34373=CARTESIAN_POINT('Ctrl Pts',(0.20239426051216,-1.,-3.78609175019242));
#34374=CARTESIAN_POINT('Ctrl Pts',(0.202854729699081,-1.,-3.77793553476614));
#34375=CARTESIAN_POINT('Ctrl Pts',(0.203192390045164,-1.,-3.7699207159487));
#34376=CARTESIAN_POINT('Ctrl Pts',(0.203414634707478,-1.,-3.76242717936885));
#34377=CARTESIAN_POINT('Ctrl Pts',(0.203530796848321,-1.,-3.75585118707734));
#34378=CARTESIAN_POINT('Ctrl Pts',(0.203550035479166,-1.,-3.75054693397875));
#34379=CARTESIAN_POINT('Ctrl Pts',(0.203484186269415,-1.,-3.74703926501752));
#34380=CARTESIAN_POINT('Ctrl Pts',(0.203375226874121,-1.,-3.74535749969115));
#34381=CARTESIAN_POINT('Ctrl Pts',(0.203266610110531,-1.,-3.74471097893845));
#34382=CARTESIAN_POINT('Ctrl Pts',(0.203188003946657,-1.,-3.74453008995092));
#34383=CARTESIAN_POINT('Ctrl Pts',(0.2031560948961,-1.,-3.74449296983004));
#34384=CARTESIAN_POINT('',(0.385112848330761,-1.,-3.73017266276651));
#34385=CARTESIAN_POINT('Origin',(0.,-1.,0.));
#34386=CARTESIAN_POINT('',(0.581791163835815,-1.,-4.15950947128175));
#34387=CARTESIAN_POINT('Ctrl Pts',(0.385112848330761,-1.,-3.73017266276651));
#34388=CARTESIAN_POINT('Ctrl Pts',(0.385087139000374,-1.,-3.73021431755274));
#34389=CARTESIAN_POINT('Ctrl Pts',(0.385037797881504,-1.,-3.73040527621055));
#34390=CARTESIAN_POINT('Ctrl Pts',(0.385031656499164,-1.,-3.73106082862548));
#34391=CARTESIAN_POINT('Ctrl Pts',(0.385187124634206,-1.,-3.73273893363406));
#34392=CARTESIAN_POINT('Ctrl Pts',(0.385670806454565,-1.,-3.73621371845318));
#34393=CARTESIAN_POINT('Ctrl Pts',(0.386519576222251,-1.,-3.74144965781276));
#34394=CARTESIAN_POINT('Ctrl Pts',(0.387663020050836,-1.,-3.74792651696654));
#34395=CARTESIAN_POINT('Ctrl Pts',(0.389054775898701,-1.,-3.75529302895152));
#34396=CARTESIAN_POINT('Ctrl Pts',(0.390642072979559,-1.,-3.76315635033257));
#34397=CARTESIAN_POINT('Ctrl Pts',(0.392372786223432,-1.,-3.77114011595967));
#34398=CARTESIAN_POINT('Ctrl Pts',(0.394202481011499,-1.,-3.77894173114283));
#34399=CARTESIAN_POINT('Ctrl Pts',(0.39610320533484,-1.,-3.78640521279313));
#34400=CARTESIAN_POINT('Ctrl Pts',(0.398064818683969,-1.,-3.7935288716329));
#34401=CARTESIAN_POINT('Ctrl Pts',(0.4000883465046,-1.,-3.80040370384546));
#34402=CARTESIAN_POINT('Ctrl Pts',(0.402181320148435,-1.,-3.80716881962728));
#34403=CARTESIAN_POINT('Ctrl Pts',(0.404352694628273,-1.,-3.81396374287793));
#34404=CARTESIAN_POINT('Ctrl Pts',(0.406607038258985,-1.,-3.8208730391381));
#34405=CARTESIAN_POINT('Ctrl Pts',(0.408942371447459,-1.,-3.82790724256471));
#34406=CARTESIAN_POINT('Ctrl Pts',(0.411353038798518,-1.,-3.83503345578698));
#34407=CARTESIAN_POINT('Ctrl Pts',(0.413831367016748,-1.,-3.84219403994762));
#34408=CARTESIAN_POINT('Ctrl Pts',(0.416369678052906,-1.,-3.84932864157497));
#34409=CARTESIAN_POINT('Ctrl Pts',(0.418962468086773,-1.,-3.85639825647996));
#34410=CARTESIAN_POINT('Ctrl Pts',(0.421607423177534,-1.,-3.86339652542709));
#34411=CARTESIAN_POINT('Ctrl Pts',(0.42430417319511,-1.,-3.87033643487851));
#34412=CARTESIAN_POINT('Ctrl Pts',(0.427053541173457,-1.,-3.87724240306597));
#34413=CARTESIAN_POINT('Ctrl Pts',(0.429856640579741,-1.,-3.88414070943341));
#34414=CARTESIAN_POINT('Ctrl Pts',(0.432713929544458,-1.,-3.89104947940611));
#34415=CARTESIAN_POINT('Ctrl Pts',(0.435624629433527,-1.,-3.89797256655462));
#34416=CARTESIAN_POINT('Ctrl Pts',(0.438587235458249,-1.,-3.90490512938563));
#34417=CARTESIAN_POINT('Ctrl Pts',(0.441599824524054,-1.,-3.91183704069153));
#34418=CARTESIAN_POINT('Ctrl Pts',(0.44466043023059,-1.,-3.91875701610719));
#34419=CARTESIAN_POINT('Ctrl Pts',(0.447767416837292,-1.,-3.92565674143416));
#34420=CARTESIAN_POINT('Ctrl Pts',(0.450919768356348,-1.,-3.93253407403123));
#34421=CARTESIAN_POINT('Ctrl Pts',(0.454116879027584,-1.,-3.93939080846298));
#34422=CARTESIAN_POINT('Ctrl Pts',(0.457358410451682,-1.,-3.94623117206678));
#34423=CARTESIAN_POINT('Ctrl Pts',(0.460644124429121,-1.,-3.95306005817364));
#34424=CARTESIAN_POINT('Ctrl Pts',(0.463973722115733,-1.,-3.95988133243538));
#34425=CARTESIAN_POINT('Ctrl Pts',(0.467346690880643,-1.,-3.9666962227393));
#34426=CARTESIAN_POINT('Ctrl Pts',(0.470762379613439,-1.,-3.97350414289392));
#34427=CARTESIAN_POINT('Ctrl Pts',(0.474220061019509,-1.,-3.98030338044409));
#34428=CARTESIAN_POINT('Ctrl Pts',(0.477718999122027,-1.,-3.98709184306738));
#34429=CARTESIAN_POINT('Ctrl Pts',(0.481258512209675,-1.,-3.99386775880679));
#34430=CARTESIAN_POINT('Ctrl Pts',(0.484838042421834,-1.,-4.00063045119288));
#34431=CARTESIAN_POINT('Ctrl Pts',(0.488457130424633,-1.,-4.0073800839099));
#34432=CARTESIAN_POINT('Ctrl Pts',(0.492115383418018,-1.,-4.01411733503546));
#34433=CARTESIAN_POINT('Ctrl Pts',(0.495812444326251,-1.,-4.02084308851832));
#34434=CARTESIAN_POINT('Ctrl Pts',(0.499547962340821,-1.,-4.02755813980101));
#34435=CARTESIAN_POINT('Ctrl Pts',(0.503321556915346,-1.,-4.03426284174272));
#34436=CARTESIAN_POINT('Ctrl Pts',(0.507132823288136,-1.,-4.04095715148915));
#34437=CARTESIAN_POINT('Ctrl Pts',(0.51098134921897,-1.,-4.04764078815447));
#34438=CARTESIAN_POINT('Ctrl Pts',(0.514866728193016,-1.,-4.05431335771199));
#34439=CARTESIAN_POINT('Ctrl Pts',(0.518788572336923,-1.,-4.06097448038013));
#34440=CARTESIAN_POINT('Ctrl Pts',(0.522746528603107,-1.,-4.06762394471314));
#34441=CARTESIAN_POINT('Ctrl Pts',(0.526740277227498,-1.,-4.07426172299847));
#34442=CARTESIAN_POINT('Ctrl Pts',(0.53076951872857,-1.,-4.08088789536836));
#34443=CARTESIAN_POINT('Ctrl Pts',(0.534833963477273,-1.,-4.08750259988885));
#34444=CARTESIAN_POINT('Ctrl Pts',(0.538933321179755,-1.,-4.09410597627));
#34445=CARTESIAN_POINT('Ctrl Pts',(0.543067286877757,-1.,-4.10069810243979));
#34446=CARTESIAN_POINT('Ctrl Pts',(0.547235539485636,-1.,-4.10727897027977));
#34447=CARTESIAN_POINT('Ctrl Pts',(0.551437758497032,-1.,-4.11384852024721));
#34448=CARTESIAN_POINT('Ctrl Pts',(0.555673636129977,-1.,-4.12040666195664));
#34449=CARTESIAN_POINT('Ctrl Pts',(0.559942890594773,-1.,-4.12695329951961));
#34450=CARTESIAN_POINT('Ctrl Pts',(0.564245279537148,-1.,-4.13348835727104));
#34451=CARTESIAN_POINT('Ctrl Pts',(0.568580610189774,-1.,-4.14001179830547));
#34452=CARTESIAN_POINT('Ctrl Pts',(0.572948736069522,-1.,-4.14652361068081));
#34453=CARTESIAN_POINT('Ctrl Pts',(0.576469391676688,-1.,-4.151723761217));
#34454=CARTESIAN_POINT('Ctrl Pts',(0.579124568914235,-1.,-4.15561864788576));
#34455=CARTESIAN_POINT('Ctrl Pts',(0.580901211463535,-1.,-4.1582129171283));
#34456=CARTESIAN_POINT('Ctrl Pts',(0.581791163835815,-1.,-4.15950947128175));
#34457=CARTESIAN_POINT('',(0.73204283740062,-1.,-4.13571194405636));
#34458=CARTESIAN_POINT('',(0.581791163835815,-1.,-4.15950947128175));
#34459=CARTESIAN_POINT('',(0.786422660831985,-1.,-3.66661143271685));
#34460=CARTESIAN_POINT('Ctrl Pts',(0.73204283740062,-1.,-4.13571194405636));
#34461=CARTESIAN_POINT('Ctrl Pts',(0.732488575135159,-1.,-4.1342038373684));
#34462=CARTESIAN_POINT('Ctrl Pts',(0.733376589323546,-1.,-4.13118752795207));
#34463=CARTESIAN_POINT('Ctrl Pts',(0.734698226764092,-1.,-4.12666277570844));
#34464=CARTESIAN_POINT('Ctrl Pts',(0.736439634331344,-1.,-4.120629196238));
#34465=CARTESIAN_POINT('Ctrl Pts',(0.738581708225843,-1.,-4.11308626951927));
#34466=CARTESIAN_POINT('Ctrl Pts',(0.740688998553376,-1.,-4.10554241757547));
#34467=CARTESIAN_POINT('Ctrl Pts',(0.742761369689841,-1.,-4.09799769702611));
#34468=CARTESIAN_POINT('Ctrl Pts',(0.7447986497065,-1.,-4.09045220253573));
#34469=CARTESIAN_POINT('Ctrl Pts',(0.746800631492315,-1.,-4.08290608095642));
#34470=CARTESIAN_POINT('Ctrl Pts',(0.748767076680557,-1.,-4.07535951056152));
#34471=CARTESIAN_POINT('Ctrl Pts',(0.750697720484036,-1.,-4.06781267242378));
#34472=CARTESIAN_POINT('Ctrl Pts',(0.752592276483072,-1.,-4.06026572221515));
#34473=CARTESIAN_POINT('Ctrl Pts',(0.754450441816078,-1.,-4.05271876687915));
#34474=CARTESIAN_POINT('Ctrl Pts',(0.75627190236958,-1.,-4.04517182653997));
#34475=CARTESIAN_POINT('Ctrl Pts',(0.758056338884944,-1.,-4.03762485803119));
#34476=CARTESIAN_POINT('Ctrl Pts',(0.759803433243751,-1.,-4.03007781954412));
#34477=CARTESIAN_POINT('Ctrl Pts',(0.761512875859804,-1.,-4.02253072741268));
#34478=CARTESIAN_POINT('Ctrl Pts',(0.763184371182935,-1.,-4.01498370680496));
#34479=CARTESIAN_POINT('Ctrl Pts',(0.764817648785197,-1.,-4.00743706791509));
#34480=CARTESIAN_POINT('Ctrl Pts',(0.766412457136063,-1.,-3.99989129179622));
#34481=CARTESIAN_POINT('Ctrl Pts',(0.767968531377914,-1.,-3.9923468788101));
#34482=CARTESIAN_POINT('Ctrl Pts',(0.769485566245544,-1.,-3.98480422348451));
#34483=CARTESIAN_POINT('Ctrl Pts',(0.77096319003047,-1.,-3.97726349165488));
#34484=CARTESIAN_POINT('Ctrl Pts',(0.772400931772136,-1.,-3.96972446532772));
#34485=CARTESIAN_POINT('Ctrl Pts',(0.773798212026565,-1.,-3.96218649639807));
#34486=CARTESIAN_POINT('Ctrl Pts',(0.775154418039351,-1.,-3.9546488545231));
#34487=CARTESIAN_POINT('Ctrl Pts',(0.776468966697921,-1.,-3.94711101619447));
#34488=CARTESIAN_POINT('Ctrl Pts',(0.777741370568558,-1.,-3.93957296768103));
#34489=CARTESIAN_POINT('Ctrl Pts',(0.77897130813482,-1.,-3.93203552473174));
#34490=CARTESIAN_POINT('Ctrl Pts',(0.780158678615542,-1.,-3.92450058323823));
#34491=CARTESIAN_POINT('Ctrl Pts',(0.781303428618366,-1.,-3.91697036054676));
#34492=CARTESIAN_POINT('Ctrl Pts',(0.782405395622764,-1.,-3.90944671004542));
#34493=CARTESIAN_POINT('Ctrl Pts',(0.783464141529081,-1.,-3.9019303904397));
#34494=CARTESIAN_POINT('Ctrl Pts',(0.784478799358336,-1.,-3.89442039235103));
#34495=CARTESIAN_POINT('Ctrl Pts',(0.78544789034073,-1.,-3.88691313167398));
#34496=CARTESIAN_POINT('Ctrl Pts',(0.786369675812608,-1.,-3.8794040281819));
#34497=CARTESIAN_POINT('Ctrl Pts',(0.787242527617999,-1.,-3.87188916600912));
#34498=CARTESIAN_POINT('Ctrl Pts',(0.788065315093777,-1.,-3.86436702561345));
#34499=CARTESIAN_POINT('Ctrl Pts',(0.788837734090671,-1.,-3.85683995872529));
#34500=CARTESIAN_POINT('Ctrl Pts',(0.789560798155582,-1.,-3.84931637808894));
#34501=CARTESIAN_POINT('Ctrl Pts',(0.790236124191242,-1.,-3.84180762342454));
#34502=CARTESIAN_POINT('Ctrl Pts',(0.7908650127053,-1.,-3.83432392054786));
#34503=CARTESIAN_POINT('Ctrl Pts',(0.791447528662369,-1.,-3.82687033899792));
#34504=CARTESIAN_POINT('Ctrl Pts',(0.791981740718634,-1.,-3.81944345442249));
#34505=CARTESIAN_POINT('Ctrl Pts',(0.792462483517634,-1.,-3.81202588694756));
#34506=CARTESIAN_POINT('Ctrl Pts',(0.792882695234777,-1.,-3.80459229925637));
#34507=CARTESIAN_POINT('Ctrl Pts',(0.793235612973273,-1.,-3.79711921389897));
#34508=CARTESIAN_POINT('Ctrl Pts',(0.793516871680993,-1.,-3.78959439439235));
#34509=CARTESIAN_POINT('Ctrl Pts',(0.7937262357813,-1.,-3.78202460377598));
#34510=CARTESIAN_POINT('Ctrl Pts',(0.793870523787407,-1.,-3.77444863801212));
#34511=CARTESIAN_POINT('Ctrl Pts',(0.793961083688991,-1.,-3.76692626931111));
#34512=CARTESIAN_POINT('Ctrl Pts',(0.794008429134907,-1.,-3.75951468666257));
#34513=CARTESIAN_POINT('Ctrl Pts',(0.794017347371377,-1.,-3.75224692493864));
#34514=CARTESIAN_POINT('Ctrl Pts',(0.793982700459951,-1.,-3.74511357728861));
#34515=CARTESIAN_POINT('Ctrl Pts',(0.793882700937016,-1.,-3.73803280541687));
#34516=CARTESIAN_POINT('Ctrl Pts',(0.793682750269684,-1.,-3.73086914695805));
#34517=CARTESIAN_POINT('Ctrl Pts',(0.793347023784204,-1.,-3.72348797293734));
#34518=CARTESIAN_POINT('Ctrl Pts',(0.792848377370287,-1.,-3.71580242396124));
#34519=CARTESIAN_POINT('Ctrl Pts',(0.792177688845817,-1.,-3.70781724021806));
#34520=CARTESIAN_POINT('Ctrl Pts',(0.79135657569598,-1.,-3.69968940808721));
#34521=CARTESIAN_POINT('Ctrl Pts',(0.790436284988787,-1.,-3.69172044327364));
#34522=CARTESIAN_POINT('Ctrl Pts',(0.789483546064386,-1.,-3.68428439783905));
#34523=CARTESIAN_POINT('Ctrl Pts',(0.788569566220285,-1.,-3.67777119516252));
#34524=CARTESIAN_POINT('Ctrl Pts',(0.787758799995742,-1.,-3.67252923663655));
#34525=CARTESIAN_POINT('Ctrl Pts',(0.787145041181545,-1.,-3.66907505398677));
#34526=CARTESIAN_POINT('Ctrl Pts',(0.786774337198062,-1.,-3.66743103898702));
#34527=CARTESIAN_POINT('Ctrl Pts',(0.786565919558984,-1.,-3.66680946938292));
#34528=CARTESIAN_POINT('Ctrl Pts',(0.786459983895431,-1.,-3.6666431041522));
#34529=CARTESIAN_POINT('Ctrl Pts',(0.786422660831985,-1.,-3.66661143271685));
#34530=CARTESIAN_POINT('',(0.963899035117249,-1.,-3.62400312501245));
#34531=CARTESIAN_POINT('Origin',(0.,-1.,0.));
#34532=CARTESIAN_POINT('',(1.22531898815164,-1.,-4.01728681790024));
#34533=CARTESIAN_POINT('Ctrl Pts',(0.963899035117249,-1.,-3.62400312501245));
#34534=CARTESIAN_POINT('Ctrl Pts',(0.963880158555582,-1.,-3.6240482887845));
#34535=CARTESIAN_POINT('Ctrl Pts',(0.963861297423241,-1.,-3.62424461507588));
#34536=CARTESIAN_POINT('Ctrl Pts',(0.963957782642843,-1.,-3.62489305727662));
#34537=CARTESIAN_POINT('Ctrl Pts',(0.964373850166457,-1.,-3.62652618145335));
#34538=CARTESIAN_POINT('Ctrl Pts',(0.965395153165293,-1.,-3.62988252139846));
#34539=CARTESIAN_POINT('Ctrl Pts',(0.967052554541385,-1.,-3.63492122081143));
#34540=CARTESIAN_POINT('Ctrl Pts',(0.969195124675865,-1.,-3.64113946505766));
#34541=CARTESIAN_POINT('Ctrl Pts',(0.971722122061341,-1.,-3.64819756447455));
#34542=CARTESIAN_POINT('Ctrl Pts',(0.974519971354848,-1.,-3.65571576735126));
#34543=CARTESIAN_POINT('Ctrl Pts',(0.977478312751618,-1.,-3.66333049637475));
#34544=CARTESIAN_POINT('Ctrl Pts',(0.980505922458267,-1.,-3.67074983340361));
#34545=CARTESIAN_POINT('Ctrl Pts',(0.983550791470419,-1.,-3.67782408841715));
#34546=CARTESIAN_POINT('Ctrl Pts',(0.986602639863837,-1.,-3.68455317926068));
#34547=CARTESIAN_POINT('Ctrl Pts',(0.989676715398558,-1.,-3.69102682138847));
#34548=CARTESIAN_POINT('Ctrl Pts',(0.99280221833201,-1.,-3.69738123415662));
#34549=CARTESIAN_POINT('Ctrl Pts',(0.996009819772518,-1.,-3.70375282282138));
#34550=CARTESIAN_POINT('Ctrl Pts',(0.99931726075653,-1.,-3.71022439713938));
#34551=CARTESIAN_POINT('Ctrl Pts',(1.00272423396822,-1.,-3.71680667125119));
#34552=CARTESIAN_POINT('Ctrl Pts',(1.0062200073571,-1.,-3.72346803750596));
#34553=CARTESIAN_POINT('Ctrl Pts',(1.00978798539496,-1.,-3.73015276704426));
#34554=CARTESIAN_POINT('Ctrl Pts',(1.01341114319903,-1.,-3.73680245055734));
#34555=CARTESIAN_POINT('Ctrl Pts',(1.01707794311079,-1.,-3.74337942504959));
#34556=CARTESIAN_POINT('Ctrl Pts',(1.02078510487428,-1.,-3.74987777155834));
#34557=CARTESIAN_POINT('Ctrl Pts',(1.0245342944466,-1.,-3.75631037456194));
#34558=CARTESIAN_POINT('Ctrl Pts',(1.02833014458181,-1.,-3.76270122291232));
#34559=CARTESIAN_POINT('Ctrl Pts',(1.0321778660492,-1.,-3.76907609832522));
#34560=CARTESIAN_POINT('Ctrl Pts',(1.03608074678013,-1.,-3.77545283140445));
#34561=CARTESIAN_POINT('Ctrl Pts',(1.04003862055804,-1.,-3.78183535008192));
#34562=CARTESIAN_POINT('Ctrl Pts',(1.04404924374426,-1.,-3.78821910787195));
#34563=CARTESIAN_POINT('Ctrl Pts',(1.04810913267641,-1.,-3.79459440308793));
#34564=CARTESIAN_POINT('Ctrl Pts',(1.05221457990015,-1.,-3.80095039790678));
#34565=CARTESIAN_POINT('Ctrl Pts',(1.05636266918643,-1.,-3.80727913637784));
#34566=CARTESIAN_POINT('Ctrl Pts',(1.06055206187298,-1.,-3.81357866117485));
#34567=CARTESIAN_POINT('Ctrl Pts',(1.06478244038931,-1.,-3.81985083953012));
#34568=CARTESIAN_POINT('Ctrl Pts',(1.0690541318036,-1.,-3.82609989967278));
#34569=CARTESIAN_POINT('Ctrl Pts',(1.0733676663346,-1.,-3.83233071195145));
#34570=CARTESIAN_POINT('Ctrl Pts',(1.07772335353856,-1.,-3.83854714117486));
#34571=CARTESIAN_POINT('Ctrl Pts',(1.08212087917986,-1.,-3.84475048030615));
#34572=CARTESIAN_POINT('Ctrl Pts',(1.08655950846377,-1.,-3.85094025222691));
#34573=CARTESIAN_POINT('Ctrl Pts',(1.09103825516288,-1.,-3.85711487933911));
#34574=CARTESIAN_POINT('Ctrl Pts',(1.09555606505012,-1.,-3.86327241021242));
#34575=CARTESIAN_POINT('Ctrl Pts',(1.10011198761202,-1.,-3.86941120134872));
#34576=CARTESIAN_POINT('Ctrl Pts',(1.10470536603303,-1.,-3.87553067187566));
#34577=CARTESIAN_POINT('Ctrl Pts',(1.10933577224029,-1.,-3.88163105531791));
#34578=CARTESIAN_POINT('Ctrl Pts',(1.11400292434447,-1.,-3.88771308285229));
#34579=CARTESIAN_POINT('Ctrl Pts',(1.11870660794609,-1.,-3.89377768340362));
#34580=CARTESIAN_POINT('Ctrl Pts',(1.12344660099029,-1.,-3.89982569749978));
#34581=CARTESIAN_POINT('Ctrl Pts',(1.12822258281518,-1.,-3.90585753318622));
#34582=CARTESIAN_POINT('Ctrl Pts',(1.13303414693849,-1.,-3.91187321145495));
#34583=CARTESIAN_POINT('Ctrl Pts',(1.13788084225511,-1.,-3.91787251936688));
#34584=CARTESIAN_POINT('Ctrl Pts',(1.14276220561575,-1.,-3.92385513133937));
#34585=CARTESIAN_POINT('Ctrl Pts',(1.14767779451147,-1.,-3.92982073294334));
#34586=CARTESIAN_POINT('Ctrl Pts',(1.1526272271639,-1.,-3.9357691705651));
#34587=CARTESIAN_POINT('Ctrl Pts',(1.1576101834106,-1.,-3.94170046685542));
#34588=CARTESIAN_POINT('Ctrl Pts',(1.16262637999261,-1.,-3.9476147478092));
#34589=CARTESIAN_POINT('Ctrl Pts',(1.16767555244495,-1.,-3.95351219510062));
#34590=CARTESIAN_POINT('Ctrl Pts',(1.17275743590327,-1.,-3.95939299213164));
#34591=CARTESIAN_POINT('Ctrl Pts',(1.17787174135445,-1.,-3.96525726357682));
#34592=CARTESIAN_POINT('Ctrl Pts',(1.18301815039596,-1.,-3.9711050516465));
#34593=CARTESIAN_POINT('Ctrl Pts',(1.18819633715285,-1.,-3.97693634766926));
#34594=CARTESIAN_POINT('Ctrl Pts',(1.19340598349307,-1.,-3.98275111052015));
#34595=CARTESIAN_POINT('Ctrl Pts',(1.19864679609596,-1.,-3.98854928957287));
#34596=CARTESIAN_POINT('Ctrl Pts',(1.2039185237544,-1.,-3.99433084800649));
#34597=CARTESIAN_POINT('Ctrl Pts',(1.20922097030107,-1.,-4.00009577952534));
#34598=CARTESIAN_POINT('Ctrl Pts',(1.21455398918813,-1.,-4.00584409524937));
#34599=CARTESIAN_POINT('Ctrl Pts',(1.21884478244983,-1.,-4.01042947142681));
#34600=CARTESIAN_POINT('Ctrl Pts',(1.22207656456199,-1.,-4.01386104434674));
#34601=CARTESIAN_POINT('Ctrl Pts',(1.22423716681447,-1.,-4.0161454457032));
#34602=CARTESIAN_POINT('Ctrl Pts',(1.22531898815164,-1.,-4.01728681790024));
#34603=CARTESIAN_POINT('',(1.36999806084572,-1.,-3.97027773754922));
#34604=CARTESIAN_POINT('',(1.22531898815164,-1.,-4.01728681790024));
#34605=CARTESIAN_POINT('',(1.35032489087101,-1.,-3.4984457533445));
#34606=CARTESIAN_POINT('Ctrl Pts',(1.36999806084572,-1.,-3.97027773754922));
#34607=CARTESIAN_POINT('Ctrl Pts',(1.37020239094614,-1.,-3.9687184694131));
#34608=CARTESIAN_POINT('Ctrl Pts',(1.37060761745635,-1.,-3.96560037974645));
#34609=CARTESIAN_POINT('Ctrl Pts',(1.3712051561502,-1.,-3.96092458506535));
#34610=CARTESIAN_POINT('Ctrl Pts',(1.37198126432386,-1.,-3.95469287280914));
#34611=CARTESIAN_POINT('Ctrl Pts',(1.37291699202807,-1.,-3.94690771785133));
#34612=CARTESIAN_POINT('Ctrl Pts',(1.37381821967165,-1.,-3.93912709040818));
#34613=CARTESIAN_POINT('Ctrl Pts',(1.37468482215751,-1.,-3.93135106761844));
#34614=CARTESIAN_POINT('Ctrl Pts',(1.37551664448242,-1.,-3.92357976987672));
#34615=CARTESIAN_POINT('Ctrl Pts',(1.37631350505797,-1.,-3.91581337462644));
#34616=CARTESIAN_POINT('Ctrl Pts',(1.3770751963402,-1.,-3.90805209523486));
#34617=CARTESIAN_POINT('Ctrl Pts',(1.37780148512792,-1.,-3.90029615196727));
#34618=CARTESIAN_POINT('Ctrl Pts',(1.3784921128802,-1.,-3.89254574338496));
#34619=CARTESIAN_POINT('Ctrl Pts',(1.37914679719383,-1.,-3.88480102249278));
#34620=CARTESIAN_POINT('Ctrl Pts',(1.37976523097073,-1.,-3.87706205830532));
#34621=CARTESIAN_POINT('Ctrl Pts',(1.38034709213014,-1.,-3.86932885813068));
#34622=CARTESIAN_POINT('Ctrl Pts',(1.38089205992989,-1.,-3.86160143043959));
#34623=CARTESIAN_POINT('Ctrl Pts',(1.38139983115049,-1.,-3.85387983979481));
#34624=CARTESIAN_POINT('Ctrl Pts',(1.38187013346109,-1.,-3.84616425605764));
#34625=CARTESIAN_POINT('Ctrl Pts',(1.38230274828821,-1.,-3.83845502790746));
#34626=CARTESIAN_POINT('Ctrl Pts',(1.38269750245138,-1.,-3.8307526698229));
#34627=CARTESIAN_POINT('Ctrl Pts',(1.38305421262763,-1.,-3.82305771743829));
#34628=CARTESIAN_POINT('Ctrl Pts',(1.38337263902782,-1.,-3.81537060817811));
#34629=CARTESIAN_POINT('Ctrl Pts',(1.3836524404622,-1.,-3.80769156398411));
#34630=CARTESIAN_POINT('Ctrl Pts',(1.38389311766682,-1.,-3.80002044322111));
#34631=CARTESIAN_POINT('Ctrl Pts',(1.38409399694566,-1.,-3.79235669640841));
#34632=CARTESIAN_POINT('Ctrl Pts',(1.38425435883756,-1.,-3.78469969805082));
#34633=CARTESIAN_POINT('Ctrl Pts',(1.38437354551428,-1.,-3.77704902230418));
#34634=CARTESIAN_POINT('Ctrl Pts',(1.38445107339518,-1.,-3.76940473185779));
#34635=CARTESIAN_POINT('Ctrl Pts',(1.3844867525335,-1.,-3.76176768271367));
#34636=CARTESIAN_POINT('Ctrl Pts',(1.38448077997163,-1.,-3.7541397631875));
#34637=CARTESIAN_POINT('Ctrl Pts',(1.38443344984394,-1.,-3.74652317167876));
#34638=CARTESIAN_POINT('Ctrl Pts',(1.38434489156458,-1.,-3.73891976418104));
#34639=CARTESIAN_POINT('Ctrl Pts',(1.38421479111531,-1.,-3.73133035859282));
#34640=CARTESIAN_POINT('Ctrl Pts',(1.3840421342895,-1.,-3.72375409358803));
#34641=CARTESIAN_POINT('Ctrl Pts',(1.38382489984586,-1.,-3.7161876605181));
#34642=CARTESIAN_POINT('Ctrl Pts',(1.38356065402124,-1.,-3.70862680753347));
#34643=CARTESIAN_POINT('Ctrl Pts',(1.38324717612865,-1.,-3.701067921679));
#34644=CARTESIAN_POINT('Ctrl Pts',(1.3828831117165,-1.,-3.69350967899526));
#34645=CARTESIAN_POINT('Ctrl Pts',(1.38246852827182,-1.,-3.68595444983838));
#34646=CARTESIAN_POINT('Ctrl Pts',(1.3820057429062,-1.,-3.67841038482414));
#34647=CARTESIAN_POINT('Ctrl Pts',(1.38149812653868,-1.,-3.67088843112262));
#34648=CARTESIAN_POINT('Ctrl Pts',(1.38094856333552,-1.,-3.66339848520857));
#34649=CARTESIAN_POINT('Ctrl Pts',(1.38035791051212,-1.,-3.6559455440439));
#34650=CARTESIAN_POINT('Ctrl Pts',(1.37972372481603,-1.,-3.64852652756456));
#34651=CARTESIAN_POINT('Ctrl Pts',(1.37903818567359,-1.,-3.64112507791141));
#34652=CARTESIAN_POINT('Ctrl Pts',(1.37829035457339,-1.,-3.63371727442486));
#34653=CARTESIAN_POINT('Ctrl Pts',(1.37746987919881,-1.,-3.62628098665145));
#34654=CARTESIAN_POINT('Ctrl Pts',(1.37657053403107,-1.,-3.61880481160421));
#34655=CARTESIAN_POINT('Ctrl Pts',(1.37559314436634,-1.,-3.61129546591064));
#34656=CARTESIAN_POINT('Ctrl Pts',(1.37455051379623,-1.,-3.60379020123988));
#34657=CARTESIAN_POINT('Ctrl Pts',(1.37346320103157,-1.,-3.59634627869048));
#34658=CARTESIAN_POINT('Ctrl Pts',(1.37235053660976,-1.,-3.58901853846365));
#34659=CARTESIAN_POINT('Ctrl Pts',(1.37122241663062,-1.,-3.58183885982715));
#34660=CARTESIAN_POINT('Ctrl Pts',(1.37007229485659,-1.,-3.57479875549486));
#34661=CARTESIAN_POINT('Ctrl Pts',(1.36886584973389,-1.,-3.5678208030466));
#34662=CARTESIAN_POINT('Ctrl Pts',(1.36754771771233,-1.,-3.56077662028649));
#34663=CARTESIAN_POINT('Ctrl Pts',(1.3660614545677,-1.,-3.55353883995949));
#34664=CARTESIAN_POINT('Ctrl Pts',(1.36436666257597,-1.,-3.54602591832973));
#34665=CARTESIAN_POINT('Ctrl Pts',(1.36245507339307,-1.,-3.53824396424961));
#34666=CARTESIAN_POINT('Ctrl Pts',(1.36037259643734,-1.,-3.530344649616));
#34667=CARTESIAN_POINT('Ctrl Pts',(1.35821701528836,-1.,-3.52261776116748));
#34668=CARTESIAN_POINT('Ctrl Pts',(1.35611275237152,-1.,-3.51542230699556));
#34669=CARTESIAN_POINT('Ctrl Pts',(1.35419113575956,-1.,-3.50913227059999));
#34670=CARTESIAN_POINT('Ctrl Pts',(1.35257032843486,-1.,-3.50408168106261));
#34671=CARTESIAN_POINT('Ctrl Pts',(1.35142377279517,-1.,-3.5007660381649));
#34672=CARTESIAN_POINT('Ctrl Pts',(1.35080045218586,-1.,-3.49920025459723));
#34673=CARTESIAN_POINT('Ctrl Pts',(1.35049736560527,-1.,-3.49861894124827));
#34674=CARTESIAN_POINT('Ctrl Pts',(1.35036670892966,-1.,-3.49847119623846));
#34675=CARTESIAN_POINT('Ctrl Pts',(1.35032489087101,-1.,-3.4984457533445));
#34676=CARTESIAN_POINT('',(1.51895082866166,-1.,-3.42859860294378));
#34677=CARTESIAN_POINT('Origin',(0.,-1.,0.));
#34678=CARTESIAN_POINT('',(1.83867539237861,-1.,-3.77614523045147));
#34679=CARTESIAN_POINT('Ctrl Pts',(1.51895082866166,-1.,-3.42859860294378));
#34680=CARTESIAN_POINT('Ctrl Pts',(1.51893924967231,-1.,-3.42864616361967));
#34681=CARTESIAN_POINT('Ctrl Pts',(1.51895133295017,-1.,-3.42884302333978));
#34682=CARTESIAN_POINT('Ctrl Pts',(1.51914806898539,-1.,-3.42946838852728));
#34683=CARTESIAN_POINT('Ctrl Pts',(1.5198144909343,-1.,-3.43101631893491));
#34684=CARTESIAN_POINT('Ctrl Pts',(1.52134826724227,-1.,-3.43417156977749));
#34685=CARTESIAN_POINT('Ctrl Pts',(1.52377348950429,-1.,-3.43888895974182));
#34686=CARTESIAN_POINT('Ctrl Pts',(1.52686242875717,-1.,-3.44469547527));
#34687=CARTESIAN_POINT('Ctrl Pts',(1.530462444618,-1.,-3.45127136828667));
#34688=CARTESIAN_POINT('Ctrl Pts',(1.53440195378902,-1.,-3.45825932955273));
#34689=CARTESIAN_POINT('Ctrl Pts',(1.53851507915533,-1.,-3.46531752207222));
#34690=CARTESIAN_POINT('Ctrl Pts',(1.54266605398152,-1.,-3.47217189224576));
#34691=CARTESIAN_POINT('Ctrl Pts',(1.54678009290206,-1.,-3.47868272898599));
#34692=CARTESIAN_POINT('Ctrl Pts',(1.55084702970382,-1.,-3.48485155928414));
#34693=CARTESIAN_POINT('Ctrl Pts',(1.5548959590107,-1.,-3.49076460877317));
#34694=CARTESIAN_POINT('Ctrl Pts',(1.55897703097859,-1.,-3.49655185179623));
#34695=CARTESIAN_POINT('Ctrl Pts',(1.56314187758689,-1.,-3.50234321621607));
#34696=CARTESIAN_POINT('Ctrl Pts',(1.56742097575041,-1.,-3.50821771695427));
#34697=CARTESIAN_POINT('Ctrl Pts',(1.57181569799774,-1.,-3.51418598431733));
#34698=CARTESIAN_POINT('Ctrl Pts',(1.5763104998818,-1.,-3.52021847865961));
#34699=CARTESIAN_POINT('Ctrl Pts',(1.58088027227856,-1.,-3.52626275334899));
#34700=CARTESIAN_POINT('Ctrl Pts',(1.58549906268083,-1.,-3.53226378147068));
#34701=CARTESIAN_POINT('Ctrl Pts',(1.59014958368725,-1.,-3.53818616861045));
#34702=CARTESIAN_POINT('Ctrl Pts',(1.5948276694975,-1.,-3.544024581823));
#34703=CARTESIAN_POINT('Ctrl Pts',(1.59953698113444,-1.,-3.54979148634426));
#34704=CARTESIAN_POINT('Ctrl Pts',(1.60428584699848,-1.,-3.55550985096117));
#34705=CARTESIAN_POINT('Ctrl Pts',(1.60908344685459,-1.,-3.56120432482986));
#34706=CARTESIAN_POINT('Ctrl Pts',(1.61393581747522,-1.,-3.56689200468404));
#34707=CARTESIAN_POINT('Ctrl Pts',(1.61884340915412,-1.,-3.57257679609826));
#34708=CARTESIAN_POINT('Ctrl Pts',(1.62380329464851,-1.,-3.57825455954405));
#34709=CARTESIAN_POINT('Ctrl Pts',(1.62881051550748,-1.,-3.5839162577435));
#34710=CARTESIAN_POINT('Ctrl Pts',(1.63385971451259,-1.,-3.58955176627876));
#34711=CARTESIAN_POINT('Ctrl Pts',(1.63894676675349,-1.,-3.59515368334887));
#34712=CARTESIAN_POINT('Ctrl Pts',(1.6440700438558,-1.,-3.6007202851384));
#34713=CARTESIAN_POINT('Ctrl Pts',(1.64922952425833,-1.,-3.60625346556992));
#34714=CARTESIAN_POINT('Ctrl Pts',(1.65442619244327,-1.,-3.61175734965129));
#34715=CARTESIAN_POINT('Ctrl Pts',(1.65966133399186,-1.,-3.61723666482457));
#34716=CARTESIAN_POINT('Ctrl Pts',(1.66493585923853,-1.,-3.62269517989104));
#34717=CARTESIAN_POINT('Ctrl Pts',(1.67024966008037,-1.,-3.62813422105257));
#34718=CARTESIAN_POINT('Ctrl Pts',(1.67560193613145,-1.,-3.63355343201211));
#34719=CARTESIAN_POINT('Ctrl Pts',(1.68099146651577,-1.,-3.63895140887443));
#34720=CARTESIAN_POINT('Ctrl Pts',(1.68641690471455,-1.,-3.64432638915199));
#34721=CARTESIAN_POINT('Ctrl Pts',(1.691877054817,-1.,-3.64967689827393));
#34722=CARTESIAN_POINT('Ctrl Pts',(1.69737117722558,-1.,-3.65500246526798));
#34723=CARTESIAN_POINT('Ctrl Pts',(1.70289888566904,-1.,-3.6603033877491));
#34724=CARTESIAN_POINT('Ctrl Pts',(1.70846001610983,-1.,-3.6655804319893));
#34725=CARTESIAN_POINT('Ctrl Pts',(1.71405450210392,-1.,-3.67083454901629));
#34726=CARTESIAN_POINT('Ctrl Pts',(1.71968225581787,-1.,-3.67606660374665));
#34727=CARTESIAN_POINT('Ctrl Pts',(1.72534302437003,-1.,-3.68127704936472));
#34728=CARTESIAN_POINT('Ctrl Pts',(1.73103640956647,-1.,-3.68646597019188));
#34729=CARTESIAN_POINT('Ctrl Pts',(1.73676193254493,-1.,-3.69163322647906));
#34730=CARTESIAN_POINT('Ctrl Pts',(1.74251908492589,-1.,-3.6967785691046));
#34731=CARTESIAN_POINT('Ctrl Pts',(1.74830738046092,-1.,-3.70190175673422));
#34732=CARTESIAN_POINT('Ctrl Pts',(1.75412641804148,-1.,-3.70700269736876));
#34733=CARTESIAN_POINT('Ctrl Pts',(1.75997588499021,-1.,-3.71208146346455));
#34734=CARTESIAN_POINT('Ctrl Pts',(1.76585552124549,-1.,-3.71713822377676));
#34735=CARTESIAN_POINT('Ctrl Pts',(1.77176509401846,-1.,-3.72217319911429));
#34736=CARTESIAN_POINT('Ctrl Pts',(1.77770437039606,-1.,-3.72718661205504));
#34737=CARTESIAN_POINT('Ctrl Pts',(1.78367308442682,-1.,-3.73217863095022));
#34738=CARTESIAN_POINT('Ctrl Pts',(1.78967092823139,-1.,-3.73714934729962));
#34739=CARTESIAN_POINT('Ctrl Pts',(1.79569757859041,-1.,-3.74209880351667));
#34740=CARTESIAN_POINT('Ctrl Pts',(1.80175271485519,-1.,-3.74702700874954));
#34741=CARTESIAN_POINT('Ctrl Pts',(1.80783603939662,-1.,-3.75193395888069));
#34742=CARTESIAN_POINT('Ctrl Pts',(1.81394729834032,-1.,-3.75681965683995));
#34743=CARTESIAN_POINT('Ctrl Pts',(1.82008629694924,-1.,-3.76168412709652));
#34744=CARTESIAN_POINT('Ctrl Pts',(1.82625289221933,-1.,-3.76652740355856));
#34745=CARTESIAN_POINT('Ctrl Pts',(1.83120816956515,-1.,-3.77038509819777));
#34746=CARTESIAN_POINT('Ctrl Pts',(1.83493697935064,-1.,-3.77326886065484));
#34747=CARTESIAN_POINT('Ctrl Pts',(1.83742834010821,-1.,-3.77518714458232));
#34748=CARTESIAN_POINT('Ctrl Pts',(1.83867539237861,-1.,-3.77614523045147));
#34749=CARTESIAN_POINT('',(1.97421938526992,-1.,-3.70708211654725));
#34750=CARTESIAN_POINT('',(1.83867539237861,-1.,-3.77614523045147));
#34751=CARTESIAN_POINT('',(1.88097764062541,-1.,-3.24413672884902));
#34752=CARTESIAN_POINT('Ctrl Pts',(1.97421938526992,-1.,-3.70708211654725));
#34753=CARTESIAN_POINT('Ctrl Pts',(1.974177276451,-1.,-3.7055100813194));
#34754=CARTESIAN_POINT('Ctrl Pts',(1.97408973726149,-1.,-3.70236698911837));
#34755=CARTESIAN_POINT('Ctrl Pts',(1.97394846382288,-1.,-3.69765528558292));
#34756=CARTESIAN_POINT('Ctrl Pts',(1.97374016224397,-1.,-3.69137888597855));
#34757=CARTESIAN_POINT('Ctrl Pts',(1.9734465030363,-1.,-3.68354319913416));
#34758=CARTESIAN_POINT('Ctrl Pts',(1.97311947678035,-1.,-3.67571738106175));
#34759=CARTESIAN_POINT('Ctrl Pts',(1.9727589719863,-1.,-3.66790152751984));
#34760=CARTESIAN_POINT('Ctrl Pts',(1.97236485439317,-1.,-3.66009578166865));
#34761=CARTESIAN_POINT('Ctrl Pts',(1.97193697240645,-1.,-3.65230034717364));
#34762=CARTESIAN_POINT('Ctrl Pts',(1.97147515441539,-1.,-3.64451546724222));
#34763=CARTESIAN_POINT('Ctrl Pts',(1.97097920454698,-1.,-3.63674139590853));
#34764=CARTESIAN_POINT('Ctrl Pts',(1.97044889850518,-1.,-3.62897836973397));
#34765=CARTESIAN_POINT('Ctrl Pts',(1.96988398129888,-1.,-3.62122658401722));
#34766=CARTESIAN_POINT('Ctrl Pts',(1.96928416040712,-1.,-3.61348615496393));
#34767=CARTESIAN_POINT('Ctrl Pts',(1.96864911885775,-1.,-3.60575714017676));
#34768=CARTESIAN_POINT('Ctrl Pts',(1.96797854118257,-1.,-3.59803959819725));
#34769=CARTESIAN_POINT('Ctrl Pts',(1.96727213799507,-1.,-3.5903336402273));
#34770=CARTESIAN_POINT('Ctrl Pts',(1.9665296668894,-1.,-3.58263947663884));
#34771=CARTESIAN_POINT('Ctrl Pts',(1.96575096652857,-1.,-3.57495748601088));
#34772=CARTESIAN_POINT('Ctrl Pts',(1.96493594634643,-1.,-3.56728820357933));
#34773=CARTESIAN_POINT('Ctrl Pts',(1.96408450906868,-1.,-3.55963218706201));
#34774=CARTESIAN_POINT('Ctrl Pts',(1.96319648628667,-1.,-3.55198990600929));
#34775=CARTESIAN_POINT('Ctrl Pts',(1.96227157573058,-1.,-3.54436163300425));
#34776=CARTESIAN_POINT('Ctrl Pts',(1.96130926212661,-1.,-3.53674730625759));
#34777=CARTESIAN_POINT('Ctrl Pts',(1.96030879411534,-1.,-3.52914648844289));
#34778=CARTESIAN_POINT('Ctrl Pts',(1.95926936324436,-1.,-3.52155867431438));
#34779=CARTESIAN_POINT('Ctrl Pts',(1.95819025316768,-1.,-3.51398354617773));
#34780=CARTESIAN_POINT('Ctrl Pts',(1.95707099606513,-1.,-3.50642124159913));
#34781=CARTESIAN_POINT('Ctrl Pts',(1.9559115382367,-1.,-3.49887263575602));
#34782=CARTESIAN_POINT('Ctrl Pts',(1.95471236969653,-1.,-3.49133956289154));
#34783=CARTESIAN_POINT('Ctrl Pts',(1.95347412486316,-1.,-3.48382414832649));
#34784=CARTESIAN_POINT('Ctrl Pts',(1.95219722189878,-1.,-3.47632820495926));
#34785=CARTESIAN_POINT('Ctrl Pts',(1.95088147859876,-1.,-3.4688525897419));
#34786=CARTESIAN_POINT('Ctrl Pts',(1.94952575850196,-1.,-3.46139661060959));
#34787=CARTESIAN_POINT('Ctrl Pts',(1.94812754766524,-1.,-3.45395731584051));
#34788=CARTESIAN_POINT('Ctrl Pts',(1.94668377715332,-1.,-3.44653088665685));
#34789=CARTESIAN_POINT('Ctrl Pts',(1.94519168842883,-1.,-3.43911410197693));
#34790=CARTESIAN_POINT('Ctrl Pts',(1.94364973660285,-1.,-3.43170586602436));
#34791=CARTESIAN_POINT('Ctrl Pts',(1.94205835913692,-1.,-3.42430850941497));
#34792=CARTESIAN_POINT('Ctrl Pts',(1.94042111965237,-1.,-3.41692971994082));
#34793=CARTESIAN_POINT('Ctrl Pts',(1.93874306008132,-1.,-3.40957978266623));
#34794=CARTESIAN_POINT('Ctrl Pts',(1.93702857723089,-1.,-3.40226802104093));
#34795=CARTESIAN_POINT('Ctrl Pts',(1.93527929945982,-1.,-3.39499923640789));
#34796=CARTESIAN_POINT('Ctrl Pts',(1.93349233176794,-1.,-3.38777076883267));
#34797=CARTESIAN_POINT('Ctrl Pts',(1.93165739093292,-1.,-3.38056768525577));
#34798=CARTESIAN_POINT('Ctrl Pts',(1.92975993109897,-1.,-3.37336807068078));
#34799=CARTESIAN_POINT('Ctrl Pts',(1.92778626543803,-1.,-3.36615168657597));
#34800=CARTESIAN_POINT('Ctrl Pts',(1.92572846125763,-1.,-3.35890824422976));
#34801=CARTESIAN_POINT('Ctrl Pts',(1.92358838440518,-1.,-3.35164424847207));
#34802=CARTESIAN_POINT('Ctrl Pts',(1.92138450828378,-1.,-3.34439448941915));
#34803=CARTESIAN_POINT('Ctrl Pts',(1.91914609610173,-1.,-3.33721230709948));
#34804=CARTESIAN_POINT('Ctrl Pts',(1.91690081930297,-1.,-3.33014884257812));
#34805=CARTESIAN_POINT('Ctrl Pts',(1.91466343916612,-1.,-3.32323403454507));
#34806=CARTESIAN_POINT('Ctrl Pts',(1.91242616234459,-1.,-3.31646052426395));
#34807=CARTESIAN_POINT('Ctrl Pts',(1.91014297830502,-1.,-3.30975721158694));
#34808=CARTESIAN_POINT('Ctrl Pts',(1.90773912171424,-1.,-3.30300595568341));
#34809=CARTESIAN_POINT('Ctrl Pts',(1.9051389186417,-1.,-3.29608978722258));
#34810=CARTESIAN_POINT('Ctrl Pts',(1.9022897124757,-1.,-3.28893448600364));
#34811=CARTESIAN_POINT('Ctrl Pts',(1.89918429230424,-1.,-3.28154737912287));
#34812=CARTESIAN_POINT('Ctrl Pts',(1.89589172903662,-1.,-3.27407108932908));
#34813=CARTESIAN_POINT('Ctrl Pts',(1.89255393500769,-1.,-3.2667765388833));
#34814=CARTESIAN_POINT('Ctrl Pts',(1.88934996203508,-1.,-3.2599988519361));
#34815=CARTESIAN_POINT('Ctrl Pts',(1.88646802523372,-1.,-3.25408686339298));
#34816=CARTESIAN_POINT('Ctrl Pts',(1.88407708646435,-1.,-3.24935200512055));
#34817=CARTESIAN_POINT('Ctrl Pts',(1.88242596600422,-1.,-3.24625654410705));
#34818=CARTESIAN_POINT('Ctrl Pts',(1.88156537699118,-1.,-3.24480754675942));
#34819=CARTESIAN_POINT('Ctrl Pts',(1.88117508446657,-1.,-3.24428080352952));
#34820=CARTESIAN_POINT('Ctrl Pts',(1.88102292397987,-1.,-3.24415531671311));
#34821=CARTESIAN_POINT('Ctrl Pts',(1.88097764062541,-1.,-3.24413672884902));
#34822=CARTESIAN_POINT('',(2.03660101169564,-1.,-3.14877060440425));
#34823=CARTESIAN_POINT('Origin',(0.,-1.,0.));
#34824=CARTESIAN_POINT('',(2.40675750623143,-1.,-3.44202241512147));
#34825=CARTESIAN_POINT('Ctrl Pts',(2.03660101169564,-1.,-3.14877060440425));
#34826=CARTESIAN_POINT('Ctrl Pts',(2.03659701539175,-1.,-3.1488193908823));
#34827=CARTESIAN_POINT('Ctrl Pts',(2.03663974554941,-1.,-3.14901193669147));
#34828=CARTESIAN_POINT('Ctrl Pts',(2.03693188810614,-1.,-3.14959882629936));
#34829=CARTESIAN_POINT('Ctrl Pts',(2.03783225496023,-1.,-3.15102344775396));
#34830=CARTESIAN_POINT('Ctrl Pts',(2.03984073791432,-1.,-3.1538999167466));
#34831=CARTESIAN_POINT('Ctrl Pts',(2.04297406404132,-1.,-3.15817983946525));
#34832=CARTESIAN_POINT('Ctrl Pts',(2.0469333124766,-1.,-3.16343165059235));
#34833=CARTESIAN_POINT('Ctrl Pts',(2.05151770247452,-1.,-3.16936341689859));
#34834=CARTESIAN_POINT('Ctrl Pts',(2.05650186773279,-1.,-3.17564906975592));
#34835=CARTESIAN_POINT('Ctrl Pts',(2.06166849827143,-1.,-3.18197692964677));
#34836=CARTESIAN_POINT('Ctrl Pts',(2.06684062744065,-1.,-3.18809755562297));
#34837=CARTESIAN_POINT('Ctrl Pts',(2.07192253497765,-1.,-3.19388465568113));
#34838=CARTESIAN_POINT('Ctrl Pts',(2.0769044187063,-1.,-3.19934132835879));
#34839=CARTESIAN_POINT('Ctrl Pts',(2.08182850370816,-1.,-3.20454818630635));
#34840=CARTESIAN_POINT('Ctrl Pts',(2.08676465517435,-1.,-3.20962575845433));
#34841=CARTESIAN_POINT('Ctrl Pts',(2.0917841946046,-1.,-3.2146942960168));
#34842=CARTESIAN_POINT('Ctrl Pts',(2.09692958434933,-1.,-3.21982707347067));
#34843=CARTESIAN_POINT('Ctrl Pts',(2.10220384298533,-1.,-3.22503437553496));
#34844=CARTESIAN_POINT('Ctrl Pts',(2.1075869964248,-1.,-3.23028945793334));
#34845=CARTESIAN_POINT('Ctrl Pts',(2.11304604021784,-1.,-3.23554444767115));
#34846=CARTESIAN_POINT('Ctrl Pts',(2.11854673326972,-1.,-3.24074905517282));
#34847=CARTESIAN_POINT('Ctrl Pts',(2.12406646410943,-1.,-3.24587102613347));
#34848=CARTESIAN_POINT('Ctrl Pts',(2.1296002839681,-1.,-3.25090574493994));
#34849=CARTESIAN_POINT('Ctrl Pts',(2.13515375878786,-1.,-3.25586495065027));
#34850=CARTESIAN_POINT('Ctrl Pts',(2.14073870754257,-1.,-3.26077002641868));
#34851=CARTESIAN_POINT('Ctrl Pts',(2.14636805295663,-1.,-3.26564388189764));
#34852=CARTESIAN_POINT('Ctrl Pts',(2.15205043199818,-1.,-3.27050245897244));
#34853=CARTESIAN_POINT('Ctrl Pts',(2.15778690038359,-1.,-3.27534954469206));
#34854=CARTESIAN_POINT('Ctrl Pts',(2.16357391934434,-1.,-3.28018150841414));
#34855=CARTESIAN_POINT('Ctrl Pts',(2.16940517773459,-1.,-3.2849901997973));
#34856=CARTESIAN_POINT('Ctrl Pts',(2.17527380048422,-1.,-3.28976645712566));
#34857=CARTESIAN_POINT('Ctrl Pts',(2.18117455557062,-1.,-3.29450361500484));
#34858=CARTESIAN_POINT('Ctrl Pts',(2.18710556500325,-1.,-3.29920022557635));
#34859=CARTESIAN_POINT('Ctrl Pts',(2.19306710376112,-1.,-3.30385816281831));
#34860=CARTESIAN_POINT('Ctrl Pts',(2.19906078949924,-1.,-3.30848134694597));
#34861=CARTESIAN_POINT('Ctrl Pts',(2.20508863150608,-1.,-3.3130742460895));
#34862=CARTESIAN_POINT('Ctrl Pts',(2.21115211847872,-1.,-3.31764044024231));
#34863=CARTESIAN_POINT('Ctrl Pts',(2.21725135110889,-1.,-3.32218125618955));
#34864=CARTESIAN_POINT('Ctrl Pts',(2.22338548312758,-1.,-3.32669646722871));
#34865=CARTESIAN_POINT('Ctrl Pts',(2.22955308907221,-1.,-3.33118487773593));
#34866=CARTESIAN_POINT('Ctrl Pts',(2.23575256328809,-1.,-3.33564495756478));
#34867=CARTESIAN_POINT('Ctrl Pts',(2.24198249391437,-1.,-3.34007543738044));
#34868=CARTESIAN_POINT('Ctrl Pts',(2.24824207678287,-1.,-3.34447596770768));
#34869=CARTESIAN_POINT('Ctrl Pts',(2.25453097693524,-1.,-3.34884690292342));
#34870=CARTESIAN_POINT('Ctrl Pts',(2.26084915222484,-1.,-3.35318902552676));
#34871=CARTESIAN_POINT('Ctrl Pts',(2.26719668579921,-1.,-3.35750328523077));
#34872=CARTESIAN_POINT('Ctrl Pts',(2.27357362620902,-1.,-3.36179055004369));
#34873=CARTESIAN_POINT('Ctrl Pts',(2.27997979457968,-1.,-3.36605130712978));
#34874=CARTESIAN_POINT('Ctrl Pts',(2.28641481081045,-1.,-3.37028570206357));
#34875=CARTESIAN_POINT('Ctrl Pts',(2.2928781800731,-1.,-3.37449367172707));
#34876=CARTESIAN_POINT('Ctrl Pts',(2.29936936127588,-1.,-3.37867504959382));
#34877=CARTESIAN_POINT('Ctrl Pts',(2.30588783640389,-1.,-3.38282967336676));
#34878=CARTESIAN_POINT('Ctrl Pts',(2.31243319489505,-1.,-3.38695751492659));
#34879=CARTESIAN_POINT('Ctrl Pts',(2.31900513925627,-1.,-3.39105869475112));
#34880=CARTESIAN_POINT('Ctrl Pts',(2.32560343902683,-1.,-3.39513342020045));
#34881=CARTESIAN_POINT('Ctrl Pts',(2.33222789882601,-1.,-3.39918194578115));
#34882=CARTESIAN_POINT('Ctrl Pts',(2.33887832342715,-1.,-3.40320452776646));
#34883=CARTESIAN_POINT('Ctrl Pts',(2.34555447648901,-1.,-3.40720137403888));
#34884=CARTESIAN_POINT('Ctrl Pts',(2.35225606823649,-1.,-3.41117262313464));
#34885=CARTESIAN_POINT('Ctrl Pts',(2.35898278606449,-1.,-3.4151183675076));
#34886=CARTESIAN_POINT('Ctrl Pts',(2.36573431470313,-1.,-3.41903866635384));
#34887=CARTESIAN_POINT('Ctrl Pts',(2.37251035954351,-1.,-3.42293356216595));
#34888=CARTESIAN_POINT('Ctrl Pts',(2.37931067029517,-1.,-3.42680309755241));
#34889=CARTESIAN_POINT('Ctrl Pts',(2.38613505844641,-1.,-3.43064732714472));
#34890=CARTESIAN_POINT('Ctrl Pts',(2.39298338805823,-1.,-3.43446630680436));
#34891=CARTESIAN_POINT('Ctrl Pts',(2.39848113411428,-1.,-3.43750133066037));
#34892=CARTESIAN_POINT('Ctrl Pts',(2.40261515590099,-1.,-3.43976627485223));
#34893=CARTESIAN_POINT('Ctrl Pts',(2.40537592959345,-1.,-3.44127120683402));
#34894=CARTESIAN_POINT('Ctrl Pts',(2.40675750623143,-1.,-3.44202241512147));
#34895=CARTESIAN_POINT('',(2.52982887637028,-1.,-3.35260583073571));
#34896=CARTESIAN_POINT('',(2.40675750623143,-1.,-3.44202241512147));
#34897=CARTESIAN_POINT('',(2.36531447826073,-1.,-2.90994629141676));
#34898=CARTESIAN_POINT('Ctrl Pts',(2.52982887637028,-1.,-3.35260583073571));
#34899=CARTESIAN_POINT('Ctrl Pts',(2.5295413654909,-1.,-3.35105973714072));
#34900=CARTESIAN_POINT('Ctrl Pts',(2.52896321610703,-1.,-3.34796903576663));
#34901=CARTESIAN_POINT('Ctrl Pts',(2.52808660915689,-1.,-3.34333744115511));
#34902=CARTESIAN_POINT('Ctrl Pts',(2.52689902690158,-1.,-3.33717089999103));
#34903=CARTESIAN_POINT('Ctrl Pts',(2.52538321164634,-1.,-3.32947762187533));
#34904=CARTESIAN_POINT('Ctrl Pts',(2.5238359839626,-1.,-3.32179931078699));
#34905=CARTESIAN_POINT('Ctrl Pts',(2.52225724871313,-1.,-3.31413607874645));
#34906=CARTESIAN_POINT('Ctrl Pts',(2.52064689568511,-1.,-3.30648808815443));
#34907=CARTESIAN_POINT('Ctrl Pts',(2.51900480701068,-1.,-3.29885556388353));
#34908=CARTESIAN_POINT('Ctrl Pts',(2.51733085123797,-1.,-3.2912387729927));
#34909=CARTESIAN_POINT('Ctrl Pts',(2.51562487464514,-1.,-3.28363799702982));
#34910=CARTESIAN_POINT('Ctrl Pts',(2.513886692704,-1.,-3.27605350473142));
#34911=CARTESIAN_POINT('Ctrl Pts',(2.51211608411423,-1.,-3.26848552888116));
#34912=CARTESIAN_POINT('Ctrl Pts',(2.51031277813486,-1.,-3.26093423001434));
#34913=CARTESIAN_POINT('Ctrl Pts',(2.50847647070723,-1.,-3.25339971460982));
#34914=CARTESIAN_POINT('Ctrl Pts',(2.506606859405,-1.,-3.24588208983849));
#34915=CARTESIAN_POINT('Ctrl Pts',(2.5047036758003,-1.,-3.23838151080319));
#34916=CARTESIAN_POINT('Ctrl Pts',(2.50276671338111,-1.,-3.23089822320646));
#34917=CARTESIAN_POINT('Ctrl Pts',(2.50079587201957,-1.,-3.22343262620503));
#34918=CARTESIAN_POINT('Ctrl Pts',(2.4987911459939,-1.,-3.21598526261286));
#34919=CARTESIAN_POINT('Ctrl Pts',(2.4967525264737,-1.,-3.20855669849836));
#34920=CARTESIAN_POINT('Ctrl Pts',(2.49467992057755,-1.,-3.20114742397588));
#34921=CARTESIAN_POINT('Ctrl Pts',(2.49257307239848,-1.,-3.19375775555798));
#34922=CARTESIAN_POINT('Ctrl Pts',(2.49043146334059,-1.,-3.18638771282266));
#34923=CARTESIAN_POINT('Ctrl Pts',(2.48825428288201,-1.,-3.17903698136622));
#34924=CARTESIAN_POINT('Ctrl Pts',(2.48604065348587,-1.,-3.17170518863313));
#34925=CARTESIAN_POINT('Ctrl Pts',(2.48378981792725,-1.,-3.16439213290161));
#34926=CARTESIAN_POINT('Ctrl Pts',(2.48150133566571,-1.,-3.15709802322739));
#34927=CARTESIAN_POINT('Ctrl Pts',(2.47917529057029,-1.,-3.14982373241352));
#34928=CARTESIAN_POINT('Ctrl Pts',(2.47681245356109,-1.,-3.1425709954655));
#34929=CARTESIAN_POINT('Ctrl Pts',(2.47441378371932,-1.,-3.13534181229295));
#34930=CARTESIAN_POINT('Ctrl Pts',(2.47197997765871,-1.,-3.12813790805952));
#34931=CARTESIAN_POINT('Ctrl Pts',(2.46951098947469,-1.,-3.12096015766983));
#34932=CARTESIAN_POINT('Ctrl Pts',(2.46700558843506,-1.,-3.11380805536122));
#34933=CARTESIAN_POINT('Ctrl Pts',(2.46446082979646,-1.,-3.1066790790198));
#34934=CARTESIAN_POINT('Ctrl Pts',(2.46187308501884,-1.,-3.09956993697052));
#34935=CARTESIAN_POINT('Ctrl Pts',(2.4592391256388,-1.,-3.09247787931887));
#34936=CARTESIAN_POINT('Ctrl Pts',(2.45655725437039,-1.,-3.08540206545315));
#34937=CARTESIAN_POINT('Ctrl Pts',(2.4538282678779,-1.,-3.07834472886139));
#34938=CARTESIAN_POINT('Ctrl Pts',(2.45105688854422,-1.,-3.07131290521297));
#34939=CARTESIAN_POINT('Ctrl Pts',(2.44824970516543,-1.,-3.06431596421405));
#34940=CARTESIAN_POINT('Ctrl Pts',(2.44541251892556,-1.,-3.05736242671506));
#34941=CARTESIAN_POINT('Ctrl Pts',(2.44254768923105,-1.,-3.05045678021504));
#34942=CARTESIAN_POINT('Ctrl Pts',(2.43965194061857,-1.,-3.04359685040555));
#34943=CARTESIAN_POINT('Ctrl Pts',(2.43671278042414,-1.,-3.03676949672822));
#34944=CARTESIAN_POINT('Ctrl Pts',(2.43371241361488,-1.,-3.02995534946978));
#34945=CARTESIAN_POINT('Ctrl Pts',(2.43063415586637,-1.,-3.02313656036004));
#34946=CARTESIAN_POINT('Ctrl Pts',(2.42746856264168,-1.,-3.01630420830504));
#34947=CARTESIAN_POINT('Ctrl Pts',(2.42421849439613,-1.,-3.00946442616659));
#34948=CARTESIAN_POINT('Ctrl Pts',(2.42090763946779,-1.,-3.00264868585996));
#34949=CARTESIAN_POINT('Ctrl Pts',(2.41757324500514,-1.,-2.99590509293503));
#34950=CARTESIAN_POINT('Ctrl Pts',(2.41425064199586,-1.,-2.98927983005796));
#34951=CARTESIAN_POINT('Ctrl Pts',(2.41095909342571,-1.,-2.98280015815107));
#34952=CARTESIAN_POINT('Ctrl Pts',(2.40768975073713,-1.,-2.97646002822422));
#34953=CARTESIAN_POINT('Ctrl Pts',(2.40438604734919,-1.,-2.9701964131236));
#34954=CARTESIAN_POINT('Ctrl Pts',(2.4009556571164,-1.,-2.96390432240312));
#34955=CARTESIAN_POINT('Ctrl Pts',(2.39730553974516,-1.,-2.95748006482942));
#34956=CARTESIAN_POINT('Ctrl Pts',(2.39337207631667,-1.,-2.95085857128439));
#34957=CARTESIAN_POINT('Ctrl Pts',(2.38914929090759,-1.,-2.94404820669076));
#34958=CARTESIAN_POINT('Ctrl Pts',(2.38472771516311,-1.,-2.93717903280391));
#34959=CARTESIAN_POINT('Ctrl Pts',(2.38028989582073,-1.,-2.93049643640206));
#34960=CARTESIAN_POINT('Ctrl Pts',(2.3760651052403,-1.,-2.92430340582608));
#34961=CARTESIAN_POINT('Ctrl Pts',(2.37229381109821,-1.,-2.91891503791411));
#34962=CARTESIAN_POINT('Ctrl Pts',(2.36919161373173,-1.,-2.9146124988314));
#34963=CARTESIAN_POINT('Ctrl Pts',(2.36707658451664,-1.,-2.91181344022549));
#34964=CARTESIAN_POINT('Ctrl Pts',(2.36599991765749,-1.,-2.91051690822156));
#34965=CARTESIAN_POINT('Ctrl Pts',(2.36553202948613,-1.,-2.91005770527719));
#34966=CARTESIAN_POINT('Ctrl Pts',(2.36536211188453,-1.,-2.90995756655606));
#34967=CARTESIAN_POINT('Ctrl Pts',(2.36531447826073,-1.,-2.90994629141676));
#34968=CARTESIAN_POINT('',(2.50410331873042,-1.,-2.79140942341378));
#34969=CARTESIAN_POINT('Origin',(0.,-1.,0.));
#34970=CARTESIAN_POINT('',(2.91557726271063,-1.,-3.02314558451372));
#34971=CARTESIAN_POINT('Ctrl Pts',(2.50410331873042,-1.,-2.79140942341378));
#34972=CARTESIAN_POINT('Ctrl Pts',(2.50410700351426,-1.,-2.79145823440899));
#34973=CARTESIAN_POINT('Ctrl Pts',(2.50417932839343,-1.,-2.79164172519039));
#34974=CARTESIAN_POINT('Ctrl Pts',(2.50455968395235,-1.,-2.79217568804874));
#34975=CARTESIAN_POINT('Ctrl Pts',(2.50567182569153,-1.,-2.79344192164204));
#34976=CARTESIAN_POINT('Ctrl Pts',(2.50810555977564,-1.,-2.7959687805717));
#34977=CARTESIAN_POINT('Ctrl Pts',(2.51186983687947,-1.,-2.79970585014308));
#34978=CARTESIAN_POINT('Ctrl Pts',(2.51660190466067,-1.,-2.80427363984939));
#34979=CARTESIAN_POINT('Ctrl Pts',(2.52205778589922,-1.,-2.80941521967234));
#34980=CARTESIAN_POINT('Ctrl Pts',(2.52796388055457,-1.,-2.8148437904867));
#34981=CARTESIAN_POINT('Ctrl Pts',(2.53405679667463,-1.,-2.82028550483744));
#34982=CARTESIAN_POINT('Ctrl Pts',(2.54012272520141,-1.,-2.82552167649157));
#34983=CARTESIAN_POINT('Ctrl Pts',(2.54604736792542,-1.,-2.83044254225794));
#34984=CARTESIAN_POINT('Ctrl Pts',(2.55182152806964,-1.,-2.83505269592412));
#34985=CARTESIAN_POINT('Ctrl Pts',(2.55749952145165,-1.,-2.83942515220699));
#34986=CARTESIAN_POINT('Ctrl Pts',(2.56316920798489,-1.,-2.84366802680211));
#34987=CARTESIAN_POINT('Ctrl Pts',(2.56891984251743,-1.,-2.84788893329091));
#34988=CARTESIAN_POINT('Ctrl Pts',(2.57480482727128,-1.,-2.85215360144483));
#34989=CARTESIAN_POINT('Ctrl Pts',(2.58082875254407,-1.,-2.85647171715147));
#34990=CARTESIAN_POINT('Ctrl Pts',(2.5869677064356,-1.,-2.86081999003668));
#34991=CARTESIAN_POINT('Ctrl Pts',(2.59318160184921,-1.,-2.86515629953528));
#34992=CARTESIAN_POINT('Ctrl Pts',(2.59942875223202,-1.,-2.86943633170712));
#34993=CARTESIAN_POINT('Ctrl Pts',(2.6056817788128,-1.,-2.87363176656475));
#34994=CARTESIAN_POINT('Ctrl Pts',(2.61193507170928,-1.,-2.87773881947885));
#34995=CARTESIAN_POINT('Ctrl Pts',(2.61819596473087,-1.,-2.88176821427502));
#34996=CARTESIAN_POINT('Ctrl Pts',(2.62447947640253,-1.,-2.88573922195049));
#34997=CARTESIAN_POINT('Ctrl Pts',(2.63080195420771,-1.,-2.88967244854243));
#34998=CARTESIAN_POINT('Ctrl Pts',(2.63717442263944,-1.,-2.89358228854557));
#34999=CARTESIAN_POINT('Ctrl Pts',(2.64359851684146,-1.,-2.89747231723361));
#35000=CARTESIAN_POINT('Ctrl Pts',(2.65007017365576,-1.,-2.90133950224879));
#35001=CARTESIAN_POINT('Ctrl Pts',(2.65658188464287,-1.,-2.90517678087467));
#35002=CARTESIAN_POINT('Ctrl Pts',(2.66312542616808,-1.,-2.90897617968921));
#35003=CARTESIAN_POINT('Ctrl Pts',(2.66969458792627,-1.,-2.91273193382876));
#35004=CARTESIAN_POINT('Ctrl Pts',(2.67628728855309,-1.,-2.91644290704281));
#35005=CARTESIAN_POINT('Ctrl Pts',(2.68290409279689,-1.,-2.92011090722152));
#35006=CARTESIAN_POINT('Ctrl Pts',(2.68954721165342,-1.,-2.92373955325876));
#35007=CARTESIAN_POINT('Ctrl Pts',(2.69621932864302,-1.,-2.92733294395268));
#35008=CARTESIAN_POINT('Ctrl Pts',(2.70292247416881,-1.,-2.93089438233746));
#35009=CARTESIAN_POINT('Ctrl Pts',(2.70965695523776,-1.,-2.93442516311168));
#35010=CARTESIAN_POINT('Ctrl Pts',(2.71642190053575,-1.,-2.93792519474955));
#35011=CARTESIAN_POINT('Ctrl Pts',(2.72321571511322,-1.,-2.94139351933882));
#35012=CARTESIAN_POINT('Ctrl Pts',(2.73003657371613,-1.,-2.94482887675139));
#35013=CARTESIAN_POINT('Ctrl Pts',(2.73688288329825,-1.,-2.94823023414381));
#35014=CARTESIAN_POINT('Ctrl Pts',(2.7437537949221,-1.,-2.95159737214305));
#35015=CARTESIAN_POINT('Ctrl Pts',(2.75064903318996,-1.,-2.95493069316211));
#35016=CARTESIAN_POINT('Ctrl Pts',(2.75756867888393,-1.,-2.9582309766594));
#35017=CARTESIAN_POINT('Ctrl Pts',(2.76451296269571,-1.,-2.96149914764832));
#35018=CARTESIAN_POINT('Ctrl Pts',(2.77148206836464,-1.,-2.96473605585548));
#35019=CARTESIAN_POINT('Ctrl Pts',(2.77847589542767,-1.,-2.9679422104295));
#35020=CARTESIAN_POINT('Ctrl Pts',(2.78549409123657,-1.,-2.97111781461349));
#35021=CARTESIAN_POINT('Ctrl Pts',(2.79253615718147,-1.,-2.97426288347475));
#35022=CARTESIAN_POINT('Ctrl Pts',(2.79960153278186,-1.,-2.97737733718242));
#35023=CARTESIAN_POINT('Ctrl Pts',(2.80668968101162,-1.,-2.98046109647299));
#35024=CARTESIAN_POINT('Ctrl Pts',(2.81380019196454,-1.,-2.9835141977994));
#35025=CARTESIAN_POINT('Ctrl Pts',(2.82093279065704,-1.,-2.98653680669434));
#35026=CARTESIAN_POINT('Ctrl Pts',(2.82808728190402,-1.,-2.98952916401699));
#35027=CARTESIAN_POINT('Ctrl Pts',(2.83526351254383,-1.,-2.99249155170479));
#35028=CARTESIAN_POINT('Ctrl Pts',(2.84246132984334,-1.,-2.995424253416));
#35029=CARTESIAN_POINT('Ctrl Pts',(2.84968053289104,-1.,-2.99832751144566));
#35030=CARTESIAN_POINT('Ctrl Pts',(2.85692085715129,-1.,-3.0012015079552));
#35031=CARTESIAN_POINT('Ctrl Pts',(2.86418200833065,-1.,-3.00404638316245));
#35032=CARTESIAN_POINT('Ctrl Pts',(2.87146368430104,-1.,-3.00686224485374));
#35033=CARTESIAN_POINT('Ctrl Pts',(2.87876560072799,-1.,-3.0096491810855));
#35034=CARTESIAN_POINT('Ctrl Pts',(2.88608751706796,-1.,-3.01240727309568));
#35035=CARTESIAN_POINT('Ctrl Pts',(2.8934292556764,-1.,-3.01513660433291));
#35036=CARTESIAN_POINT('Ctrl Pts',(2.90079069102661,-1.,-3.01783725123646));
#35037=CARTESIAN_POINT('Ctrl Pts',(2.90669553303902,-1.,-3.01997487194926));
#35038=CARTESIAN_POINT('Ctrl Pts',(2.91113297349052,-1.,-3.02156522743299));
#35039=CARTESIAN_POINT('Ctrl Pts',(2.91409518070707,-1.,-3.02261975104912));
#35040=CARTESIAN_POINT('Ctrl Pts',(2.91557726271063,-1.,-3.02314558451372));
#35041=CARTESIAN_POINT('',(3.02314558451372,-1.,-2.91557726271063));
#35042=CARTESIAN_POINT('',(2.91557726271063,-1.,-3.02314558451372));
#35043=CARTESIAN_POINT('',(2.79140942341258,-1.,-2.50410331873176));
#35044=CARTESIAN_POINT('Ctrl Pts',(3.02314558451372,-1.,-2.91557726271063));
#35045=CARTESIAN_POINT('Ctrl Pts',(3.02261975104593,-1.,-2.91409518070399));
#35046=CARTESIAN_POINT('Ctrl Pts',(3.02156522742431,-1.,-2.91113297348212));
#35047=CARTESIAN_POINT('Ctrl Pts',(3.01997487193503,-1.,-2.90669553302526));
#35048=CARTESIAN_POINT('Ctrl Pts',(3.01783725121981,-1.,-2.9007906910105));
#35049=CARTESIAN_POINT('Ctrl Pts',(3.01513660431928,-1.,-2.89342925566321));
#35050=CARTESIAN_POINT('Ctrl Pts',(3.01240727308829,-1.,-2.8860875170608));
#35051=CARTESIAN_POINT('Ctrl Pts',(3.00964918108476,-1.,-2.87876560072727));
#35052=CARTESIAN_POINT('Ctrl Pts',(3.00686224485784,-1.,-2.87146368430502));
#35053=CARTESIAN_POINT('Ctrl Pts',(3.00404638316867,-1.,-2.86418200833667));
#35054=CARTESIAN_POINT('Ctrl Pts',(3.00120150796095,-1.,-2.85692085715686));
#35055=CARTESIAN_POINT('Ctrl Pts',(2.99832751144925,-1.,-2.84968053289451));
#35056=CARTESIAN_POINT('Ctrl Pts',(2.99542425341685,-1.,-2.84246132984415));
#35057=CARTESIAN_POINT('Ctrl Pts',(2.99249155170339,-1.,-2.83526351254248));
#35058=CARTESIAN_POINT('Ctrl Pts',(2.98952916401446,-1.,-2.82808728190157));
#35059=CARTESIAN_POINT('Ctrl Pts',(2.9865368066918,-1.,-2.82093279065457));
#35060=CARTESIAN_POINT('Ctrl Pts',(2.98351419779767,-1.,-2.81380019196286));
#35061=CARTESIAN_POINT('Ctrl Pts',(2.98046109647241,-1.,-2.80668968101106));
#35062=CARTESIAN_POINT('Ctrl Pts',(2.97737733718287,-1.,-2.7996015327823));
#35063=CARTESIAN_POINT('Ctrl Pts',(2.9742628834758,-1.,-2.79253615718248));
#35064=CARTESIAN_POINT('Ctrl Pts',(2.97111781461465,-1.,-2.78549409123769));
#35065=CARTESIAN_POINT('Ctrl Pts',(2.96794221043036,-1.,-2.7784758954285));
#35066=CARTESIAN_POINT('Ctrl Pts',(2.96473605585583,-1.,-2.77148206836498));
#35067=CARTESIAN_POINT('Ctrl Pts',(2.96149914764818,-1.,-2.76451296269557));
#35068=CARTESIAN_POINT('Ctrl Pts',(2.95823097665896,-1.,-2.7575686788835));
#35069=CARTESIAN_POINT('Ctrl Pts',(2.95493069316161,-1.,-2.75064903318947));
#35070=CARTESIAN_POINT('Ctrl Pts',(2.95159737214266,-1.,-2.74375379492172));
#35071=CARTESIAN_POINT('Ctrl Pts',(2.94823023414364,-1.,-2.73688288329808));
#35072=CARTESIAN_POINT('Ctrl Pts',(2.94482887675143,-1.,-2.73003657371617));
#35073=CARTESIAN_POINT('Ctrl Pts',(2.94139351933897,-1.,-2.72321571511337));
#35074=CARTESIAN_POINT('Ctrl Pts',(2.93792519474972,-1.,-2.71642190053592));
#35075=CARTESIAN_POINT('Ctrl Pts',(2.93442516311179,-1.,-2.70965695523787));
#35076=CARTESIAN_POINT('Ctrl Pts',(2.93089438233749,-1.,-2.70292247416885));
#35077=CARTESIAN_POINT('Ctrl Pts',(2.92733294395267,-1.,-2.69621932864301));
#35078=CARTESIAN_POINT('Ctrl Pts',(2.92373955325875,-1.,-2.68954721165339));
#35079=CARTESIAN_POINT('Ctrl Pts',(2.92011090722152,-1.,-2.68290409279688));
#35080=CARTESIAN_POINT('Ctrl Pts',(2.91644290704285,-1.,-2.67628728855312));
#35081=CARTESIAN_POINT('Ctrl Pts',(2.91273193382882,-1.,-2.66969458792631));
#35082=CARTESIAN_POINT('Ctrl Pts',(2.90897617968923,-1.,-2.6631254261681));
#35083=CARTESIAN_POINT('Ctrl Pts',(2.90517678087461,-1.,-2.65658188464282));
#35084=CARTESIAN_POINT('Ctrl Pts',(2.90133950224867,-1.,-2.65007017365564));
#35085=CARTESIAN_POINT('Ctrl Pts',(2.89747231723345,-1.,-2.64359851684131));
#35086=CARTESIAN_POINT('Ctrl Pts',(2.89358228854544,-1.,-2.63717442263932));
#35087=CARTESIAN_POINT('Ctrl Pts',(2.88967244854239,-1.,-2.63080195420767));
#35088=CARTESIAN_POINT('Ctrl Pts',(2.88573922195059,-1.,-2.62447947640262));
#35089=CARTESIAN_POINT('Ctrl Pts',(2.88176821427525,-1.,-2.61819596473108));
#35090=CARTESIAN_POINT('Ctrl Pts',(2.87773881947915,-1.,-2.61193507170955));
#35091=CARTESIAN_POINT('Ctrl Pts',(2.87363176656501,-1.,-2.60568177881303));
#35092=CARTESIAN_POINT('Ctrl Pts',(2.86943633170722,-1.,-2.5994287522321));
#35093=CARTESIAN_POINT('Ctrl Pts',(2.86515629953513,-1.,-2.59318160184908));
#35094=CARTESIAN_POINT('Ctrl Pts',(2.86081999003629,-1.,-2.58696770643524));
#35095=CARTESIAN_POINT('Ctrl Pts',(2.85647171715092,-1.,-2.58082875254357));
#35096=CARTESIAN_POINT('Ctrl Pts',(2.85215360144431,-1.,-2.57480482727081));
#35097=CARTESIAN_POINT('Ctrl Pts',(2.84788893329067,-1.,-2.56891984251721));
#35098=CARTESIAN_POINT('Ctrl Pts',(2.84366802680237,-1.,-2.56316920798513));
#35099=CARTESIAN_POINT('Ctrl Pts',(2.83942515220782,-1.,-2.55749952145241));
#35100=CARTESIAN_POINT('Ctrl Pts',(2.83505269592536,-1.,-2.55182152807077));
#35101=CARTESIAN_POINT('Ctrl Pts',(2.83044254225917,-1.,-2.54604736792655));
#35102=CARTESIAN_POINT('Ctrl Pts',(2.8255216764922,-1.,-2.54012272520199));
#35103=CARTESIAN_POINT('Ctrl Pts',(2.82028550483689,-1.,-2.53405679667412));
#35104=CARTESIAN_POINT('Ctrl Pts',(2.81484379048475,-1.,-2.52796388055278));
#35105=CARTESIAN_POINT('Ctrl Pts',(2.80941521966941,-1.,-2.52205778589653));
#35106=CARTESIAN_POINT('Ctrl Pts',(2.80427363984653,-1.,-2.51660190465805));
#35107=CARTESIAN_POINT('Ctrl Pts',(2.79970585014168,-1.,-2.51186983687818));
#35108=CARTESIAN_POINT('Ctrl Pts',(2.79596878057287,-1.,-2.50810555977671));
#35109=CARTESIAN_POINT('Ctrl Pts',(2.79344192164147,-1.,-2.50567182569081));
#35110=CARTESIAN_POINT('Ctrl Pts',(2.79217568804755,-1.,-2.50455968395146));
#35111=CARTESIAN_POINT('Ctrl Pts',(2.79164172518905,-1.,-2.50417932839313));
#35112=CARTESIAN_POINT('Ctrl Pts',(2.79145823440781,-1.,-2.50410700351493));
#35113=CARTESIAN_POINT('Ctrl Pts',(2.79140942341258,-1.,-2.50410331873176));
#35114=CARTESIAN_POINT('',(2.90994629141562,-1.,-2.36531447826213));
#35115=CARTESIAN_POINT('Origin',(0.,-1.,0.));
#35116=CARTESIAN_POINT('',(3.35260583073571,-1.,-2.52982887637028));
#35117=CARTESIAN_POINT('Ctrl Pts',(2.90994629141562,-1.,-2.36531447826213));
#35118=CARTESIAN_POINT('Ctrl Pts',(2.90995756655558,-1.,-2.3653621118858));
#35119=CARTESIAN_POINT('Ctrl Pts',(2.9100577052777,-1.,-2.36553202948741));
#35120=CARTESIAN_POINT('Ctrl Pts',(2.91051690822262,-1.,-2.36599991765853));
#35121=CARTESIAN_POINT('Ctrl Pts',(2.91181344022628,-1.,-2.36707658451709));
#35122=CARTESIAN_POINT('Ctrl Pts',(2.91461249883016,-1.,-2.36919161373074));
#35123=CARTESIAN_POINT('Ctrl Pts',(2.9189150379156,-1.,-2.37229381109939));
#35124=CARTESIAN_POINT('Ctrl Pts',(2.92430340582912,-1.,-2.37606510524271));
#35125=CARTESIAN_POINT('Ctrl Pts',(2.93049643640517,-1.,-2.3802898958232));
#35126=CARTESIAN_POINT('Ctrl Pts',(2.93717903280599,-1.,-2.38472771516476));
#35127=CARTESIAN_POINT('Ctrl Pts',(2.94404820669135,-1.,-2.38914929090806));
#35128=CARTESIAN_POINT('Ctrl Pts',(2.95085857128372,-1.,-2.39337207631613));
#35129=CARTESIAN_POINT('Ctrl Pts',(2.95748006482811,-1.,-2.39730553974412));
#35130=CARTESIAN_POINT('Ctrl Pts',(2.9639043224018,-1.,-2.40095565711535));
#35131=CARTESIAN_POINT('Ctrl Pts',(2.97019641312272,-1.,-2.40438604734848));
#35132=CARTESIAN_POINT('Ctrl Pts',(2.97646002822395,-1.,-2.40768975073691));
#35133=CARTESIAN_POINT('Ctrl Pts',(2.98280015815132,-1.,-2.41095909342591));
#35134=CARTESIAN_POINT('Ctrl Pts',(2.98927983005851,-1.,-2.4142506419963));
#35135=CARTESIAN_POINT('Ctrl Pts',(2.99590509293561,-1.,-2.4175732450056));
#35136=CARTESIAN_POINT('Ctrl Pts',(3.00264868586038,-1.,-2.42090763946812));
#35137=CARTESIAN_POINT('Ctrl Pts',(3.00946442616674,-1.,-2.42421849439625));
#35138=CARTESIAN_POINT('Ctrl Pts',(3.01630420830493,-1.,-2.4274685626416));
#35139=CARTESIAN_POINT('Ctrl Pts',(3.02313656035977,-1.,-2.43063415586615));
#35140=CARTESIAN_POINT('Ctrl Pts',(3.02995534946946,-1.,-2.43371241361462));
#35141=CARTESIAN_POINT('Ctrl Pts',(3.03676949672797,-1.,-2.43671278042394));
#35142=CARTESIAN_POINT('Ctrl Pts',(3.04359685040545,-1.,-2.43965194061849));
#35143=CARTESIAN_POINT('Ctrl Pts',(3.05045678021509,-1.,-2.44254768923109));
#35144=CARTESIAN_POINT('Ctrl Pts',(3.05736242671521,-1.,-2.44541251892568));
#35145=CARTESIAN_POINT('Ctrl Pts',(3.06431596421422,-1.,-2.44824970516558));
#35146=CARTESIAN_POINT('Ctrl Pts',(3.0713129052131,-1.,-2.45105688854432));
#35147=CARTESIAN_POINT('Ctrl Pts',(3.07834472886145,-1.,-2.45382826787795));
#35148=CARTESIAN_POINT('Ctrl Pts',(3.08540206545313,-1.,-2.45655725437037));
#35149=CARTESIAN_POINT('Ctrl Pts',(3.09247787931881,-1.,-2.45923912563875));
#35150=CARTESIAN_POINT('Ctrl Pts',(3.09956993697048,-1.,-2.4618730850188));
#35151=CARTESIAN_POINT('Ctrl Pts',(3.10667907901981,-1.,-2.46446082979645));
#35152=CARTESIAN_POINT('Ctrl Pts',(3.11380805536124,-1.,-2.46700558843507));
#35153=CARTESIAN_POINT('Ctrl Pts',(3.12096015766984,-1.,-2.4695109894747));
#35154=CARTESIAN_POINT('Ctrl Pts',(3.12813790805948,-1.,-2.47197997765868));
#35155=CARTESIAN_POINT('Ctrl Pts',(3.13534181229282,-1.,-2.47441378371923));
#35156=CARTESIAN_POINT('Ctrl Pts',(3.14257099546531,-1.,-2.47681245356095));
#35157=CARTESIAN_POINT('Ctrl Pts',(3.14982373241335,-1.,-2.47917529057016));
#35158=CARTESIAN_POINT('Ctrl Pts',(3.15709802322735,-1.,-2.48150133566568));
#35159=CARTESIAN_POINT('Ctrl Pts',(3.16439213290181,-1.,-2.48378981792739));
#35160=CARTESIAN_POINT('Ctrl Pts',(3.17170518863357,-1.,-2.48604065348619));
#35161=CARTESIAN_POINT('Ctrl Pts',(3.17903698136678,-1.,-2.48825428288243));
#35162=CARTESIAN_POINT('Ctrl Pts',(3.18638771282315,-1.,-2.49043146334095));
#35163=CARTESIAN_POINT('Ctrl Pts',(3.19375775555814,-1.,-2.4925730723986));
#35164=CARTESIAN_POINT('Ctrl Pts',(3.20114742397549,-1.,-2.49467992057726));
#35165=CARTESIAN_POINT('Ctrl Pts',(3.2085566984974,-1.,-2.49675252647298));
#35166=CARTESIAN_POINT('Ctrl Pts',(3.21598526261157,-1.,-2.49879114599293));
#35167=CARTESIAN_POINT('Ctrl Pts',(3.22343262620387,-1.,-2.5007958720187));
#35168=CARTESIAN_POINT('Ctrl Pts',(3.23089822320596,-1.,-2.50276671338074));
#35169=CARTESIAN_POINT('Ctrl Pts',(3.23838151080383,-1.,-2.50470367580078));
#35170=CARTESIAN_POINT('Ctrl Pts',(3.24588208984042,-1.,-2.50660685940645));
#35171=CARTESIAN_POINT('Ctrl Pts',(3.25339971461265,-1.,-2.50847647070936));
#35172=CARTESIAN_POINT('Ctrl Pts',(3.26093423001716,-1.,-2.51031277813697));
#35173=CARTESIAN_POINT('Ctrl Pts',(3.26848552888271,-1.,-2.51211608411539));
#35174=CARTESIAN_POINT('Ctrl Pts',(3.27605350473048,-1.,-2.51388669270329));
#35175=CARTESIAN_POINT('Ctrl Pts',(3.28363799702583,-1.,-2.51562487464215));
#35176=CARTESIAN_POINT('Ctrl Pts',(3.2912387729863,-1.,-2.51733085123316));
#35177=CARTESIAN_POINT('Ctrl Pts',(3.29885556387661,-1.,-2.51900480700548));
#35178=CARTESIAN_POINT('Ctrl Pts',(3.30648808814986,-1.,-2.52064689568167));
#35179=CARTESIAN_POINT('Ctrl Pts',(3.31413607874727,-1.,-2.52225724871375));
#35180=CARTESIAN_POINT('Ctrl Pts',(3.32179931079521,-1.,-2.52383598396878));
#35181=CARTESIAN_POINT('Ctrl Pts',(3.32947762189049,-1.,-2.52538321165774));
#35182=CARTESIAN_POINT('Ctrl Pts',(3.33717090000955,-1.,-2.52689902691551));
#35183=CARTESIAN_POINT('Ctrl Pts',(3.34333744117093,-1.,-2.52808660916879));
#35184=CARTESIAN_POINT('Ctrl Pts',(3.34796903577628,-1.,-2.5289632161143));
#35185=CARTESIAN_POINT('Ctrl Pts',(3.35105973714426,-1.,-2.52954136549357));
#35186=CARTESIAN_POINT('Ctrl Pts',(3.35260583073571,-1.,-2.52982887637028));
#35187=CARTESIAN_POINT('',(3.44202241512147,-1.,-2.40675750623143));
#35188=CARTESIAN_POINT('',(3.35260583073571,-1.,-2.52982887637028));
#35189=CARTESIAN_POINT('',(3.14877060440327,-1.,-2.03660101169714));
#35190=CARTESIAN_POINT('Ctrl Pts',(3.44202241512147,-1.,-2.40675750623143));
#35191=CARTESIAN_POINT('Ctrl Pts',(3.44127120683039,-1.,-2.4053759295909));
#35192=CARTESIAN_POINT('Ctrl Pts',(3.43976627484234,-1.,-2.40261515589405));
#35193=CARTESIAN_POINT('Ctrl Pts',(3.43750133064416,-1.,-2.39848113410292));
#35194=CARTESIAN_POINT('Ctrl Pts',(3.4344663067854,-1.,-2.39298338804493));
#35195=CARTESIAN_POINT('Ctrl Pts',(3.43064732712919,-1.,-2.38613505843552));
#35196=CARTESIAN_POINT('Ctrl Pts',(3.42680309754399,-1.,-2.37931067028926));
#35197=CARTESIAN_POINT('Ctrl Pts',(3.42293356216511,-1.,-2.37251035954292));
#35198=CARTESIAN_POINT('Ctrl Pts',(3.41903866635852,-1.,-2.36573431470642));
#35199=CARTESIAN_POINT('Ctrl Pts',(3.41511836751469,-1.,-2.35898278606946));
#35200=CARTESIAN_POINT('Ctrl Pts',(3.41117262314119,-1.,-2.35225606824109));
#35201=CARTESIAN_POINT('Ctrl Pts',(3.40720137404297,-1.,-2.34555447649188));
#35202=CARTESIAN_POINT('Ctrl Pts',(3.40320452776743,-1.,-2.33887832342782));
#35203=CARTESIAN_POINT('Ctrl Pts',(3.39918194577956,-1.,-2.33222789882489));
#35204=CARTESIAN_POINT('Ctrl Pts',(3.39513342019756,-1.,-2.3256034390248));
#35205=CARTESIAN_POINT('Ctrl Pts',(3.39105869474822,-1.,-2.31900513925424));
#35206=CARTESIAN_POINT('Ctrl Pts',(3.38695751492462,-1.,-2.31243319489367));
#35207=CARTESIAN_POINT('Ctrl Pts',(3.3828296733661,-1.,-2.30588783640343));
#35208=CARTESIAN_POINT('Ctrl Pts',(3.37867504959433,-1.,-2.29936936127624));
#35209=CARTESIAN_POINT('Ctrl Pts',(3.37449367172826,-1.,-2.29287818007393));
#35210=CARTESIAN_POINT('Ctrl Pts',(3.37028570206488,-1.,-2.28641481081137));
#35211=CARTESIAN_POINT('Ctrl Pts',(3.36605130713076,-1.,-2.27997979458037));
#35212=CARTESIAN_POINT('Ctrl Pts',(3.36179055004409,-1.,-2.2735736262093));
#35213=CARTESIAN_POINT('Ctrl Pts',(3.35750328523061,-1.,-2.2671966857991));
#35214=CARTESIAN_POINT('Ctrl Pts',(3.35318902552626,-1.,-2.26084915222449));
#35215=CARTESIAN_POINT('Ctrl Pts',(3.34884690292285,-1.,-2.25453097693483));
#35216=CARTESIAN_POINT('Ctrl Pts',(3.34447596770723,-1.,-2.24824207678256));
#35217=CARTESIAN_POINT('Ctrl Pts',(3.34007543738025,-1.,-2.24198249391422));
#35218=CARTESIAN_POINT('Ctrl Pts',(3.33564495756481,-1.,-2.23575256328812));
#35219=CARTESIAN_POINT('Ctrl Pts',(3.33118487773611,-1.,-2.22955308907233));
#35220=CARTESIAN_POINT('Ctrl Pts',(3.3266964672289,-1.,-2.22338548312772));
#35221=CARTESIAN_POINT('Ctrl Pts',(3.32218125618968,-1.,-2.21725135110898));
#35222=CARTESIAN_POINT('Ctrl Pts',(3.31764044024235,-1.,-2.21115211847875));
#35223=CARTESIAN_POINT('Ctrl Pts',(3.31307424608949,-1.,-2.20508863150607));
#35224=CARTESIAN_POINT('Ctrl Pts',(3.30848134694595,-1.,-2.19906078949923));
#35225=CARTESIAN_POINT('Ctrl Pts',(3.30385816281831,-1.,-2.19306710376111));
#35226=CARTESIAN_POINT('Ctrl Pts',(3.29920022557639,-1.,-2.18710556500327));
#35227=CARTESIAN_POINT('Ctrl Pts',(3.2945036150049,-1.,-2.18117455557065));
#35228=CARTESIAN_POINT('Ctrl Pts',(3.28976645712568,-1.,-2.17527380048423));
#35229=CARTESIAN_POINT('Ctrl Pts',(3.28499019979724,-1.,-2.16940517773455));
#35230=CARTESIAN_POINT('Ctrl Pts',(3.280181508414,-1.,-2.16357391934425));
#35231=CARTESIAN_POINT('Ctrl Pts',(3.27534954469187,-1.,-2.15778690038347));
#35232=CARTESIAN_POINT('Ctrl Pts',(3.27050245897228,-1.,-2.15205043199808));
#35233=CARTESIAN_POINT('Ctrl Pts',(3.26564388189759,-1.,-2.1463680529566));
#35234=CARTESIAN_POINT('Ctrl Pts',(3.26077002641879,-1.,-2.14073870754264));
#35235=CARTESIAN_POINT('Ctrl Pts',(3.25586495065054,-1.,-2.13515375878803));
#35236=CARTESIAN_POINT('Ctrl Pts',(3.25090574494028,-1.,-2.12960028396832));
#35237=CARTESIAN_POINT('Ctrl Pts',(3.24587102613376,-1.,-2.12406646410962));
#35238=CARTESIAN_POINT('Ctrl Pts',(3.24074905517293,-1.,-2.11854673326979));
#35239=CARTESIAN_POINT('Ctrl Pts',(3.23554444767099,-1.,-2.11304604021773));
#35240=CARTESIAN_POINT('Ctrl Pts',(3.23028945793289,-1.,-2.10758699642451));
#35241=CARTESIAN_POINT('Ctrl Pts',(3.22503437553434,-1.,-2.10220384298492));
#35242=CARTESIAN_POINT('Ctrl Pts',(3.21982707347009,-1.,-2.09692958434895));
#35243=CARTESIAN_POINT('Ctrl Pts',(3.21469429601654,-1.,-2.09178419460443));
#35244=CARTESIAN_POINT('Ctrl Pts',(3.20962575845463,-1.,-2.08676465517455));
#35245=CARTESIAN_POINT('Ctrl Pts',(3.2045481863073,-1.,-2.08182850370878));
#35246=CARTESIAN_POINT('Ctrl Pts',(3.19934132836019,-1.,-2.07690441870722));
#35247=CARTESIAN_POINT('Ctrl Pts',(3.19388465568252,-1.,-2.07192253497857));
#35248=CARTESIAN_POINT('Ctrl Pts',(3.18809755562368,-1.,-2.06684062744112));
#35249=CARTESIAN_POINT('Ctrl Pts',(3.18197692964614,-1.,-2.06166849827101));
#35250=CARTESIAN_POINT('Ctrl Pts',(3.17564906975371,-1.,-2.05650186773132));
#35251=CARTESIAN_POINT('Ctrl Pts',(3.16936341689527,-1.,-2.05151770247233));
#35252=CARTESIAN_POINT('Ctrl Pts',(3.16343165058912,-1.,-2.04693331247446));
#35253=CARTESIAN_POINT('Ctrl Pts',(3.15817983946367,-1.,-2.04297406404027));
#35254=CARTESIAN_POINT('Ctrl Pts',(3.15389991674792,-1.,-2.03984073791519));
#35255=CARTESIAN_POINT('Ctrl Pts',(3.15102344775328,-1.,-2.03783225495961));
#35256=CARTESIAN_POINT('Ctrl Pts',(3.14959882629805,-1.,-2.03693188810545));
#35257=CARTESIAN_POINT('Ctrl Pts',(3.1490119366901,-1.,-2.03663974554932));
#35258=CARTESIAN_POINT('Ctrl Pts',(3.14881939088124,-1.,-2.03659701539259));
#35259=CARTESIAN_POINT('Ctrl Pts',(3.14877060440327,-1.,-2.03660101169714));
#35260=CARTESIAN_POINT('',(3.24413672884812,-1.,-1.88097764062697));
#35261=CARTESIAN_POINT('Origin',(0.,-1.,0.));
#35262=CARTESIAN_POINT('',(3.70708211654725,-1.,-1.97421938526992));
#35263=CARTESIAN_POINT('Ctrl Pts',(3.24413672884812,-1.,-1.88097764062697));
#35264=CARTESIAN_POINT('Ctrl Pts',(3.24415531671284,-1.,-1.8810229239812));
#35265=CARTESIAN_POINT('Ctrl Pts',(3.24428080353022,-1.,-1.88117508446775));
#35266=CARTESIAN_POINT('Ctrl Pts',(3.24480754676064,-1.,-1.88156537699203));
#35267=CARTESIAN_POINT('Ctrl Pts',(3.2462565441079,-1.,-1.88242596600454));
#35268=CARTESIAN_POINT('Ctrl Pts',(3.24935200511918,-1.,-1.88407708646357));
#35269=CARTESIAN_POINT('Ctrl Pts',(3.25408686339463,-1.,-1.88646802523466));
#35270=CARTESIAN_POINT('Ctrl Pts',(3.25999885193947,-1.,-1.88934996203698));
#35271=CARTESIAN_POINT('Ctrl Pts',(3.26677653888676,-1.,-1.89255393500965));
#35272=CARTESIAN_POINT('Ctrl Pts',(3.27407108933139,-1.,-1.89589172903793));
#35273=CARTESIAN_POINT('Ctrl Pts',(3.28154737912352,-1.,-1.89918429230462));
#35274=CARTESIAN_POINT('Ctrl Pts',(3.2889344860029,-1.,-1.90228971247527));
#35275=CARTESIAN_POINT('Ctrl Pts',(3.29608978722113,-1.,-1.90513891864087));
#35276=CARTESIAN_POINT('Ctrl Pts',(3.30300595568195,-1.,-1.90773912171341));
#35277=CARTESIAN_POINT('Ctrl Pts',(3.30975721158596,-1.,-1.91014297830446));
#35278=CARTESIAN_POINT('Ctrl Pts',(3.31646052426364,-1.,-1.91242616234442));
#35279=CARTESIAN_POINT('Ctrl Pts',(3.32323403454535,-1.,-1.91466343916628));
#35280=CARTESIAN_POINT('Ctrl Pts',(3.33014884257873,-1.,-1.91690081930332));
#35281=CARTESIAN_POINT('Ctrl Pts',(3.33721230710012,-1.,-1.9191460961021));
#35282=CARTESIAN_POINT('Ctrl Pts',(3.34439448941961,-1.,-1.92138450828404));
#35283=CARTESIAN_POINT('Ctrl Pts',(3.35164424847223,-1.,-1.92358838440528));
#35284=CARTESIAN_POINT('Ctrl Pts',(3.35890824422965,-1.,-1.92572846125756));
#35285=CARTESIAN_POINT('Ctrl Pts',(3.36615168657567,-1.,-1.92778626543786));
#35286=CARTESIAN_POINT('Ctrl Pts',(3.37336807068043,-1.,-1.92975993109877));
#35287=CARTESIAN_POINT('Ctrl Pts',(3.3805676852555,-1.,-1.93165739093276));
#35288=CARTESIAN_POINT('Ctrl Pts',(3.38777076883256,-1.,-1.93349233176788));
#35289=CARTESIAN_POINT('Ctrl Pts',(3.39499923640795,-1.,-1.93527929945985));
#35290=CARTESIAN_POINT('Ctrl Pts',(3.40226802104109,-1.,-1.93702857723098));
#35291=CARTESIAN_POINT('Ctrl Pts',(3.40957978266642,-1.,-1.93874306008143));
#35292=CARTESIAN_POINT('Ctrl Pts',(3.41692971994096,-1.,-1.94042111965246));
#35293=CARTESIAN_POINT('Ctrl Pts',(3.42430850941503,-1.,-1.94205835913696));
#35294=CARTESIAN_POINT('Ctrl Pts',(3.43170586602434,-1.,-1.94364973660284));
#35295=CARTESIAN_POINT('Ctrl Pts',(3.43911410197687,-1.,-1.94519168842879));
#35296=CARTESIAN_POINT('Ctrl Pts',(3.44653088665681,-1.,-1.94668377715329));
#35297=CARTESIAN_POINT('Ctrl Pts',(3.45395731584051,-1.,-1.94812754766524));
#35298=CARTESIAN_POINT('Ctrl Pts',(3.46139661060962,-1.,-1.94952575850197));
#35299=CARTESIAN_POINT('Ctrl Pts',(3.46885258974191,-1.,-1.95088147859877));
#35300=CARTESIAN_POINT('Ctrl Pts',(3.47632820495921,-1.,-1.95219722189876));
#35301=CARTESIAN_POINT('Ctrl Pts',(3.48382414832634,-1.,-1.95347412486309));
#35302=CARTESIAN_POINT('Ctrl Pts',(3.49133956289133,-1.,-1.95471236969643));
#35303=CARTESIAN_POINT('Ctrl Pts',(3.49887263575583,-1.,-1.95591153823661));
#35304=CARTESIAN_POINT('Ctrl Pts',(3.50642124159909,-1.,-1.95707099606511));
#35305=CARTESIAN_POINT('Ctrl Pts',(3.51398354617794,-1.,-1.95819025316779));
#35306=CARTESIAN_POINT('Ctrl Pts',(3.52155867431486,-1.,-1.95926936324461));
#35307=CARTESIAN_POINT('Ctrl Pts',(3.52914648844351,-1.,-1.96030879411566));
#35308=CARTESIAN_POINT('Ctrl Pts',(3.53674730625813,-1.,-1.96130926212689));
#35309=CARTESIAN_POINT('Ctrl Pts',(3.54436163300443,-1.,-1.96227157573067));
#35310=CARTESIAN_POINT('Ctrl Pts',(3.55198990600886,-1.,-1.96319648628644));
#35311=CARTESIAN_POINT('Ctrl Pts',(3.55963218706096,-1.,-1.96408450906812));
#35312=CARTESIAN_POINT('Ctrl Pts',(3.56728820357791,-1.,-1.96493594634567));
#35313=CARTESIAN_POINT('Ctrl Pts',(3.57495748600959,-1.,-1.96575096652789));
#35314=CARTESIAN_POINT('Ctrl Pts',(3.58263947663829,-1.,-1.96652966688911));
#35315=CARTESIAN_POINT('Ctrl Pts',(3.59033364022801,-1.,-1.96727213799544));
#35316=CARTESIAN_POINT('Ctrl Pts',(3.59803959819938,-1.,-1.96797854118369));
#35317=CARTESIAN_POINT('Ctrl Pts',(3.60575714017989,-1.,-1.9686491188594));
#35318=CARTESIAN_POINT('Ctrl Pts',(3.61348615496704,-1.,-1.96928416040877));
#35319=CARTESIAN_POINT('Ctrl Pts',(3.62122658401893,-1.,-1.96988398129978));
#35320=CARTESIAN_POINT('Ctrl Pts',(3.62897836973293,-1.,-1.97044889850463));
#35321=CARTESIAN_POINT('Ctrl Pts',(3.63674139590412,-1.,-1.97097920454464));
#35322=CARTESIAN_POINT('Ctrl Pts',(3.64451546723514,-1.,-1.97147515441164));
#35323=CARTESIAN_POINT('Ctrl Pts',(3.652300347166,-1.,-1.9719369724024));
#35324=CARTESIAN_POINT('Ctrl Pts',(3.6600957816636,-1.,-1.9723648543905));
#35325=CARTESIAN_POINT('Ctrl Pts',(3.66790152752075,-1.,-1.97275897198678));
#35326=CARTESIAN_POINT('Ctrl Pts',(3.67571738107084,-1.,-1.97311947678517));
#35327=CARTESIAN_POINT('Ctrl Pts',(3.68354319915092,-1.,-1.97344650304519));
#35328=CARTESIAN_POINT('Ctrl Pts',(3.69137888599902,-1.,-1.97374016225483));
#35329=CARTESIAN_POINT('Ctrl Pts',(3.6976552856004,-1.,-1.97394846383216));
#35330=CARTESIAN_POINT('Ctrl Pts',(3.70236698912904,-1.,-1.97408973726715));
#35331=CARTESIAN_POINT('Ctrl Pts',(3.70551008132332,-1.,-1.97417727645308));
#35332=CARTESIAN_POINT('Ctrl Pts',(3.70708211654725,-1.,-1.97421938526992));
#35333=CARTESIAN_POINT('',(3.77614523045147,-1.,-1.83867539237861));
#35334=CARTESIAN_POINT('',(3.70708211654725,-1.,-1.97421938526992));
#35335=CARTESIAN_POINT('',(3.42859860294305,-1.,-1.5189508286633));
#35336=CARTESIAN_POINT('Ctrl Pts',(3.77614523045147,-1.,-1.83867539237861));
#35337=CARTESIAN_POINT('Ctrl Pts',(3.77518714457833,-1.,-1.83742834010626));
#35338=CARTESIAN_POINT('Ctrl Pts',(3.77326886064398,-1.,-1.83493697934534));
#35339=CARTESIAN_POINT('Ctrl Pts',(3.77038509817999,-1.,-1.83120816955646));
#35340=CARTESIAN_POINT('Ctrl Pts',(3.76652740353775,-1.,-1.82625289220915));
#35341=CARTESIAN_POINT('Ctrl Pts',(3.76168412707948,-1.,-1.82008629694091));
#35342=CARTESIAN_POINT('Ctrl Pts',(3.75681965683071,-1.,-1.8139472983358));
#35343=CARTESIAN_POINT('Ctrl Pts',(3.75193395887977,-1.,-1.80783603939617));
#35344=CARTESIAN_POINT('Ctrl Pts',(3.74702700875467,-1.,-1.8017527148577));
#35345=CARTESIAN_POINT('Ctrl Pts',(3.74209880352445,-1.,-1.79569757859422));
#35346=CARTESIAN_POINT('Ctrl Pts',(3.73714934730681,-1.,-1.78967092823491));
#35347=CARTESIAN_POINT('Ctrl Pts',(3.7321786309547,-1.,-1.78367308442901));
#35348=CARTESIAN_POINT('Ctrl Pts',(3.72718661205609,-1.,-1.77770437039658));
#35349=CARTESIAN_POINT('Ctrl Pts',(3.72217319911254,-1.,-1.77176509401761));
#35350=CARTESIAN_POINT('Ctrl Pts',(3.71713822377359,-1.,-1.76585552124394));
#35351=CARTESIAN_POINT('Ctrl Pts',(3.71208146346136,-1.,-1.75997588498865));
#35352=CARTESIAN_POINT('Ctrl Pts',(3.70700269736659,-1.,-1.75412641804042));
#35353=CARTESIAN_POINT('Ctrl Pts',(3.7019017567335,-1.,-1.74830738046057));
#35354=CARTESIAN_POINT('Ctrl Pts',(3.69677856910517,-1.,-1.74251908492617));
#35355=CARTESIAN_POINT('Ctrl Pts',(3.69163322648036,-1.,-1.73676193254557));
#35356=CARTESIAN_POINT('Ctrl Pts',(3.68646597019332,-1.,-1.73103640956717));
#35357=CARTESIAN_POINT('Ctrl Pts',(3.68127704936579,-1.,-1.72534302437056));
#35358=CARTESIAN_POINT('Ctrl Pts',(3.67606660374709,-1.,-1.71968225581808));
#35359=CARTESIAN_POINT('Ctrl Pts',(3.67083454901611,-1.,-1.71405450210384));
#35360=CARTESIAN_POINT('Ctrl Pts',(3.66558043198876,-1.,-1.70846001610956));
#35361=CARTESIAN_POINT('Ctrl Pts',(3.66030338774847,-1.,-1.70289888566873));
#35362=CARTESIAN_POINT('Ctrl Pts',(3.65500246526749,-1.,-1.69737117722534));
#35363=CARTESIAN_POINT('Ctrl Pts',(3.64967689827371,-1.,-1.69187705481689));
#35364=CARTESIAN_POINT('Ctrl Pts',(3.64432638915203,-1.,-1.68641690471457));
#35365=CARTESIAN_POINT('Ctrl Pts',(3.63895140887462,-1.,-1.68099146651586));
#35366=CARTESIAN_POINT('Ctrl Pts',(3.63355343201232,-1.,-1.67560193613156));
#35367=CARTESIAN_POINT('Ctrl Pts',(3.62813422105271,-1.,-1.67024966008045));
#35368=CARTESIAN_POINT('Ctrl Pts',(3.62269517989109,-1.,-1.66493585923855));
#35369=CARTESIAN_POINT('Ctrl Pts',(3.61723666482456,-1.,-1.65966133399186));
#35370=CARTESIAN_POINT('Ctrl Pts',(3.61175734965127,-1.,-1.65442619244325));
#35371=CARTESIAN_POINT('Ctrl Pts',(3.60625346556992,-1.,-1.64922952425832));
#35372=CARTESIAN_POINT('Ctrl Pts',(3.60072028513845,-1.,-1.64407004385582));
#35373=CARTESIAN_POINT('Ctrl Pts',(3.59515368334893,-1.,-1.63894676675352));
#35374=CARTESIAN_POINT('Ctrl Pts',(3.58955176627879,-1.,-1.6338597145126));
#35375=CARTESIAN_POINT('Ctrl Pts',(3.58391625774343,-1.,-1.62881051550745));
#35376=CARTESIAN_POINT('Ctrl Pts',(3.5782545595439,-1.,-1.62380329464844));
#35377=CARTESIAN_POINT('Ctrl Pts',(3.57257679609806,-1.,-1.61884340915404));
#35378=CARTESIAN_POINT('Ctrl Pts',(3.56689200468387,-1.,-1.61393581747514));
#35379=CARTESIAN_POINT('Ctrl Pts',(3.5612043248298,-1.,-1.60908344685457));
#35380=CARTESIAN_POINT('Ctrl Pts',(3.55550985096129,-1.,-1.60428584699853));
#35381=CARTESIAN_POINT('Ctrl Pts',(3.54979148634454,-1.,-1.59953698113457));
#35382=CARTESIAN_POINT('Ctrl Pts',(3.54402458182337,-1.,-1.59482766949766));
#35383=CARTESIAN_POINT('Ctrl Pts',(3.53818616861077,-1.,-1.59014958368739));
#35384=CARTESIAN_POINT('Ctrl Pts',(3.5322637814708,-1.,-1.58549906268088));
#35385=CARTESIAN_POINT('Ctrl Pts',(3.52626275334881,-1.,-1.58088027227848));
#35386=CARTESIAN_POINT('Ctrl Pts',(3.52021847865912,-1.,-1.57631049988158));
#35387=CARTESIAN_POINT('Ctrl Pts',(3.51418598431665,-1.,-1.57181569799743));
#35388=CARTESIAN_POINT('Ctrl Pts',(3.50821771695363,-1.,-1.56742097575012));
#35389=CARTESIAN_POINT('Ctrl Pts',(3.50234321621578,-1.,-1.56314187758675));
#35390=CARTESIAN_POINT('Ctrl Pts',(3.49655185179655,-1.,-1.55897703097874));
#35391=CARTESIAN_POINT('Ctrl Pts',(3.4907646087742,-1.,-1.55489595901116));
#35392=CARTESIAN_POINT('Ctrl Pts',(3.48485155928567,-1.,-1.55084702970452));
#35393=CARTESIAN_POINT('Ctrl Pts',(3.47868272898751,-1.,-1.54678009290276));
#35394=CARTESIAN_POINT('Ctrl Pts',(3.47217189224653,-1.,-1.54266605398188));
#35395=CARTESIAN_POINT('Ctrl Pts',(3.46531752207153,-1.,-1.53851507915502));
#35396=CARTESIAN_POINT('Ctrl Pts',(3.45825932955032,-1.,-1.53440195378792));
#35397=CARTESIAN_POINT('Ctrl Pts',(3.45127136828305,-1.,-1.53046244461635));
#35398=CARTESIAN_POINT('Ctrl Pts',(3.44469547526647,-1.,-1.52686242875556));
#35399=CARTESIAN_POINT('Ctrl Pts',(3.4388889597401,-1.,-1.5237734895035));
#35400=CARTESIAN_POINT('Ctrl Pts',(3.43417156977893,-1.,-1.52134826724293));
#35401=CARTESIAN_POINT('Ctrl Pts',(3.43101631893414,-1.,-1.5198144909338));
#35402=CARTESIAN_POINT('Ctrl Pts',(3.42946838852587,-1.,-1.51914806898491));
#35403=CARTESIAN_POINT('Ctrl Pts',(3.42884302333841,-1.,-1.5189513329503));
#35404=CARTESIAN_POINT('Ctrl Pts',(3.42864616361875,-1.,-1.51893924967331));
#35405=CARTESIAN_POINT('Ctrl Pts',(3.42859860294305,-1.,-1.5189508286633));
#35406=CARTESIAN_POINT('',(3.49844575334386,-1.,-1.35032489087269));
#35407=CARTESIAN_POINT('Origin',(0.,-1.,0.));
#35408=CARTESIAN_POINT('',(3.97027773754922,-1.,-1.36999806084572));
#35409=CARTESIAN_POINT('Ctrl Pts',(3.49844575334386,-1.,-1.35032489087269));
#35410=CARTESIAN_POINT('Ctrl Pts',(3.49847119623841,-1.,-1.35036670893102));
#35411=CARTESIAN_POINT('Ctrl Pts',(3.49861894124915,-1.,-1.35049736560633));
#35412=CARTESIAN_POINT('Ctrl Pts',(3.49920025459856,-1.,-1.35080045218652));
#35413=CARTESIAN_POINT('Ctrl Pts',(3.5007660381658,-1.,-1.35142377279535));
#35414=CARTESIAN_POINT('Ctrl Pts',(3.50408168106113,-1.,-1.3525703284343));
#35415=CARTESIAN_POINT('Ctrl Pts',(3.50913227060177,-1.,-1.35419113576022));
#35416=CARTESIAN_POINT('Ctrl Pts',(3.51542230699919,-1.,-1.35611275237288));
#35417=CARTESIAN_POINT('Ctrl Pts',(3.52261776117121,-1.,-1.35821701528975));
#35418=CARTESIAN_POINT('Ctrl Pts',(3.53034464961849,-1.,-1.36037259643827));
#35419=CARTESIAN_POINT('Ctrl Pts',(3.53824396425032,-1.,-1.36245507339334));
#35420=CARTESIAN_POINT('Ctrl Pts',(3.54602591832893,-1.,-1.36436666257568));
#35421=CARTESIAN_POINT('Ctrl Pts',(3.55353883995793,-1.,-1.36606145456711));
#35422=CARTESIAN_POINT('Ctrl Pts',(3.56077662028492,-1.,-1.36754771771174));
#35423=CARTESIAN_POINT('Ctrl Pts',(3.56782080304554,-1.,-1.36886584973349));
#35424=CARTESIAN_POINT('Ctrl Pts',(3.57479875549453,-1.,-1.37007229485646));
#35425=CARTESIAN_POINT('Ctrl Pts',(3.58183885982745,-1.,-1.37122241663073));
#35426=CARTESIAN_POINT('Ctrl Pts',(3.5890185384643,-1.,-1.37235053661));
#35427=CARTESIAN_POINT('Ctrl Pts',(3.59634627869117,-1.,-1.37346320103184));
#35428=CARTESIAN_POINT('Ctrl Pts',(3.60379020124038,-1.,-1.37455051379642));
#35429=CARTESIAN_POINT('Ctrl Pts',(3.61129546591082,-1.,-1.37559314436641));
#35430=CARTESIAN_POINT('Ctrl Pts',(3.61880481160408,-1.,-1.37657053403102));
#35431=CARTESIAN_POINT('Ctrl Pts',(3.62628098665112,-1.,-1.37746987919868));
#35432=CARTESIAN_POINT('Ctrl Pts',(3.63371727442448,-1.,-1.37829035457325));
#35433=CARTESIAN_POINT('Ctrl Pts',(3.64112507791112,-1.,-1.37903818567347));
#35434=CARTESIAN_POINT('Ctrl Pts',(3.64852652756444,-1.,-1.37972372481598));
#35435=CARTESIAN_POINT('Ctrl Pts',(3.65594554404396,-1.,-1.38035791051215));
#35436=CARTESIAN_POINT('Ctrl Pts',(3.66339848520874,-1.,-1.38094856333558));
#35437=CARTESIAN_POINT('Ctrl Pts',(3.67088843112282,-1.,-1.38149812653876));
#35438=CARTESIAN_POINT('Ctrl Pts',(3.6784103848243,-1.,-1.38200574290626));
#35439=CARTESIAN_POINT('Ctrl Pts',(3.68595444983844,-1.,-1.38246852827185));
#35440=CARTESIAN_POINT('Ctrl Pts',(3.69350967899523,-1.,-1.38288311171649));
#35441=CARTESIAN_POINT('Ctrl Pts',(3.70106792167894,-1.,-1.38324717612862));
#35442=CARTESIAN_POINT('Ctrl Pts',(3.70862680753343,-1.,-1.38356065402122));
#35443=CARTESIAN_POINT('Ctrl Pts',(3.7161876605181,-1.,-1.38382489984585));
#35444=CARTESIAN_POINT('Ctrl Pts',(3.72375409358805,-1.,-1.3840421342895));
#35445=CARTESIAN_POINT('Ctrl Pts',(3.73133035859283,-1.,-1.38421479111531));
#35446=CARTESIAN_POINT('Ctrl Pts',(3.73891976418099,-1.,-1.38434489156456));
#35447=CARTESIAN_POINT('Ctrl Pts',(3.7465231716786,-1.,-1.38443344984389));
#35448=CARTESIAN_POINT('Ctrl Pts',(3.75413976318727,-1.,-1.38448077997155));
#35449=CARTESIAN_POINT('Ctrl Pts',(3.76176768271347,-1.,-1.38448675253343));
#35450=CARTESIAN_POINT('Ctrl Pts',(3.76940473185775,-1.,-1.38445107339517));
#35451=CARTESIAN_POINT('Ctrl Pts',(3.77704902230441,-1.,-1.38437354551435));
#35452=CARTESIAN_POINT('Ctrl Pts',(3.78469969805134,-1.,-1.38425435883773));
#35453=CARTESIAN_POINT('Ctrl Pts',(3.79235669640907,-1.,-1.38409399694589));
#35454=CARTESIAN_POINT('Ctrl Pts',(3.80002044322169,-1.,-1.38389311766701));
#35455=CARTESIAN_POINT('Ctrl Pts',(3.80769156398429,-1.,-1.38365244046226));
#35456=CARTESIAN_POINT('Ctrl Pts',(3.81537060817765,-1.,-1.38337263902766));
#35457=CARTESIAN_POINT('Ctrl Pts',(3.82305771743715,-1.,-1.38305421262724));
#35458=CARTESIAN_POINT('Ctrl Pts',(3.83075266982138,-1.,-1.38269750245086));
#35459=CARTESIAN_POINT('Ctrl Pts',(3.83845502790609,-1.,-1.38230274828774));
#35460=CARTESIAN_POINT('Ctrl Pts',(3.84616425605705,-1.,-1.38187013346089));
#35461=CARTESIAN_POINT('Ctrl Pts',(3.85387983979557,-1.,-1.38139983115075));
#35462=CARTESIAN_POINT('Ctrl Pts',(3.86160143044187,-1.,-1.38089205993068));
#35463=CARTESIAN_POINT('Ctrl Pts',(3.86932885813403,-1.,-1.38034709213129));
#35464=CARTESIAN_POINT('Ctrl Pts',(3.87706205830865,-1.,-1.37976523097187));
#35465=CARTESIAN_POINT('Ctrl Pts',(3.88480102249461,-1.,-1.37914679719446));
#35466=CARTESIAN_POINT('Ctrl Pts',(3.89254574338385,-1.,-1.37849211287981));
#35467=CARTESIAN_POINT('Ctrl Pts',(3.90029615196255,-1.,-1.3778014851263));
#35468=CARTESIAN_POINT('Ctrl Pts',(3.90805209522729,-1.,-1.3770751963376));
#35469=CARTESIAN_POINT('Ctrl Pts',(3.91581337461825,-1.,-1.37631350505516));
#35470=CARTESIAN_POINT('Ctrl Pts',(3.92357976987132,-1.,-1.37551664448057));
#35471=CARTESIAN_POINT('Ctrl Pts',(3.93135106761941,-1.,-1.37468482215784));
#35472=CARTESIAN_POINT('Ctrl Pts',(3.93912709041791,-1.,-1.37381821967499));
#35473=CARTESIAN_POINT('Ctrl Pts',(3.94690771786926,-1.,-1.37291699203423));
#35474=CARTESIAN_POINT('Ctrl Pts',(3.95469287283105,-1.,-1.37198126433139));
#35475=CARTESIAN_POINT('Ctrl Pts',(3.96092458508407,-1.,-1.37120515615663));
#35476=CARTESIAN_POINT('Ctrl Pts',(3.96560037975788,-1.,-1.37060761746027));
#35477=CARTESIAN_POINT('Ctrl Pts',(3.9687184694173,-1.,-1.37020239094758));
#35478=CARTESIAN_POINT('Ctrl Pts',(3.97027773754922,-1.,-1.36999806084572));
#35479=CARTESIAN_POINT('',(4.01728681790024,-1.,-1.22531898815164));
#35480=CARTESIAN_POINT('',(3.97027773754922,-1.,-1.36999806084572));
#35481=CARTESIAN_POINT('',(3.62400312501199,-1.,-0.963899035118986));
#35482=CARTESIAN_POINT('Ctrl Pts',(4.01728681790024,-1.,-1.22531898815164));
#35483=CARTESIAN_POINT('Ctrl Pts',(4.01614544569895,-1.,-1.22423716681317));
#35484=CARTESIAN_POINT('Ctrl Pts',(4.01386104433519,-1.,-1.22207656455845));
#35485=CARTESIAN_POINT('Ctrl Pts',(4.01042947140789,-1.,-1.21884478244403));
#35486=CARTESIAN_POINT('Ctrl Pts',(4.00584409522722,-1.,-1.21455398918133));
#35487=CARTESIAN_POINT('Ctrl Pts',(4.00009577950721,-1.,-1.20922097029551));
#35488=CARTESIAN_POINT('Ctrl Pts',(3.99433084799666,-1.,-1.20391852375139));
#35489=CARTESIAN_POINT('Ctrl Pts',(3.98854928957189,-1.,-1.19864679609566));
#35490=CARTESIAN_POINT('Ctrl Pts',(3.98275111052561,-1.,-1.19340598349475));
#35491=CARTESIAN_POINT('Ctrl Pts',(3.97693634767754,-1.,-1.18819633715539));
#35492=CARTESIAN_POINT('Ctrl Pts',(3.97110505165415,-1.,-1.18301815039831));
#35493=CARTESIAN_POINT('Ctrl Pts',(3.96525726358159,-1.,-1.17787174135592));
#35494=CARTESIAN_POINT('Ctrl Pts',(3.95939299213276,-1.,-1.17275743590361));
#35495=CARTESIAN_POINT('Ctrl Pts',(3.95351219509876,-1.,-1.16767555244438));
#35496=CARTESIAN_POINT('Ctrl Pts',(3.94761474780583,-1.,-1.16262637999157));
#35497=CARTESIAN_POINT('Ctrl Pts',(3.94170046685203,-1.,-1.15761018340956));
#35498=CARTESIAN_POINT('Ctrl Pts',(3.9357691705628,-1.,-1.1526272271632));
#35499=CARTESIAN_POINT('Ctrl Pts',(3.92982073294257,-1.,-1.14767779451124));
#35500=CARTESIAN_POINT('Ctrl Pts',(3.92385513133997,-1.,-1.14276220561593));
#35501=CARTESIAN_POINT('Ctrl Pts',(3.91787251936827,-1.,-1.13788084225554));
#35502=CARTESIAN_POINT('Ctrl Pts',(3.91187321145649,-1.,-1.13303414693896));
#35503=CARTESIAN_POINT('Ctrl Pts',(3.90585753318737,-1.,-1.12822258281553));
#35504=CARTESIAN_POINT('Ctrl Pts',(3.89982569750025,-1.,-1.12344660099043));
#35505=CARTESIAN_POINT('Ctrl Pts',(3.89377768340344,-1.,-1.11870660794603));
#35506=CARTESIAN_POINT('Ctrl Pts',(3.88771308285171,-1.,-1.11400292434429));
#35507=CARTESIAN_POINT('Ctrl Pts',(3.88163105531724,-1.,-1.10933577224008));
#35508=CARTESIAN_POINT('Ctrl Pts',(3.87553067187514,-1.,-1.10470536603287));
#35509=CARTESIAN_POINT('Ctrl Pts',(3.86941120134849,-1.,-1.10011198761195));
#35510=CARTESIAN_POINT('Ctrl Pts',(3.86327241021247,-1.,-1.09555606505013));
#35511=CARTESIAN_POINT('Ctrl Pts',(3.85711487933931,-1.,-1.09103825516294));
#35512=CARTESIAN_POINT('Ctrl Pts',(3.85094025222713,-1.,-1.08655950846384));
#35513=CARTESIAN_POINT('Ctrl Pts',(3.8447504803063,-1.,-1.08212087917991));
#35514=CARTESIAN_POINT('Ctrl Pts',(3.83854714117491,-1.,-1.07772335353858));
#35515=CARTESIAN_POINT('Ctrl Pts',(3.83233071195144,-1.,-1.07336766633459));
#35516=CARTESIAN_POINT('Ctrl Pts',(3.82609989967276,-1.,-1.06905413180359));
#35517=CARTESIAN_POINT('Ctrl Pts',(3.81985083953012,-1.,-1.0647824403893));
#35518=CARTESIAN_POINT('Ctrl Pts',(3.8135786611749,-1.,-1.06055206187299));
#35519=CARTESIAN_POINT('Ctrl Pts',(3.80727913637791,-1.,-1.05636266918644));
#35520=CARTESIAN_POINT('Ctrl Pts',(3.80095039790681,-1.,-1.05221457990016));
#35521=CARTESIAN_POINT('Ctrl Pts',(3.79459440308786,-1.,-1.04810913267639));
#35522=CARTESIAN_POINT('Ctrl Pts',(3.78821910787179,-1.,-1.04404924374422));
#35523=CARTESIAN_POINT('Ctrl Pts',(3.7818353500817,-1.,-1.04003862055798));
#35524=CARTESIAN_POINT('Ctrl Pts',(3.77545283140427,-1.,-1.03608074678008));
#35525=CARTESIAN_POINT('Ctrl Pts',(3.76907609832516,-1.,-1.03217786604919));
#35526=CARTESIAN_POINT('Ctrl Pts',(3.76270122291245,-1.,-1.02833014458184));
#35527=CARTESIAN_POINT('Ctrl Pts',(3.75631037456224,-1.,-1.02453429444668));
#35528=CARTESIAN_POINT('Ctrl Pts',(3.74987777155873,-1.,-1.02078510487439));
#35529=CARTESIAN_POINT('Ctrl Pts',(3.74337942504993,-1.,-1.01707794311088));
#35530=CARTESIAN_POINT('Ctrl Pts',(3.73680245055747,-1.,-1.01341114319906));
#35531=CARTESIAN_POINT('Ctrl Pts',(3.73015276704407,-1.,-1.00978798539491));
#35532=CARTESIAN_POINT('Ctrl Pts',(3.72346803750544,-1.,-1.00622000735696));
#35533=CARTESIAN_POINT('Ctrl Pts',(3.71680667125047,-1.,-1.00272423396802));
#35534=CARTESIAN_POINT('Ctrl Pts',(3.7102243971387,-1.,-0.999317260756345));
#35535=CARTESIAN_POINT('Ctrl Pts',(3.70375282282107,-1.,-0.996009819772432));
#35536=CARTESIAN_POINT('Ctrl Pts',(3.69738123415696,-1.,-0.992802218332104));
#35537=CARTESIAN_POINT('Ctrl Pts',(3.69102682138955,-1.,-0.989676715398859));
#35538=CARTESIAN_POINT('Ctrl Pts',(3.6845531792623,-1.,-0.986602639864286));
#35539=CARTESIAN_POINT('Ctrl Pts',(3.67782408841876,-1.,-0.983550791470865));
#35540=CARTESIAN_POINT('Ctrl Pts',(3.67074983340444,-1.,-0.980505922458495));
#35541=CARTESIAN_POINT('Ctrl Pts',(3.66333049637403,-1.,-0.977478312751416));
#35542=CARTESIAN_POINT('Ctrl Pts',(3.6557157673487,-1.,-0.974519971354139));
#35543=CARTESIAN_POINT('Ctrl Pts',(3.64819756447072,-1.,-0.971722122060278));
#35544=CARTESIAN_POINT('Ctrl Pts',(3.64113946505393,-1.,-0.969195124674829));
#35545=CARTESIAN_POINT('Ctrl Pts',(3.6349212208096,-1.,-0.967052554540878));
#35546=CARTESIAN_POINT('Ctrl Pts',(3.62988252139998,-1.,-0.965395153165716));
#35547=CARTESIAN_POINT('Ctrl Pts',(3.62652618145252,-1.,-0.964373850166081));
#35548=CARTESIAN_POINT('Ctrl Pts',(3.62489305727516,-1.,-0.963957782642589));
#35549=CARTESIAN_POINT('Ctrl Pts',(3.62424461507455,-1.,-0.963861297423579));
#35550=CARTESIAN_POINT('Ctrl Pts',(3.62404828878374,-1.,-0.963880158556713));
#35551=CARTESIAN_POINT('Ctrl Pts',(3.62400312501199,-1.,-0.963899035118986));
#35552=CARTESIAN_POINT('',(3.66661143271648,-1.,-0.786422660833743));
#35553=CARTESIAN_POINT('Origin',(0.,-1.,0.));
#35554=CARTESIAN_POINT('',(4.13571194405636,-1.,-0.73204283740062));
#35555=CARTESIAN_POINT('Ctrl Pts',(3.66661143271648,-1.,-0.786422660833743));
#35556=CARTESIAN_POINT('Ctrl Pts',(3.66664310415236,-1.,-0.786459983896781));
#35557=CARTESIAN_POINT('Ctrl Pts',(3.66680946938396,-1.,-0.78656591955989));
#35558=CARTESIAN_POINT('Ctrl Pts',(3.66743103898844,-1.,-0.7867743371985));
#35559=CARTESIAN_POINT('Ctrl Pts',(3.66907505398769,-1.,-0.787145041181589));
#35560=CARTESIAN_POINT('Ctrl Pts',(3.672529236635,-1.,-0.787758799995427));
#35561=CARTESIAN_POINT('Ctrl Pts',(3.67777119516438,-1.,-0.788569566220663));
#35562=CARTESIAN_POINT('Ctrl Pts',(3.68428439784285,-1.,-0.789483546065159));
#35563=CARTESIAN_POINT('Ctrl Pts',(3.69172044327754,-1.,-0.79043628498958));
#35564=CARTESIAN_POINT('Ctrl Pts',(3.69968940808982,-1.,-0.791356575696509));
#35565=CARTESIAN_POINT('Ctrl Pts',(3.70781724021879,-1.,-0.792177688845968));
#35566=CARTESIAN_POINT('Ctrl Pts',(3.7158024239604,-1.,-0.792848377370116));
#35567=CARTESIAN_POINT('Ctrl Pts',(3.7234879729357,-1.,-0.793347023783871));
#35568=CARTESIAN_POINT('Ctrl Pts',(3.7308691469564,-1.,-0.793682750269348));
#35569=CARTESIAN_POINT('Ctrl Pts',(3.73803280541576,-1.,-0.793882700936791));
#35570=CARTESIAN_POINT('Ctrl Pts',(3.74511357728827,-1.,-0.79398270045988));
#35571=CARTESIAN_POINT('Ctrl Pts',(3.75224692493895,-1.,-0.794017347371441));
#35572=CARTESIAN_POINT('Ctrl Pts',(3.75951468666325,-1.,-0.794008429135047));
#35573=CARTESIAN_POINT('Ctrl Pts',(3.76692626931184,-1.,-0.793961083689141));
#35574=CARTESIAN_POINT('Ctrl Pts',(3.77444863801264,-1.,-0.793870523787515));
#35575=CARTESIAN_POINT('Ctrl Pts',(3.78202460377617,-1.,-0.79372623578134));
#35576=CARTESIAN_POINT('Ctrl Pts',(3.78959439439222,-1.,-0.793516871680966));
#35577=CARTESIAN_POINT('Ctrl Pts',(3.79711921389862,-1.,-0.793235612973201));
#35578=CARTESIAN_POINT('Ctrl Pts',(3.80459229925598,-1.,-0.792882695234693));
#35579=CARTESIAN_POINT('Ctrl Pts',(3.81202588694726,-1.,-0.792462483517568));
#35580=CARTESIAN_POINT('Ctrl Pts',(3.81944345442237,-1.,-0.791981740718607));
#35581=CARTESIAN_POINT('Ctrl Pts',(3.82687033899799,-1.,-0.791447528662381));
#35582=CARTESIAN_POINT('Ctrl Pts',(3.83432392054804,-1.,-0.79086501270534));
#35583=CARTESIAN_POINT('Ctrl Pts',(3.84180762342476,-1.,-0.790236124191289));
#35584=CARTESIAN_POINT('Ctrl Pts',(3.8493163780891,-1.,-0.789560798155619));
#35585=CARTESIAN_POINT('Ctrl Pts',(3.85683995872536,-1.,-0.788837734090688));
#35586=CARTESIAN_POINT('Ctrl Pts',(3.86436702561342,-1.,-0.788065315093771));
#35587=CARTESIAN_POINT('Ctrl Pts',(3.87188916600905,-1.,-0.787242527617981));
#35588=CARTESIAN_POINT('Ctrl Pts',(3.87940402818186,-1.,-0.786369675812592));
#35589=CARTESIAN_POINT('Ctrl Pts',(3.88691313167399,-1.,-0.785447890340723));
#35590=CARTESIAN_POINT('Ctrl Pts',(3.89442039235105,-1.,-0.784478799358336));
#35591=CARTESIAN_POINT('Ctrl Pts',(3.90193039043971,-1.,-0.783464141529083));
#35592=CARTESIAN_POINT('Ctrl Pts',(3.90944671004536,-1.,-0.782405395622759));
#35593=CARTESIAN_POINT('Ctrl Pts',(3.9169703605466,-1.,-0.781303428618344));
#35594=CARTESIAN_POINT('Ctrl Pts',(3.92450058323799,-1.,-0.780158678615507));
#35595=CARTESIAN_POINT('Ctrl Pts',(3.93203552473153,-1.,-0.778971308134786));
#35596=CARTESIAN_POINT('Ctrl Pts',(3.93957296768098,-1.,-0.77774137056855));
#35597=CARTESIAN_POINT('Ctrl Pts',(3.94711101619471,-1.,-0.77646896669796));
#35598=CARTESIAN_POINT('Ctrl Pts',(3.95464885452364,-1.,-0.775154418039442));
#35599=CARTESIAN_POINT('Ctrl Pts',(3.96218649639876,-1.,-0.773798212026683));
#35600=CARTESIAN_POINT('Ctrl Pts',(3.96972446532832,-1.,-0.772400931772239));
#35601=CARTESIAN_POINT('Ctrl Pts',(3.97726349165507,-1.,-0.770963190030504));
#35602=CARTESIAN_POINT('Ctrl Pts',(3.98480422348403,-1.,-0.76948556624546));
#35603=CARTESIAN_POINT('Ctrl Pts',(3.99234687880892,-1.,-0.767968531377708));
#35604=CARTESIAN_POINT('Ctrl Pts',(3.99989129179464,-1.,-0.766412457135786));
#35605=CARTESIAN_POINT('Ctrl Pts',(4.00743706791366,-1.,-0.764817648784947));
#35606=CARTESIAN_POINT('Ctrl Pts',(4.01498370680434,-1.,-0.763184371182827));
#35607=CARTESIAN_POINT('Ctrl Pts',(4.02253072741347,-1.,-0.761512875859942));
#35608=CARTESIAN_POINT('Ctrl Pts',(4.0300778195465,-1.,-0.759803433244166));
#35609=CARTESIAN_POINT('Ctrl Pts',(4.03762485803468,-1.,-0.758056338885554));
#35610=CARTESIAN_POINT('Ctrl Pts',(4.04517182654344,-1.,-0.756271902370187));
#35611=CARTESIAN_POINT('Ctrl Pts',(4.05271876688106,-1.,-0.754450441816412));
#35612=CARTESIAN_POINT('Ctrl Pts',(4.06026572221399,-1.,-0.752592276482869));
#35613=CARTESIAN_POINT('Ctrl Pts',(4.06781267241886,-1.,-0.750697720483176));
#35614=CARTESIAN_POINT('Ctrl Pts',(4.07535951055363,-1.,-0.748767076679177));
#35615=CARTESIAN_POINT('Ctrl Pts',(4.08290608094789,-1.,-0.746800631490822));
#35616=CARTESIAN_POINT('Ctrl Pts',(4.09045220253011,-1.,-0.744798649705514));
#35617=CARTESIAN_POINT('Ctrl Pts',(4.09799769702712,-1.,-0.742761369690018));
#35618=CARTESIAN_POINT('Ctrl Pts',(4.1055424175856,-1.,-0.740688998555152));
#35619=CARTESIAN_POINT('Ctrl Pts',(4.11308626953795,-1.,-0.738581708229119));
#35620=CARTESIAN_POINT('Ctrl Pts',(4.12062919626082,-1.,-0.736439634335347));
#35621=CARTESIAN_POINT('Ctrl Pts',(4.12666277572794,-1.,-0.734698226767513));
#35622=CARTESIAN_POINT('Ctrl Pts',(4.13118752796397,-1.,-0.733376589325634));
#35623=CARTESIAN_POINT('Ctrl Pts',(4.13420383737278,-1.,-0.732488575135926));
#35624=CARTESIAN_POINT('Ctrl Pts',(4.13571194405636,-1.,-0.73204283740062));
#35625=CARTESIAN_POINT('',(4.15950947128175,-1.,-0.581791163835815));
#35626=CARTESIAN_POINT('',(4.13571194405636,-1.,-0.73204283740062));
#35627=CARTESIAN_POINT('',(3.73017266276632,-1.,-0.385112848332549));
#35628=CARTESIAN_POINT('Ctrl Pts',(4.15950947128175,-1.,-0.581791163835815));
#35629=CARTESIAN_POINT('Ctrl Pts',(4.15821291712391,-1.,-0.580901211462913));
#35630=CARTESIAN_POINT('Ctrl Pts',(4.15561864787379,-1.,-0.579124568912544));
#35631=CARTESIAN_POINT('Ctrl Pts',(4.1517237611974,-1.,-0.576469391673917));
#35632=CARTESIAN_POINT('Ctrl Pts',(4.14652361065787,-1.,-0.572948736066277));
#35633=CARTESIAN_POINT('Ctrl Pts',(4.14001179828669,-1.,-0.568580610187116));
#35634=CARTESIAN_POINT('Ctrl Pts',(4.13348835726086,-1.,-0.564245279535706));
#35635=CARTESIAN_POINT('Ctrl Pts',(4.12695329951859,-1.,-0.559942890594628));
#35636=CARTESIAN_POINT('Ctrl Pts',(4.1204066619623,-1.,-0.555673636130778));
#35637=CARTESIAN_POINT('Ctrl Pts',(4.11384852025578,-1.,-0.551437758498247));
#35638=CARTESIAN_POINT('Ctrl Pts',(4.1072789702877,-1.,-0.54723553948676));
#35639=CARTESIAN_POINT('Ctrl Pts',(4.10069810244473,-1.,-0.543067286878457));
#35640=CARTESIAN_POINT('Ctrl Pts',(4.09410597627116,-1.,-0.538933321179921));
#35641=CARTESIAN_POINT('Ctrl Pts',(4.08750259988693,-1.,-0.534833963477));
#35642=CARTESIAN_POINT('Ctrl Pts',(4.08088789536488,-1.,-0.530769518728076));
#35643=CARTESIAN_POINT('Ctrl Pts',(4.07426172299496,-1.,-0.526740277227));
#35644=CARTESIAN_POINT('Ctrl Pts',(4.06762394471075,-1.,-0.522746528602768));
#35645=CARTESIAN_POINT('Ctrl Pts',(4.06097448037934,-1.,-0.51878857233681));
#35646=CARTESIAN_POINT('Ctrl Pts',(4.05431335771261,-1.,-0.514866728193104));
#35647=CARTESIAN_POINT('Ctrl Pts',(4.04764078815591,-1.,-0.510981349219174));
#35648=CARTESIAN_POINT('Ctrl Pts',(4.04095715149074,-1.,-0.507132823288362));
#35649=CARTESIAN_POINT('Ctrl Pts',(4.0342628417439,-1.,-0.503321556915514));
#35650=CARTESIAN_POINT('Ctrl Pts',(4.0275581398015,-1.,-0.49954796234089));
#35651=CARTESIAN_POINT('Ctrl Pts',(4.02084308851813,-1.,-0.495812444326223));
#35652=CARTESIAN_POINT('Ctrl Pts',(4.01411733503486,-1.,-0.492115383417931));
#35653=CARTESIAN_POINT('Ctrl Pts',(4.0073800839092,-1.,-0.488457130424531));
#35654=CARTESIAN_POINT('Ctrl Pts',(4.00063045119234,-1.,-0.484838042421754));
#35655=CARTESIAN_POINT('Ctrl Pts',(3.99386775880655,-1.,-0.481258512209638));
#35656=CARTESIAN_POINT('Ctrl Pts',(3.98709184306743,-1.,-0.477718999122033));
#35657=CARTESIAN_POINT('Ctrl Pts',(3.9803033804443,-1.,-0.474220061019542));
#35658=CARTESIAN_POINT('Ctrl Pts',(3.97350414289415,-1.,-0.470762379613478));
#35659=CARTESIAN_POINT('Ctrl Pts',(3.96669622273946,-1.,-0.467346690880672));
#35660=CARTESIAN_POINT('Ctrl Pts',(3.95988133243543,-1.,-0.463973722115745));
#35661=CARTESIAN_POINT('Ctrl Pts',(3.95306005817363,-1.,-0.460644124429119));
#35662=CARTESIAN_POINT('Ctrl Pts',(3.94623117206675,-1.,-0.457358410451674));
#35663=CARTESIAN_POINT('Ctrl Pts',(3.93939080846298,-1.,-0.454116879027576));
#35664=CARTESIAN_POINT('Ctrl Pts',(3.93253407403128,-1.,-0.450919768356347));
#35665=CARTESIAN_POINT('Ctrl Pts',(3.92565674143424,-1.,-0.447767416837297));
#35666=CARTESIAN_POINT('Ctrl Pts',(3.91875701610721,-1.,-0.444660430230593));
#35667=CARTESIAN_POINT('Ctrl Pts',(3.91183704069146,-1.,-0.441599824524048));
#35668=CARTESIAN_POINT('Ctrl Pts',(3.90490512938546,-1.,-0.438587235458234));
#35669=CARTESIAN_POINT('Ctrl Pts',(3.8979725665544,-1.,-0.435624629433506));
#35670=CARTESIAN_POINT('Ctrl Pts',(3.89104947940592,-1.,-0.43271392954444));
#35671=CARTESIAN_POINT('Ctrl Pts',(3.88414070943334,-1.,-0.429856640579734));
#35672=CARTESIAN_POINT('Ctrl Pts',(3.87724240306609,-1.,-0.427053541173469));
#35673=CARTESIAN_POINT('Ctrl Pts',(3.87033643487882,-1.,-0.424304173195143));
#35674=CARTESIAN_POINT('Ctrl Pts',(3.86339652542749,-1.,-0.421607423177576));
#35675=CARTESIAN_POINT('Ctrl Pts',(3.85639825648031,-1.,-0.41896246808681));
#35676=CARTESIAN_POINT('Ctrl Pts',(3.8493286415751,-1.,-0.41636967805292));
#35677=CARTESIAN_POINT('Ctrl Pts',(3.84219403994742,-1.,-0.413831367016727));
#35678=CARTESIAN_POINT('Ctrl Pts',(3.83503345578645,-1.,-0.41135303879846));
#35679=CARTESIAN_POINT('Ctrl Pts',(3.82790724256397,-1.,-0.408942371447377));
#35680=CARTESIAN_POINT('Ctrl Pts',(3.82087303913741,-1.,-0.406607038258907));
#35681=CARTESIAN_POINT('Ctrl Pts',(3.81396374287762,-1.,-0.404352694628237));
#35682=CARTESIAN_POINT('Ctrl Pts',(3.80716881962763,-1.,-0.402181320148475));
#35683=CARTESIAN_POINT('Ctrl Pts',(3.80040370384659,-1.,-0.400088346504727));
#35684=CARTESIAN_POINT('Ctrl Pts',(3.79352887163457,-1.,-0.398064818684159));
#35685=CARTESIAN_POINT('Ctrl Pts',(3.78640521279479,-1.,-0.396103205335029));
#35686=CARTESIAN_POINT('Ctrl Pts',(3.77894173114368,-1.,-0.394202481011595));
#35687=CARTESIAN_POINT('Ctrl Pts',(3.77114011595892,-1.,-0.392372786223347));
#35688=CARTESIAN_POINT('Ctrl Pts',(3.76315635032993,-1.,-0.390642072979259));
#35689=CARTESIAN_POINT('Ctrl Pts',(3.75529302894757,-1.,-0.389054775898251));
#35690=CARTESIAN_POINT('Ctrl Pts',(3.74792651696269,-1.,-0.387663020050396));
#35691=CARTESIAN_POINT('Ctrl Pts',(3.74144965781088,-1.,-0.386519576222036));
#35692=CARTESIAN_POINT('Ctrl Pts',(3.73621371845475,-1.,-0.385670806454744));
#35693=CARTESIAN_POINT('Ctrl Pts',(3.73273893363318,-1.,-0.385187124633965));
#35694=CARTESIAN_POINT('Ctrl Pts',(3.73106082862399,-1.,-0.385031656499142));
#35695=CARTESIAN_POINT('Ctrl Pts',(3.73040527620929,-1.,-0.385037797882046));
#35696=CARTESIAN_POINT('Ctrl Pts',(3.73021431755218,-1.,-0.385087139001609));
#35697=CARTESIAN_POINT('Ctrl Pts',(3.73017266276632,-1.,-0.385112848332549));
#35698=CARTESIAN_POINT('',(3.74449296982994,-1.,-0.203156094897896));
#35699=CARTESIAN_POINT('Origin',(0.,-1.,0.));
#35700=CARTESIAN_POINT('',(4.19931119685982,-1.,-0.0760622897878241));
#35701=CARTESIAN_POINT('Ctrl Pts',(3.74449296982994,-1.,-0.203156094897896));
#35702=CARTESIAN_POINT('Ctrl Pts',(3.74453008995129,-1.,-0.203188003947965));
#35703=CARTESIAN_POINT('Ctrl Pts',(3.74471097893961,-1.,-0.203266610111264));
#35704=CARTESIAN_POINT('Ctrl Pts',(3.74535749969262,-1.,-0.203375226874332));
#35705=CARTESIAN_POINT('Ctrl Pts',(3.74703926501843,-1.,-0.203484186269315));
#35706=CARTESIAN_POINT('Ctrl Pts',(3.75054693397716,-1.,-0.203550035479097));
#35707=CARTESIAN_POINT('Ctrl Pts',(3.75585118707924,-1.,-0.203530796848404));
#35708=CARTESIAN_POINT('Ctrl Pts',(3.76242717937273,-1.,-0.203414634707647));
#35709=CARTESIAN_POINT('Ctrl Pts',(3.76992071595267,-1.,-0.203192390045338));
#35710=CARTESIAN_POINT('Ctrl Pts',(3.77793553476879,-1.,-0.202854729699197));
#35711=CARTESIAN_POINT('Ctrl Pts',(3.78609175019317,-1.,-0.202394260512193));
#35712=CARTESIAN_POINT('Ctrl Pts',(3.79408354187274,-1.,-0.201807533800799));
#35713=CARTESIAN_POINT('Ctrl Pts',(3.80175247447171,-1.,-0.201097756307252));
#35714=CARTESIAN_POINT('Ctrl Pts',(3.80909529318501,-1.,-0.20027467943329));
#35715=CARTESIAN_POINT('Ctrl Pts',(3.81620203429702,-1.,-0.199351525297397));
#35716=CARTESIAN_POINT('Ctrl Pts',(3.82321127348981,-1.,-0.19834261690047));
#35717=CARTESIAN_POINT('Ctrl Pts',(3.83026221776488,-1.,-0.197260935827375));
#35718=CARTESIAN_POINT('Ctrl Pts',(3.83743910616265,-1.,-0.19611519897189));
#35719=CARTESIAN_POINT('Ctrl Pts',(3.84475203347052,-1.,-0.194909009460255));
#35720=CARTESIAN_POINT('Ctrl Pts',(3.85216762264019,-1.,-0.193642806777748));
#35721=CARTESIAN_POINT('Ctrl Pts',(3.85962774407652,-1.,-0.19231515304498));
#35722=CARTESIAN_POINT('Ctrl Pts',(3.8670715862477,-1.,-0.190924190418613));
#35723=CARTESIAN_POINT('Ctrl Pts',(3.87445976418377,-1.,-0.189469253358255));
#35724=CARTESIAN_POINT('Ctrl Pts',(3.88178563496187,-1.,-0.187951632512664));
#35725=CARTESIAN_POINT('Ctrl Pts',(3.88906196725817,-1.,-0.186373724985263));
#35726=CARTESIAN_POINT('Ctrl Pts',(3.89631300742633,-1.,-0.184738537728035));
#35727=CARTESIAN_POINT('Ctrl Pts',(3.90356488555138,-1.,-0.183049081993193));
#35728=CARTESIAN_POINT('Ctrl Pts',(3.91083557557193,-1.,-0.181307740731796));
#35729=CARTESIAN_POINT('Ctrl Pts',(3.91812876180948,-1.,-0.179515885822895));
#35730=CARTESIAN_POINT('Ctrl Pts',(3.92543942697672,-1.,-0.177674246152328));
#35731=CARTESIAN_POINT('Ctrl Pts',(3.93275726771049,-1.,-0.175783136893873));
#35732=CARTESIAN_POINT('Ctrl Pts',(3.94007083096214,-1.,-0.173842734974608));
#35733=CARTESIAN_POINT('Ctrl Pts',(3.94737164900861,-1.,-0.171853355369233));
#35734=CARTESIAN_POINT('Ctrl Pts',(3.95465744665263,-1.,-0.16981566637413));
#35735=CARTESIAN_POINT('Ctrl Pts',(3.96192990160296,-1.,-0.167730547023312));
#35736=CARTESIAN_POINT('Ctrl Pts',(3.9691931362141,-1.,-0.165598992851098));
#35737=CARTESIAN_POINT('Ctrl Pts',(3.97645194630944,-1.,-0.163422004609999));
#35738=CARTESIAN_POINT('Ctrl Pts',(3.98371010319866,-1.,-0.161200482186088));
#35739=CARTESIAN_POINT('Ctrl Pts',(3.99096873945862,-1.,-0.158935123982796));
#35740=CARTESIAN_POINT('Ctrl Pts',(3.99822717425869,-1.,-0.156626481393736));
#35741=CARTESIAN_POINT('Ctrl Pts',(4.00548360245297,-1.,-0.15427500487231));
#35742=CARTESIAN_POINT('Ctrl Pts',(4.01273584234684,-1.,-0.151881094022909));
#35743=CARTESIAN_POINT('Ctrl Pts',(4.01998203715588,-1.,-0.149445144968708));
#35744=CARTESIAN_POINT('Ctrl Pts',(4.02722143147048,-1.,-0.146967602878999));
#35745=CARTESIAN_POINT('Ctrl Pts',(4.03445411510403,-1.,-0.144448947038352));
#35746=CARTESIAN_POINT('Ctrl Pts',(4.04168069633842,-1.,-0.141889671485508));
#35747=CARTESIAN_POINT('Ctrl Pts',(4.04890199238056,-1.,-0.13929026718006));
#35748=CARTESIAN_POINT('Ctrl Pts',(4.05611873400122,-1.,-0.136651205046111));
#35749=CARTESIAN_POINT('Ctrl Pts',(4.06333121018476,-1.,-0.133972916144225));
#35750=CARTESIAN_POINT('Ctrl Pts',(4.07053931528579,-1.,-0.131255793548914));
#35751=CARTESIAN_POINT('Ctrl Pts',(4.07774270738809,-1.,-0.128500200484814));
#35752=CARTESIAN_POINT('Ctrl Pts',(4.08494093372315,-1.,-0.12570647682253));
#35753=CARTESIAN_POINT('Ctrl Pts',(4.09213355850836,-1.,-0.122874946249119));
#35754=CARTESIAN_POINT('Ctrl Pts',(4.09932031767243,-1.,-0.120005924388162));
#35755=CARTESIAN_POINT('Ctrl Pts',(4.10650113382187,-1.,-0.117099722731705));
#35756=CARTESIAN_POINT('Ctrl Pts',(4.11367603925313,-1.,-0.114156649609602));
#35757=CARTESIAN_POINT('Ctrl Pts',(4.12084512502444,-1.,-0.111177012683378));
#35758=CARTESIAN_POINT('Ctrl Pts',(4.12800848371386,-1.,-0.10816112052835));
#35759=CARTESIAN_POINT('Ctrl Pts',(4.13516614458396,-1.,-0.105109286538864));
#35760=CARTESIAN_POINT('Ctrl Pts',(4.14231804938737,-1.,-0.102021826577454));
#35761=CARTESIAN_POINT('Ctrl Pts',(4.1494640891762,-1.,-0.0988990478899816));
#35762=CARTESIAN_POINT('Ctrl Pts',(4.15660412653006,-1.,-0.0957412403297072));
#35763=CARTESIAN_POINT('Ctrl Pts',(4.16373802265942,-1.,-0.0925486672167695));
#35764=CARTESIAN_POINT('Ctrl Pts',(4.17086566491823,-1.,-0.0893215560850332));
#35765=CARTESIAN_POINT('Ctrl Pts',(4.17798698669991,-1.,-0.086060091555252));
#35766=CARTESIAN_POINT('Ctrl Pts',(4.1851019532944,-1.,-0.0827644164389515));
#35767=CARTESIAN_POINT('Ctrl Pts',(4.19078883322483,-1.,-0.0801005887117608));
#35768=CARTESIAN_POINT('Ctrl Pts',(4.19505112860624,-1.,-0.0780873956244407));
#35769=CARTESIAN_POINT('Ctrl Pts',(4.19789138621624,-1.,-0.07673845961422));
#35770=CARTESIAN_POINT('Ctrl Pts',(4.19931119685982,-1.,-0.0760622897878241));
#35771=CARTESIAN_POINT('',(4.19931119685982,-1.,0.0760622897878241));
#35772=CARTESIAN_POINT('',(4.19931119685982,-1.,-0.0760622897878241));
#35773=CARTESIAN_POINT('',(3.74449296983004,-1.,0.2031560948961));
#35774=CARTESIAN_POINT('Ctrl Pts',(4.19931119685982,-1.,0.0760622897878241));
#35775=CARTESIAN_POINT('Ctrl Pts',(4.1978913862118,-1.,0.0767384596141459));
#35776=CARTESIAN_POINT('Ctrl Pts',(4.19505112859416,-1.,0.0780873956242392));
#35777=CARTESIAN_POINT('Ctrl Pts',(4.19078883320504,-1.,0.0801005887114315));
#35778=CARTESIAN_POINT('Ctrl Pts',(4.18510195327123,-1.,0.0827644164385674));
#35779=CARTESIAN_POINT('Ctrl Pts',(4.17798698668094,-1.,0.0860600915549391));
#35780=CARTESIAN_POINT('Ctrl Pts',(4.17086566490794,-1.,0.0893215560848644));
#35781=CARTESIAN_POINT('Ctrl Pts',(4.16373802265839,-1.,0.0925486672167526));
#35782=CARTESIAN_POINT('Ctrl Pts',(4.15660412653577,-1.,0.0957412403298002));
#35783=CARTESIAN_POINT('Ctrl Pts',(4.14946408918485,-1.,0.0988990478901221));
#35784=CARTESIAN_POINT('Ctrl Pts',(4.14231804939538,-1.,0.102021826577583));
#35785=CARTESIAN_POINT('Ctrl Pts',(4.13516614458895,-1.,0.105109286538945));
#35786=CARTESIAN_POINT('Ctrl Pts',(4.12800848371504,-1.,0.108161120528369));
#35787=CARTESIAN_POINT('Ctrl Pts',(4.1208451250225,-1.,0.111177012683346));
#35788=CARTESIAN_POINT('Ctrl Pts',(4.11367603924961,-1.,0.114156649609545));
#35789=CARTESIAN_POINT('Ctrl Pts',(4.10650113381833,-1.,0.117099722731648));
#35790=CARTESIAN_POINT('Ctrl Pts',(4.09932031767002,-1.,0.120005924388124));
#35791=CARTESIAN_POINT('Ctrl Pts',(4.09213355850756,-1.,0.122874946249106));
#35792=CARTESIAN_POINT('Ctrl Pts',(4.08494093372377,-1.,0.125706476822539));
#35793=CARTESIAN_POINT('Ctrl Pts',(4.07774270738954,-1.,0.128500200484837));
#35794=CARTESIAN_POINT('Ctrl Pts',(4.0705393152874,-1.,0.13125579354894));
#35795=CARTESIAN_POINT('Ctrl Pts',(4.06333121018596,-1.,0.133972916144244));
#35796=CARTESIAN_POINT('Ctrl Pts',(4.05611873400172,-1.,0.136651205046119));
#35797=CARTESIAN_POINT('Ctrl Pts',(4.04890199238036,-1.,0.139290267180057));
#35798=CARTESIAN_POINT('Ctrl Pts',(4.04168069633781,-1.,0.1418896714855));
#35799=CARTESIAN_POINT('Ctrl Pts',(4.03445411510333,-1.,0.144448947038344));
#35800=CARTESIAN_POINT('Ctrl Pts',(4.02722143146994,-1.,0.146967602878994));
#35801=CARTESIAN_POINT('Ctrl Pts',(4.01998203715564,-1.,0.149445144968706));
#35802=CARTESIAN_POINT('Ctrl Pts',(4.01273584234689,-1.,0.15188109402291));
#35803=CARTESIAN_POINT('Ctrl Pts',(4.00548360245319,-1.,0.15427500487231));
#35804=CARTESIAN_POINT('Ctrl Pts',(3.99822717425893,-1.,0.156626481393734));
#35805=CARTESIAN_POINT('Ctrl Pts',(3.99096873945878,-1.,0.158935123982793));
#35806=CARTESIAN_POINT('Ctrl Pts',(3.98371010319872,-1.,0.161200482186084));
#35807=CARTESIAN_POINT('Ctrl Pts',(3.97645194630943,-1.,0.163422004609999));
#35808=CARTESIAN_POINT('Ctrl Pts',(3.96919313621407,-1.,0.165598992851102));
#35809=CARTESIAN_POINT('Ctrl Pts',(3.96192990160296,-1.,0.167730547023319));
#35810=CARTESIAN_POINT('Ctrl Pts',(3.95465744665268,-1.,0.169815666374138));
#35811=CARTESIAN_POINT('Ctrl Pts',(3.94737164900868,-1.,0.17185335536924));
#35812=CARTESIAN_POINT('Ctrl Pts',(3.94007083096217,-1.,0.173842734974609));
#35813=CARTESIAN_POINT('Ctrl Pts',(3.93275726771042,-1.,0.175783136893867));
#35814=CARTESIAN_POINT('Ctrl Pts',(3.92543942697655,-1.,0.177674246152317));
#35815=CARTESIAN_POINT('Ctrl Pts',(3.91812876180926,-1.,0.179515885822881));
#35816=CARTESIAN_POINT('Ctrl Pts',(3.91083557557175,-1.,0.181307740731785));
#35817=CARTESIAN_POINT('Ctrl Pts',(3.90356488555132,-1.,0.18304908199319));
#35818=CARTESIAN_POINT('Ctrl Pts',(3.89631300742646,-1.,0.184738537728042));
#35819=CARTESIAN_POINT('Ctrl Pts',(3.88906196725848,-1.,0.18637372498528));
#35820=CARTESIAN_POINT('Ctrl Pts',(3.88178563496228,-1.,0.187951632512684));
#35821=CARTESIAN_POINT('Ctrl Pts',(3.87445976418412,-1.,0.189469253358272));
#35822=CARTESIAN_POINT('Ctrl Pts',(3.86707158624783,-1.,0.190924190418619));
#35823=CARTESIAN_POINT('Ctrl Pts',(3.85962774407633,-1.,0.19231515304497));
#35824=CARTESIAN_POINT('Ctrl Pts',(3.85216762263966,-1.,0.193642806777722));
#35825=CARTESIAN_POINT('Ctrl Pts',(3.84475203346977,-1.,0.19490900946022));
#35826=CARTESIAN_POINT('Ctrl Pts',(3.83743910616195,-1.,0.196115198971858));
#35827=CARTESIAN_POINT('Ctrl Pts',(3.83026221776456,-1.,0.197260935827361));
#35828=CARTESIAN_POINT('Ctrl Pts',(3.82321127349016,-1.,0.198342616900486));
#35829=CARTESIAN_POINT('Ctrl Pts',(3.81620203429815,-1.,0.199351525297447));
#35830=CARTESIAN_POINT('Ctrl Pts',(3.80909529318669,-1.,0.200274679433364));
#35831=CARTESIAN_POINT('Ctrl Pts',(3.80175247447337,-1.,0.201097756307325));
#35832=CARTESIAN_POINT('Ctrl Pts',(3.7940835418736,-1.,0.201807533800837));
#35833=CARTESIAN_POINT('Ctrl Pts',(3.78609175019242,-1.,0.20239426051216));
#35834=CARTESIAN_POINT('Ctrl Pts',(3.77793553476614,-1.,0.20285472969908));
#35835=CARTESIAN_POINT('Ctrl Pts',(3.7699207159487,-1.,0.203192390045164));
#35836=CARTESIAN_POINT('Ctrl Pts',(3.76242717936885,-1.,0.203414634707478));
#35837=CARTESIAN_POINT('Ctrl Pts',(3.75585118707734,-1.,0.203530796848321));
#35838=CARTESIAN_POINT('Ctrl Pts',(3.75054693397875,-1.,0.203550035479166));
#35839=CARTESIAN_POINT('Ctrl Pts',(3.74703926501752,-1.,0.203484186269415));
#35840=CARTESIAN_POINT('Ctrl Pts',(3.74535749969115,-1.,0.203375226874121));
#35841=CARTESIAN_POINT('Ctrl Pts',(3.74471097893845,-1.,0.20326661011053));
#35842=CARTESIAN_POINT('Ctrl Pts',(3.74453008995092,-1.,0.203188003946656));
#35843=CARTESIAN_POINT('Ctrl Pts',(3.74449296983004,-1.,0.2031560948961));
#35844=CARTESIAN_POINT('',(3.73017266276651,-1.,0.385112848330762));
#35845=CARTESIAN_POINT('Origin',(0.,-1.,0.));
#35846=CARTESIAN_POINT('',(4.15950947128175,-1.,0.581791163835816));
#35847=CARTESIAN_POINT('Ctrl Pts',(3.73017266276651,-1.,0.385112848330762));
#35848=CARTESIAN_POINT('Ctrl Pts',(3.73021431755274,-1.,0.385087139000375));
#35849=CARTESIAN_POINT('Ctrl Pts',(3.73040527621055,-1.,0.385037797881504));
#35850=CARTESIAN_POINT('Ctrl Pts',(3.73106082862548,-1.,0.385031656499164));
#35851=CARTESIAN_POINT('Ctrl Pts',(3.73273893363406,-1.,0.385187124634207));
#35852=CARTESIAN_POINT('Ctrl Pts',(3.73621371845318,-1.,0.385670806454566));
#35853=CARTESIAN_POINT('Ctrl Pts',(3.74144965781276,-1.,0.386519576222252));
#35854=CARTESIAN_POINT('Ctrl Pts',(3.74792651696654,-1.,0.387663020050836));
#35855=CARTESIAN_POINT('Ctrl Pts',(3.75529302895152,-1.,0.389054775898702));
#35856=CARTESIAN_POINT('Ctrl Pts',(3.76315635033257,-1.,0.39064207297956));
#35857=CARTESIAN_POINT('Ctrl Pts',(3.77114011595967,-1.,0.392372786223433));
#35858=CARTESIAN_POINT('Ctrl Pts',(3.77894173114283,-1.,0.3942024810115));
#35859=CARTESIAN_POINT('Ctrl Pts',(3.78640521279313,-1.,0.396103205334841));
#35860=CARTESIAN_POINT('Ctrl Pts',(3.7935288716329,-1.,0.39806481868397));
#35861=CARTESIAN_POINT('Ctrl Pts',(3.80040370384546,-1.,0.400088346504601));
#35862=CARTESIAN_POINT('Ctrl Pts',(3.80716881962728,-1.,0.402181320148436));
#35863=CARTESIAN_POINT('Ctrl Pts',(3.81396374287793,-1.,0.404352694628274));
#35864=CARTESIAN_POINT('Ctrl Pts',(3.8208730391381,-1.,0.406607038258986));
#35865=CARTESIAN_POINT('Ctrl Pts',(3.82790724256471,-1.,0.40894237144746));
#35866=CARTESIAN_POINT('Ctrl Pts',(3.83503345578698,-1.,0.411353038798519));
#35867=CARTESIAN_POINT('Ctrl Pts',(3.84219403994762,-1.,0.413831367016748));
#35868=CARTESIAN_POINT('Ctrl Pts',(3.84932864157497,-1.,0.416369678052907));
#35869=CARTESIAN_POINT('Ctrl Pts',(3.85639825647996,-1.,0.418962468086773));
#35870=CARTESIAN_POINT('Ctrl Pts',(3.86339652542709,-1.,0.421607423177534));
#35871=CARTESIAN_POINT('Ctrl Pts',(3.87033643487851,-1.,0.424304173195111));
#35872=CARTESIAN_POINT('Ctrl Pts',(3.87724240306597,-1.,0.427053541173458));
#35873=CARTESIAN_POINT('Ctrl Pts',(3.88414070943341,-1.,0.429856640579741));
#35874=CARTESIAN_POINT('Ctrl Pts',(3.89104947940611,-1.,0.432713929544459));
#35875=CARTESIAN_POINT('Ctrl Pts',(3.89797256655462,-1.,0.435624629433528));
#35876=CARTESIAN_POINT('Ctrl Pts',(3.90490512938563,-1.,0.43858723545825));
#35877=CARTESIAN_POINT('Ctrl Pts',(3.91183704069153,-1.,0.441599824524055));
#35878=CARTESIAN_POINT('Ctrl Pts',(3.91875701610719,-1.,0.444660430230591));
#35879=CARTESIAN_POINT('Ctrl Pts',(3.92565674143416,-1.,0.447767416837293));
#35880=CARTESIAN_POINT('Ctrl Pts',(3.93253407403123,-1.,0.450919768356349));
#35881=CARTESIAN_POINT('Ctrl Pts',(3.93939080846298,-1.,0.454116879027584));
#35882=CARTESIAN_POINT('Ctrl Pts',(3.94623117206678,-1.,0.457358410451683));
#35883=CARTESIAN_POINT('Ctrl Pts',(3.95306005817364,-1.,0.460644124429122));
#35884=CARTESIAN_POINT('Ctrl Pts',(3.95988133243538,-1.,0.463973722115734));
#35885=CARTESIAN_POINT('Ctrl Pts',(3.9666962227393,-1.,0.467346690880644));
#35886=CARTESIAN_POINT('Ctrl Pts',(3.97350414289392,-1.,0.47076237961344));
#35887=CARTESIAN_POINT('Ctrl Pts',(3.98030338044409,-1.,0.47422006101951));
#35888=CARTESIAN_POINT('Ctrl Pts',(3.98709184306738,-1.,0.477718999122028));
#35889=CARTESIAN_POINT('Ctrl Pts',(3.99386775880679,-1.,0.481258512209676));
#35890=CARTESIAN_POINT('Ctrl Pts',(4.00063045119288,-1.,0.484838042421835));
#35891=CARTESIAN_POINT('Ctrl Pts',(4.0073800839099,-1.,0.488457130424634));
#35892=CARTESIAN_POINT('Ctrl Pts',(4.01411733503546,-1.,0.492115383418019));
#35893=CARTESIAN_POINT('Ctrl Pts',(4.02084308851832,-1.,0.495812444326251));
#35894=CARTESIAN_POINT('Ctrl Pts',(4.02755813980101,-1.,0.499547962340822));
#35895=CARTESIAN_POINT('Ctrl Pts',(4.03426284174272,-1.,0.503321556915346));
#35896=CARTESIAN_POINT('Ctrl Pts',(4.04095715148915,-1.,0.507132823288137));
#35897=CARTESIAN_POINT('Ctrl Pts',(4.04764078815447,-1.,0.510981349218971));
#35898=CARTESIAN_POINT('Ctrl Pts',(4.05431335771199,-1.,0.514866728193017));
#35899=CARTESIAN_POINT('Ctrl Pts',(4.06097448038013,-1.,0.518788572336924));
#35900=CARTESIAN_POINT('Ctrl Pts',(4.06762394471314,-1.,0.522746528603108));
#35901=CARTESIAN_POINT('Ctrl Pts',(4.07426172299847,-1.,0.526740277227498));
#35902=CARTESIAN_POINT('Ctrl Pts',(4.08088789536836,-1.,0.530769518728571));
#35903=CARTESIAN_POINT('Ctrl Pts',(4.08750259988885,-1.,0.534833963477273));
#35904=CARTESIAN_POINT('Ctrl Pts',(4.09410597627,-1.,0.538933321179756));
#35905=CARTESIAN_POINT('Ctrl Pts',(4.10069810243979,-1.,0.543067286877758));
#35906=CARTESIAN_POINT('Ctrl Pts',(4.10727897027977,-1.,0.547235539485637));
#35907=CARTESIAN_POINT('Ctrl Pts',(4.11384852024721,-1.,0.551437758497033));
#35908=CARTESIAN_POINT('Ctrl Pts',(4.12040666195664,-1.,0.555673636129978));
#35909=CARTESIAN_POINT('Ctrl Pts',(4.12695329951961,-1.,0.559942890594774));
#35910=CARTESIAN_POINT('Ctrl Pts',(4.13348835727104,-1.,0.564245279537149));
#35911=CARTESIAN_POINT('Ctrl Pts',(4.14001179830547,-1.,0.568580610189775));
#35912=CARTESIAN_POINT('Ctrl Pts',(4.14652361068081,-1.,0.572948736069523));
#35913=CARTESIAN_POINT('Ctrl Pts',(4.151723761217,-1.,0.576469391676689));
#35914=CARTESIAN_POINT('Ctrl Pts',(4.15561864788576,-1.,0.579124568914236));
#35915=CARTESIAN_POINT('Ctrl Pts',(4.1582129171283,-1.,0.580901211463535));
#35916=CARTESIAN_POINT('Ctrl Pts',(4.15950947128175,-1.,0.581791163835816));
#35917=CARTESIAN_POINT('',(4.13571194405636,-1.,0.732042837400621));
#35918=CARTESIAN_POINT('',(4.15950947128175,-1.,0.581791163835816));
#35919=CARTESIAN_POINT('Ctrl Pts',(4.13571194405636,-1.,0.732042837400621));
#35920=CARTESIAN_POINT('Ctrl Pts',(4.1342038373684,-1.,0.73248857513516));
#35921=CARTESIAN_POINT('Ctrl Pts',(4.13118752795207,-1.,0.733376589323547));
#35922=CARTESIAN_POINT('Ctrl Pts',(4.12666277570844,-1.,0.734698226764093));
#35923=CARTESIAN_POINT('Ctrl Pts',(4.120629196238,-1.,0.736439634331345));
#35924=CARTESIAN_POINT('Ctrl Pts',(4.11308626951927,-1.,0.738581708225844));
#35925=CARTESIAN_POINT('Ctrl Pts',(4.10554241757547,-1.,0.740688998553377));
#35926=CARTESIAN_POINT('Ctrl Pts',(4.09799769702611,-1.,0.742761369689842));
#35927=CARTESIAN_POINT('Ctrl Pts',(4.09045220253573,-1.,0.744798649706501));
#35928=CARTESIAN_POINT('Ctrl Pts',(4.08290608095642,-1.,0.746800631492316));
#35929=CARTESIAN_POINT('Ctrl Pts',(4.07535951056152,-1.,0.748767076680558));
#35930=CARTESIAN_POINT('Ctrl Pts',(4.06781267242378,-1.,0.750697720484037));
#35931=CARTESIAN_POINT('Ctrl Pts',(4.06026572221515,-1.,0.752592276483073));
#35932=CARTESIAN_POINT('Ctrl Pts',(4.05271876687915,-1.,0.754450441816078));
#35933=CARTESIAN_POINT('Ctrl Pts',(4.04517182653997,-1.,0.756271902369581));
#35934=CARTESIAN_POINT('Ctrl Pts',(4.03762485803119,-1.,0.758056338884945));
#35935=CARTESIAN_POINT('Ctrl Pts',(4.03007781954412,-1.,0.759803433243752));
#35936=CARTESIAN_POINT('Ctrl Pts',(4.02253072741268,-1.,0.761512875859805));
#35937=CARTESIAN_POINT('Ctrl Pts',(4.01498370680496,-1.,0.763184371182936));
#35938=CARTESIAN_POINT('Ctrl Pts',(4.00743706791509,-1.,0.764817648785198));
#35939=CARTESIAN_POINT('Ctrl Pts',(3.99989129179622,-1.,0.766412457136064));
#35940=CARTESIAN_POINT('Ctrl Pts',(3.9923468788101,-1.,0.767968531377915));
#35941=CARTESIAN_POINT('Ctrl Pts',(3.98480422348451,-1.,0.769485566245545));
#35942=CARTESIAN_POINT('Ctrl Pts',(3.97726349165488,-1.,0.770963190030471));
#35943=CARTESIAN_POINT('Ctrl Pts',(3.96972446532772,-1.,0.772400931772137));
#35944=CARTESIAN_POINT('Ctrl Pts',(3.96218649639807,-1.,0.773798212026566));
#35945=CARTESIAN_POINT('Ctrl Pts',(3.9546488545231,-1.,0.775154418039352));
#35946=CARTESIAN_POINT('Ctrl Pts',(3.94711101619447,-1.,0.776468966697922));
#35947=CARTESIAN_POINT('Ctrl Pts',(3.93957296768103,-1.,0.777741370568559));
#35948=CARTESIAN_POINT('Ctrl Pts',(3.93203552473174,-1.,0.778971308134821));
#35949=CARTESIAN_POINT('Ctrl Pts',(3.92450058323823,-1.,0.780158678615543));
#35950=CARTESIAN_POINT('Ctrl Pts',(3.91697036054676,-1.,0.781303428618367));
#35951=CARTESIAN_POINT('Ctrl Pts',(3.90944671004542,-1.,0.782405395622765));
#35952=CARTESIAN_POINT('Ctrl Pts',(3.9019303904397,-1.,0.783464141529082));
#35953=CARTESIAN_POINT('Ctrl Pts',(3.89442039235103,-1.,0.784478799358337));
#35954=CARTESIAN_POINT('Ctrl Pts',(3.88691313167398,-1.,0.785447890340731));
#35955=CARTESIAN_POINT('Ctrl Pts',(3.8794040281819,-1.,0.786369675812609));
#35956=CARTESIAN_POINT('Ctrl Pts',(3.87188916600912,-1.,0.787242527617999));
#35957=CARTESIAN_POINT('Ctrl Pts',(3.86436702561345,-1.,0.788065315093778));
#35958=CARTESIAN_POINT('Ctrl Pts',(3.85683995872529,-1.,0.788837734090672));
#35959=CARTESIAN_POINT('Ctrl Pts',(3.84931637808894,-1.,0.789560798155583));
#35960=CARTESIAN_POINT('Ctrl Pts',(3.84180762342454,-1.,0.790236124191243));
#35961=CARTESIAN_POINT('Ctrl Pts',(3.83432392054786,-1.,0.790865012705301));
#35962=CARTESIAN_POINT('Ctrl Pts',(3.82687033899792,-1.,0.791447528662369));
#35963=CARTESIAN_POINT('Ctrl Pts',(3.81944345442249,-1.,0.791981740718635));
#35964=CARTESIAN_POINT('Ctrl Pts',(3.81202588694756,-1.,0.792462483517635));
#35965=CARTESIAN_POINT('Ctrl Pts',(3.80459229925637,-1.,0.792882695234778));
#35966=CARTESIAN_POINT('Ctrl Pts',(3.79711921389897,-1.,0.793235612973274));
#35967=CARTESIAN_POINT('Ctrl Pts',(3.78959439439235,-1.,0.793516871680994));
#35968=CARTESIAN_POINT('Ctrl Pts',(3.78202460377598,-1.,0.793726235781301));
#35969=CARTESIAN_POINT('Ctrl Pts',(3.77444863801212,-1.,0.793870523787408));
#35970=CARTESIAN_POINT('Ctrl Pts',(3.76692626931111,-1.,0.793961083688992));
#35971=CARTESIAN_POINT('Ctrl Pts',(3.75951468666257,-1.,0.794008429134908));
#35972=CARTESIAN_POINT('Ctrl Pts',(3.75224692493864,-1.,0.794017347371378));
#35973=CARTESIAN_POINT('Ctrl Pts',(3.74511357728861,-1.,0.793982700459952));
#35974=CARTESIAN_POINT('Ctrl Pts',(3.73803280541687,-1.,0.793882700937017));
#35975=CARTESIAN_POINT('Ctrl Pts',(3.73086914695805,-1.,0.793682750269684));
#35976=CARTESIAN_POINT('Ctrl Pts',(3.72348797293734,-1.,0.793347023784205));
#35977=CARTESIAN_POINT('Ctrl Pts',(3.71580242396124,-1.,0.792848377370287));
#35978=CARTESIAN_POINT('Ctrl Pts',(3.70781724021806,-1.,0.792177688845818));
#35979=CARTESIAN_POINT('Ctrl Pts',(3.69968940808721,-1.,0.79135657569598));
#35980=CARTESIAN_POINT('Ctrl Pts',(3.69172044327364,-1.,0.790436284988788));
#35981=CARTESIAN_POINT('Ctrl Pts',(3.68428439783905,-1.,0.789483546064387));
#35982=CARTESIAN_POINT('Ctrl Pts',(3.67777119516252,-1.,0.788569566220286));
#35983=CARTESIAN_POINT('Ctrl Pts',(3.67252923663655,-1.,0.787758799995743));
#35984=CARTESIAN_POINT('Ctrl Pts',(3.66907505398677,-1.,0.787145041181546));
#35985=CARTESIAN_POINT('Ctrl Pts',(3.66743103898702,-1.,0.786774337198063));
#35986=CARTESIAN_POINT('Ctrl Pts',(3.66680946938292,-1.,0.786565919558984));
#35987=CARTESIAN_POINT('Ctrl Pts',(3.6666431041522,-1.,0.786459983895432));
#35988=CARTESIAN_POINT('Ctrl Pts',(3.66661143271685,-1.,0.786422660831985));
#35989=CARTESIAN_POINT('Origin',(0.,-1.,0.));
#35990=CARTESIAN_POINT('Origin',(0.,0.,0.));
#35991=CARTESIAN_POINT('Origin',(0.,2.2,0.));
#35992=CARTESIAN_POINT('Origin',(0.,1.,0.));
#35993=CARTESIAN_POINT('',(-2.,2.2,2.44929359829471E-16));
#35994=CARTESIAN_POINT('Origin',(0.,2.2,0.));
#35995=CARTESIAN_POINT('',(-2.,1.,2.44929359829471E-16));
#35996=CARTESIAN_POINT('',(-2.,1.,2.44929359829471E-16));
#35997=CARTESIAN_POINT('Origin',(0.,1.,0.));
#35998=CARTESIAN_POINT('Origin',(0.,2.2,0.));
#35999=CARTESIAN_POINT('Ctrl Pts',(4.15950947128175,-1.,0.581791163835816));
#36000=CARTESIAN_POINT('Ctrl Pts',(4.15950947128175,1.,0.581791163835816));
#36001=CARTESIAN_POINT('Ctrl Pts',(4.1582129171283,-1.,0.580901211463535));
#36002=CARTESIAN_POINT('Ctrl Pts',(4.1582129171283,1.,0.580901211463535));
#36003=CARTESIAN_POINT('Ctrl Pts',(4.15561864788576,-1.,0.579124568914236));
#36004=CARTESIAN_POINT('Ctrl Pts',(4.15561864788576,1.,0.579124568914236));
#36005=CARTESIAN_POINT('Ctrl Pts',(4.151723761217,-1.,0.576469391676689));
#36006=CARTESIAN_POINT('Ctrl Pts',(4.151723761217,1.,0.576469391676689));
#36007=CARTESIAN_POINT('Ctrl Pts',(4.14652361068081,-1.,0.572948736069523));
#36008=CARTESIAN_POINT('Ctrl Pts',(4.14652361068081,1.,0.572948736069523));
#36009=CARTESIAN_POINT('Ctrl Pts',(4.14001179830547,-1.,0.568580610189775));
#36010=CARTESIAN_POINT('Ctrl Pts',(4.14001179830547,1.,0.568580610189775));
#36011=CARTESIAN_POINT('Ctrl Pts',(4.13348835727104,-1.,0.564245279537149));
#36012=CARTESIAN_POINT('Ctrl Pts',(4.13348835727104,1.,0.564245279537149));
#36013=CARTESIAN_POINT('Ctrl Pts',(4.12695329951961,-1.,0.559942890594774));
#36014=CARTESIAN_POINT('Ctrl Pts',(4.12695329951961,1.,0.559942890594774));
#36015=CARTESIAN_POINT('Ctrl Pts',(4.12040666195664,-1.,0.555673636129978));
#36016=CARTESIAN_POINT('Ctrl Pts',(4.12040666195664,1.,0.555673636129978));
#36017=CARTESIAN_POINT('Ctrl Pts',(4.11384852024721,-1.,0.551437758497033));
#36018=CARTESIAN_POINT('Ctrl Pts',(4.11384852024721,1.,0.551437758497033));
#36019=CARTESIAN_POINT('Ctrl Pts',(4.10727897027977,-1.,0.547235539485637));
#36020=CARTESIAN_POINT('Ctrl Pts',(4.10727897027977,1.,0.547235539485637));
#36021=CARTESIAN_POINT('Ctrl Pts',(4.10069810243979,-1.,0.543067286877758));
#36022=CARTESIAN_POINT('Ctrl Pts',(4.10069810243979,1.,0.543067286877758));
#36023=CARTESIAN_POINT('Ctrl Pts',(4.09410597627,-1.,0.538933321179756));
#36024=CARTESIAN_POINT('Ctrl Pts',(4.09410597627,1.,0.538933321179756));
#36025=CARTESIAN_POINT('Ctrl Pts',(4.08750259988885,-1.,0.534833963477273));
#36026=CARTESIAN_POINT('Ctrl Pts',(4.08750259988885,1.,0.534833963477273));
#36027=CARTESIAN_POINT('Ctrl Pts',(4.08088789536836,-1.,0.530769518728571));
#36028=CARTESIAN_POINT('Ctrl Pts',(4.08088789536836,1.,0.530769518728571));
#36029=CARTESIAN_POINT('Ctrl Pts',(4.07426172299847,-1.,0.526740277227498));
#36030=CARTESIAN_POINT('Ctrl Pts',(4.07426172299847,1.,0.526740277227498));
#36031=CARTESIAN_POINT('Ctrl Pts',(4.06762394471314,-1.,0.522746528603108));
#36032=CARTESIAN_POINT('Ctrl Pts',(4.06762394471314,1.,0.522746528603108));
#36033=CARTESIAN_POINT('Ctrl Pts',(4.06097448038013,-1.,0.518788572336924));
#36034=CARTESIAN_POINT('Ctrl Pts',(4.06097448038013,1.,0.518788572336924));
#36035=CARTESIAN_POINT('Ctrl Pts',(4.05431335771199,-1.,0.514866728193017));
#36036=CARTESIAN_POINT('Ctrl Pts',(4.05431335771199,1.,0.514866728193017));
#36037=CARTESIAN_POINT('Ctrl Pts',(4.04764078815447,-1.,0.510981349218971));
#36038=CARTESIAN_POINT('Ctrl Pts',(4.04764078815447,1.,0.510981349218971));
#36039=CARTESIAN_POINT('Ctrl Pts',(4.04095715148915,-1.,0.507132823288137));
#36040=CARTESIAN_POINT('Ctrl Pts',(4.04095715148915,1.,0.507132823288137));
#36041=CARTESIAN_POINT('Ctrl Pts',(4.03426284174272,-1.,0.503321556915346));
#36042=CARTESIAN_POINT('Ctrl Pts',(4.03426284174272,1.,0.503321556915346));
#36043=CARTESIAN_POINT('Ctrl Pts',(4.02755813980101,-1.,0.499547962340822));
#36044=CARTESIAN_POINT('Ctrl Pts',(4.02755813980101,1.,0.499547962340822));
#36045=CARTESIAN_POINT('Ctrl Pts',(4.02084308851832,-1.,0.495812444326251));
#36046=CARTESIAN_POINT('Ctrl Pts',(4.02084308851832,1.,0.495812444326251));
#36047=CARTESIAN_POINT('Ctrl Pts',(4.01411733503546,-1.,0.492115383418019));
#36048=CARTESIAN_POINT('Ctrl Pts',(4.01411733503546,1.,0.492115383418019));
#36049=CARTESIAN_POINT('Ctrl Pts',(4.0073800839099,-1.,0.488457130424634));
#36050=CARTESIAN_POINT('Ctrl Pts',(4.0073800839099,1.,0.488457130424634));
#36051=CARTESIAN_POINT('Ctrl Pts',(4.00063045119288,-1.,0.484838042421835));
#36052=CARTESIAN_POINT('Ctrl Pts',(4.00063045119288,1.,0.484838042421835));
#36053=CARTESIAN_POINT('Ctrl Pts',(3.99386775880679,-1.,0.481258512209676));
#36054=CARTESIAN_POINT('Ctrl Pts',(3.99386775880679,1.,0.481258512209676));
#36055=CARTESIAN_POINT('Ctrl Pts',(3.98709184306738,-1.,0.477718999122028));
#36056=CARTESIAN_POINT('Ctrl Pts',(3.98709184306738,1.,0.477718999122028));
#36057=CARTESIAN_POINT('Ctrl Pts',(3.98030338044409,-1.,0.47422006101951));
#36058=CARTESIAN_POINT('Ctrl Pts',(3.98030338044409,1.,0.47422006101951));
#36059=CARTESIAN_POINT('Ctrl Pts',(3.97350414289392,-1.,0.47076237961344));
#36060=CARTESIAN_POINT('Ctrl Pts',(3.97350414289392,1.,0.47076237961344));
#36061=CARTESIAN_POINT('Ctrl Pts',(3.9666962227393,-1.,0.467346690880644));
#36062=CARTESIAN_POINT('Ctrl Pts',(3.9666962227393,1.,0.467346690880644));
#36063=CARTESIAN_POINT('Ctrl Pts',(3.95988133243538,-1.,0.463973722115734));
#36064=CARTESIAN_POINT('Ctrl Pts',(3.95988133243538,1.,0.463973722115734));
#36065=CARTESIAN_POINT('Ctrl Pts',(3.95306005817364,-1.,0.460644124429122));
#36066=CARTESIAN_POINT('Ctrl Pts',(3.95306005817364,1.,0.460644124429122));
#36067=CARTESIAN_POINT('Ctrl Pts',(3.94623117206678,-1.,0.457358410451683));
#36068=CARTESIAN_POINT('Ctrl Pts',(3.94623117206678,1.,0.457358410451683));
#36069=CARTESIAN_POINT('Ctrl Pts',(3.93939080846298,-1.,0.454116879027584));
#36070=CARTESIAN_POINT('Ctrl Pts',(3.93939080846298,1.,0.454116879027584));
#36071=CARTESIAN_POINT('Ctrl Pts',(3.93253407403123,-1.,0.450919768356349));
#36072=CARTESIAN_POINT('Ctrl Pts',(3.93253407403123,1.,0.450919768356349));
#36073=CARTESIAN_POINT('Ctrl Pts',(3.92565674143416,-1.,0.447767416837293));
#36074=CARTESIAN_POINT('Ctrl Pts',(3.92565674143416,1.,0.447767416837293));
#36075=CARTESIAN_POINT('Ctrl Pts',(3.91875701610719,-1.,0.444660430230591));
#36076=CARTESIAN_POINT('Ctrl Pts',(3.91875701610719,1.,0.444660430230591));
#36077=CARTESIAN_POINT('Ctrl Pts',(3.91183704069153,-1.,0.441599824524055));
#36078=CARTESIAN_POINT('Ctrl Pts',(3.91183704069153,1.,0.441599824524055));
#36079=CARTESIAN_POINT('Ctrl Pts',(3.90490512938563,-1.,0.43858723545825));
#36080=CARTESIAN_POINT('Ctrl Pts',(3.90490512938563,1.,0.43858723545825));
#36081=CARTESIAN_POINT('Ctrl Pts',(3.89797256655462,-1.,0.435624629433528));
#36082=CARTESIAN_POINT('Ctrl Pts',(3.89797256655462,1.,0.435624629433528));
#36083=CARTESIAN_POINT('Ctrl Pts',(3.89104947940611,-1.,0.432713929544459));
#36084=CARTESIAN_POINT('Ctrl Pts',(3.89104947940611,1.,0.432713929544459));
#36085=CARTESIAN_POINT('Ctrl Pts',(3.88414070943341,-1.,0.429856640579741));
#36086=CARTESIAN_POINT('Ctrl Pts',(3.88414070943341,1.,0.429856640579741));
#36087=CARTESIAN_POINT('Ctrl Pts',(3.87724240306597,-1.,0.427053541173458));
#36088=CARTESIAN_POINT('Ctrl Pts',(3.87724240306597,1.,0.427053541173458));
#36089=CARTESIAN_POINT('Ctrl Pts',(3.87033643487851,-1.,0.424304173195111));
#36090=CARTESIAN_POINT('Ctrl Pts',(3.87033643487851,1.,0.424304173195111));
#36091=CARTESIAN_POINT('Ctrl Pts',(3.86339652542709,-1.,0.421607423177534));
#36092=CARTESIAN_POINT('Ctrl Pts',(3.86339652542709,1.,0.421607423177534));
#36093=CARTESIAN_POINT('Ctrl Pts',(3.85639825647996,-1.,0.418962468086773));
#36094=CARTESIAN_POINT('Ctrl Pts',(3.85639825647996,1.,0.418962468086773));
#36095=CARTESIAN_POINT('Ctrl Pts',(3.84932864157497,-1.,0.416369678052907));
#36096=CARTESIAN_POINT('Ctrl Pts',(3.84932864157497,1.,0.416369678052907));
#36097=CARTESIAN_POINT('Ctrl Pts',(3.84219403994762,-1.,0.413831367016748));
#36098=CARTESIAN_POINT('Ctrl Pts',(3.84219403994762,1.,0.413831367016748));
#36099=CARTESIAN_POINT('Ctrl Pts',(3.83503345578698,-1.,0.411353038798519));
#36100=CARTESIAN_POINT('Ctrl Pts',(3.83503345578698,1.,0.411353038798519));
#36101=CARTESIAN_POINT('Ctrl Pts',(3.82790724256471,-1.,0.40894237144746));
#36102=CARTESIAN_POINT('Ctrl Pts',(3.82790724256471,1.,0.40894237144746));
#36103=CARTESIAN_POINT('Ctrl Pts',(3.8208730391381,-1.,0.406607038258986));
#36104=CARTESIAN_POINT('Ctrl Pts',(3.8208730391381,1.,0.406607038258986));
#36105=CARTESIAN_POINT('Ctrl Pts',(3.81396374287793,-1.,0.404352694628274));
#36106=CARTESIAN_POINT('Ctrl Pts',(3.81396374287793,1.,0.404352694628274));
#36107=CARTESIAN_POINT('Ctrl Pts',(3.80716881962728,-1.,0.402181320148436));
#36108=CARTESIAN_POINT('Ctrl Pts',(3.80716881962728,1.,0.402181320148436));
#36109=CARTESIAN_POINT('Ctrl Pts',(3.80040370384546,-1.,0.400088346504601));
#36110=CARTESIAN_POINT('Ctrl Pts',(3.80040370384546,1.,0.400088346504601));
#36111=CARTESIAN_POINT('Ctrl Pts',(3.7935288716329,-1.,0.39806481868397));
#36112=CARTESIAN_POINT('Ctrl Pts',(3.7935288716329,1.,0.39806481868397));
#36113=CARTESIAN_POINT('Ctrl Pts',(3.78640521279313,-1.,0.396103205334841));
#36114=CARTESIAN_POINT('Ctrl Pts',(3.78640521279313,1.,0.396103205334841));
#36115=CARTESIAN_POINT('Ctrl Pts',(3.77894173114283,-1.,0.3942024810115));
#36116=CARTESIAN_POINT('Ctrl Pts',(3.77894173114283,1.,0.3942024810115));
#36117=CARTESIAN_POINT('Ctrl Pts',(3.77114011595967,-1.,0.392372786223433));
#36118=CARTESIAN_POINT('Ctrl Pts',(3.77114011595967,1.,0.392372786223433));
#36119=CARTESIAN_POINT('Ctrl Pts',(3.76315635033257,-1.,0.39064207297956));
#36120=CARTESIAN_POINT('Ctrl Pts',(3.76315635033257,1.,0.39064207297956));
#36121=CARTESIAN_POINT('Ctrl Pts',(3.75529302895152,-1.,0.389054775898702));
#36122=CARTESIAN_POINT('Ctrl Pts',(3.75529302895152,1.,0.389054775898702));
#36123=CARTESIAN_POINT('Ctrl Pts',(3.74792651696654,-1.,0.387663020050836));
#36124=CARTESIAN_POINT('Ctrl Pts',(3.74792651696654,1.,0.387663020050836));
#36125=CARTESIAN_POINT('Ctrl Pts',(3.74144965781276,-1.,0.386519576222252));
#36126=CARTESIAN_POINT('Ctrl Pts',(3.74144965781276,1.,0.386519576222252));
#36127=CARTESIAN_POINT('Ctrl Pts',(3.73621371845318,-1.,0.385670806454566));
#36128=CARTESIAN_POINT('Ctrl Pts',(3.73621371845318,1.,0.385670806454566));
#36129=CARTESIAN_POINT('Ctrl Pts',(3.73245705638843,-1.,0.385147887988952));
#36130=CARTESIAN_POINT('Ctrl Pts',(3.73245705638843,1.,0.385147887988952));
#36131=CARTESIAN_POINT('Ctrl Pts',(3.73072465900175,-1.,0.385001870183213));
#36132=CARTESIAN_POINT('Ctrl Pts',(3.73072465900175,1.,0.385001870183213));
#36133=CARTESIAN_POINT('Ctrl Pts',(3.73015851028356,-1.,0.385047711603463));
#36134=CARTESIAN_POINT('Ctrl Pts',(3.73015851028356,1.,0.385047711603463));
#36135=CARTESIAN_POINT('Ctrl Pts',(3.73010668803042,-1.,0.385147278814643));
#36136=CARTESIAN_POINT('Ctrl Pts',(3.73010668803042,1.,0.385147278814643));
#36137=CARTESIAN_POINT('Ctrl Pts',(3.73016218570874,-1.,0.38521431477633));
#36138=CARTESIAN_POINT('Ctrl Pts',(3.73016218570874,1.,0.38521431477633));
#36139=CARTESIAN_POINT('',(3.73017266276651,1.,0.385112848330762));
#36140=CARTESIAN_POINT('Ctrl Pts',(3.73017266276651,1.,0.385112848330762));
#36141=CARTESIAN_POINT('Ctrl Pts',(3.73017266276651,0.666666666666667,0.385112848330762));
#36142=CARTESIAN_POINT('Ctrl Pts',(3.73017266276651,0.333333333333333,0.385112848330762));
#36143=CARTESIAN_POINT('Ctrl Pts',(3.73017266276651,-0.333333333333333,
0.385112848330762));
#36144=CARTESIAN_POINT('Ctrl Pts',(3.73017266276651,-0.666666666666667,
0.385112848330763));
#36145=CARTESIAN_POINT('Ctrl Pts',(3.73017266276651,-1.,0.385112848330763));
#36146=CARTESIAN_POINT('',(4.15950947128175,1.,0.581791163835816));
#36147=CARTESIAN_POINT('Ctrl Pts',(4.15950947128175,1.,0.581791163835816));
#36148=CARTESIAN_POINT('Ctrl Pts',(4.1582129171283,1.,0.580901211463535));
#36149=CARTESIAN_POINT('Ctrl Pts',(4.15561864788576,1.,0.579124568914236));
#36150=CARTESIAN_POINT('Ctrl Pts',(4.151723761217,1.,0.576469391676689));
#36151=CARTESIAN_POINT('Ctrl Pts',(4.14652361068081,1.,0.572948736069523));
#36152=CARTESIAN_POINT('Ctrl Pts',(4.14001179830547,1.,0.568580610189775));
#36153=CARTESIAN_POINT('Ctrl Pts',(4.13348835727104,1.,0.564245279537149));
#36154=CARTESIAN_POINT('Ctrl Pts',(4.12695329951961,1.,0.559942890594774));
#36155=CARTESIAN_POINT('Ctrl Pts',(4.12040666195664,1.,0.555673636129978));
#36156=CARTESIAN_POINT('Ctrl Pts',(4.11384852024721,1.,0.551437758497033));
#36157=CARTESIAN_POINT('Ctrl Pts',(4.10727897027977,1.,0.547235539485637));
#36158=CARTESIAN_POINT('Ctrl Pts',(4.10069810243979,1.,0.543067286877758));
#36159=CARTESIAN_POINT('Ctrl Pts',(4.09410597627,1.,0.538933321179756));
#36160=CARTESIAN_POINT('Ctrl Pts',(4.08750259988885,1.,0.534833963477273));
#36161=CARTESIAN_POINT('Ctrl Pts',(4.08088789536836,1.,0.530769518728571));
#36162=CARTESIAN_POINT('Ctrl Pts',(4.07426172299847,1.,0.526740277227498));
#36163=CARTESIAN_POINT('Ctrl Pts',(4.06762394471314,1.,0.522746528603108));
#36164=CARTESIAN_POINT('Ctrl Pts',(4.06097448038013,1.,0.518788572336924));
#36165=CARTESIAN_POINT('Ctrl Pts',(4.05431335771199,1.,0.514866728193017));
#36166=CARTESIAN_POINT('Ctrl Pts',(4.04764078815447,1.,0.510981349218971));
#36167=CARTESIAN_POINT('Ctrl Pts',(4.04095715148915,1.,0.507132823288137));
#36168=CARTESIAN_POINT('Ctrl Pts',(4.03426284174272,1.,0.503321556915346));
#36169=CARTESIAN_POINT('Ctrl Pts',(4.02755813980101,1.,0.499547962340822));
#36170=CARTESIAN_POINT('Ctrl Pts',(4.02084308851832,1.,0.495812444326251));
#36171=CARTESIAN_POINT('Ctrl Pts',(4.01411733503546,1.,0.492115383418019));
#36172=CARTESIAN_POINT('Ctrl Pts',(4.0073800839099,1.,0.488457130424634));
#36173=CARTESIAN_POINT('Ctrl Pts',(4.00063045119288,1.,0.484838042421835));
#36174=CARTESIAN_POINT('Ctrl Pts',(3.99386775880679,1.,0.481258512209676));
#36175=CARTESIAN_POINT('Ctrl Pts',(3.98709184306738,1.,0.477718999122028));
#36176=CARTESIAN_POINT('Ctrl Pts',(3.98030338044409,1.,0.47422006101951));
#36177=CARTESIAN_POINT('Ctrl Pts',(3.97350414289392,1.,0.47076237961344));
#36178=CARTESIAN_POINT('Ctrl Pts',(3.9666962227393,1.,0.467346690880644));
#36179=CARTESIAN_POINT('Ctrl Pts',(3.95988133243538,1.,0.463973722115734));
#36180=CARTESIAN_POINT('Ctrl Pts',(3.95306005817364,1.,0.460644124429122));
#36181=CARTESIAN_POINT('Ctrl Pts',(3.94623117206678,1.,0.457358410451683));
#36182=CARTESIAN_POINT('Ctrl Pts',(3.93939080846298,1.,0.454116879027584));
#36183=CARTESIAN_POINT('Ctrl Pts',(3.93253407403123,1.,0.450919768356349));
#36184=CARTESIAN_POINT('Ctrl Pts',(3.92565674143416,1.,0.447767416837293));
#36185=CARTESIAN_POINT('Ctrl Pts',(3.91875701610719,1.,0.444660430230591));
#36186=CARTESIAN_POINT('Ctrl Pts',(3.91183704069153,1.,0.441599824524055));
#36187=CARTESIAN_POINT('Ctrl Pts',(3.90490512938563,1.,0.43858723545825));
#36188=CARTESIAN_POINT('Ctrl Pts',(3.89797256655462,1.,0.435624629433528));
#36189=CARTESIAN_POINT('Ctrl Pts',(3.89104947940611,1.,0.432713929544459));
#36190=CARTESIAN_POINT('Ctrl Pts',(3.88414070943341,1.,0.429856640579741));
#36191=CARTESIAN_POINT('Ctrl Pts',(3.87724240306597,1.,0.427053541173458));
#36192=CARTESIAN_POINT('Ctrl Pts',(3.87033643487851,1.,0.424304173195111));
#36193=CARTESIAN_POINT('Ctrl Pts',(3.86339652542709,1.,0.421607423177534));
#36194=CARTESIAN_POINT('Ctrl Pts',(3.85639825647996,1.,0.418962468086773));
#36195=CARTESIAN_POINT('Ctrl Pts',(3.84932864157497,1.,0.416369678052907));
#36196=CARTESIAN_POINT('Ctrl Pts',(3.84219403994762,1.,0.413831367016748));
#36197=CARTESIAN_POINT('Ctrl Pts',(3.83503345578698,1.,0.411353038798519));
#36198=CARTESIAN_POINT('Ctrl Pts',(3.82790724256471,1.,0.40894237144746));
#36199=CARTESIAN_POINT('Ctrl Pts',(3.8208730391381,1.,0.406607038258986));
#36200=CARTESIAN_POINT('Ctrl Pts',(3.81396374287793,1.,0.404352694628274));
#36201=CARTESIAN_POINT('Ctrl Pts',(3.80716881962728,1.,0.402181320148436));
#36202=CARTESIAN_POINT('Ctrl Pts',(3.80040370384546,1.,0.400088346504601));
#36203=CARTESIAN_POINT('Ctrl Pts',(3.7935288716329,1.,0.39806481868397));
#36204=CARTESIAN_POINT('Ctrl Pts',(3.78640521279313,1.,0.396103205334841));
#36205=CARTESIAN_POINT('Ctrl Pts',(3.77894173114283,1.,0.3942024810115));
#36206=CARTESIAN_POINT('Ctrl Pts',(3.77114011595967,1.,0.392372786223433));
#36207=CARTESIAN_POINT('Ctrl Pts',(3.76315635033257,1.,0.39064207297956));
#36208=CARTESIAN_POINT('Ctrl Pts',(3.75529302895152,1.,0.389054775898702));
#36209=CARTESIAN_POINT('Ctrl Pts',(3.74792651696654,1.,0.387663020050836));
#36210=CARTESIAN_POINT('Ctrl Pts',(3.74144965781276,1.,0.386519576222252));
#36211=CARTESIAN_POINT('Ctrl Pts',(3.73621371845318,1.,0.385670806454566));
#36212=CARTESIAN_POINT('Ctrl Pts',(3.73273893363406,1.,0.385187124634207));
#36213=CARTESIAN_POINT('Ctrl Pts',(3.73106082862548,1.,0.385031656499164));
#36214=CARTESIAN_POINT('Ctrl Pts',(3.73040527621055,1.,0.385037797881504));
#36215=CARTESIAN_POINT('Ctrl Pts',(3.73021431755274,1.,0.385087139000375));
#36216=CARTESIAN_POINT('Ctrl Pts',(3.73017266276651,1.,0.385112848330762));
#36217=CARTESIAN_POINT('',(4.15950947128175,0.,0.581791163835816));
#36218=CARTESIAN_POINT('Ctrl Pts',(3.66663282329846,-1.,0.7863229229206));
#36219=CARTESIAN_POINT('Ctrl Pts',(3.66663282329846,1.,0.7863229229206));
#36220=CARTESIAN_POINT('Ctrl Pts',(3.66655932661986,-1.,0.786369528183326));
#36221=CARTESIAN_POINT('Ctrl Pts',(3.66655932661986,1.,0.786369528183326));
#36222=CARTESIAN_POINT('Ctrl Pts',(3.66657784455334,-1.,0.786480236185697));
#36223=CARTESIAN_POINT('Ctrl Pts',(3.66657784455334,1.,0.786480236185697));
#36224=CARTESIAN_POINT('Ctrl Pts',(3.66710211820482,-1.,0.786698783542764));
#36225=CARTESIAN_POINT('Ctrl Pts',(3.66710211820482,1.,0.786698783542764));
#36226=CARTESIAN_POINT('Ctrl Pts',(3.66879484801113,-1.,0.787095252590501));
#36227=CARTESIAN_POINT('Ctrl Pts',(3.66879484801113,1.,0.787095252590501));
#36228=CARTESIAN_POINT('Ctrl Pts',(3.67252923663655,-1.,0.787758799995743));
#36229=CARTESIAN_POINT('Ctrl Pts',(3.67252923663655,1.,0.787758799995743));
#36230=CARTESIAN_POINT('Ctrl Pts',(3.67777119516252,-1.,0.788569566220286));
#36231=CARTESIAN_POINT('Ctrl Pts',(3.67777119516252,1.,0.788569566220286));
#36232=CARTESIAN_POINT('Ctrl Pts',(3.68428439783905,-1.,0.789483546064387));
#36233=CARTESIAN_POINT('Ctrl Pts',(3.68428439783905,1.,0.789483546064387));
#36234=CARTESIAN_POINT('Ctrl Pts',(3.69172044327364,-1.,0.790436284988788));
#36235=CARTESIAN_POINT('Ctrl Pts',(3.69172044327364,1.,0.790436284988788));
#36236=CARTESIAN_POINT('Ctrl Pts',(3.69968940808721,-1.,0.79135657569598));
#36237=CARTESIAN_POINT('Ctrl Pts',(3.69968940808721,1.,0.79135657569598));
#36238=CARTESIAN_POINT('Ctrl Pts',(3.70781724021806,-1.,0.792177688845818));
#36239=CARTESIAN_POINT('Ctrl Pts',(3.70781724021806,1.,0.792177688845818));
#36240=CARTESIAN_POINT('Ctrl Pts',(3.71580242396124,-1.,0.792848377370287));
#36241=CARTESIAN_POINT('Ctrl Pts',(3.71580242396124,1.,0.792848377370287));
#36242=CARTESIAN_POINT('Ctrl Pts',(3.72348797293734,-1.,0.793347023784205));
#36243=CARTESIAN_POINT('Ctrl Pts',(3.72348797293734,1.,0.793347023784205));
#36244=CARTESIAN_POINT('Ctrl Pts',(3.73086914695805,-1.,0.793682750269684));
#36245=CARTESIAN_POINT('Ctrl Pts',(3.73086914695805,1.,0.793682750269684));
#36246=CARTESIAN_POINT('Ctrl Pts',(3.73803280541687,-1.,0.793882700937017));
#36247=CARTESIAN_POINT('Ctrl Pts',(3.73803280541687,1.,0.793882700937017));
#36248=CARTESIAN_POINT('Ctrl Pts',(3.74511357728861,-1.,0.793982700459952));
#36249=CARTESIAN_POINT('Ctrl Pts',(3.74511357728861,1.,0.793982700459952));
#36250=CARTESIAN_POINT('Ctrl Pts',(3.75224692493864,-1.,0.794017347371378));
#36251=CARTESIAN_POINT('Ctrl Pts',(3.75224692493864,1.,0.794017347371378));
#36252=CARTESIAN_POINT('Ctrl Pts',(3.75951468666257,-1.,0.794008429134908));
#36253=CARTESIAN_POINT('Ctrl Pts',(3.75951468666257,1.,0.794008429134908));
#36254=CARTESIAN_POINT('Ctrl Pts',(3.76692626931111,-1.,0.793961083688992));
#36255=CARTESIAN_POINT('Ctrl Pts',(3.76692626931111,1.,0.793961083688992));
#36256=CARTESIAN_POINT('Ctrl Pts',(3.77444863801212,-1.,0.793870523787408));
#36257=CARTESIAN_POINT('Ctrl Pts',(3.77444863801212,1.,0.793870523787408));
#36258=CARTESIAN_POINT('Ctrl Pts',(3.78202460377598,-1.,0.793726235781301));
#36259=CARTESIAN_POINT('Ctrl Pts',(3.78202460377598,1.,0.793726235781301));
#36260=CARTESIAN_POINT('Ctrl Pts',(3.78959439439235,-1.,0.793516871680994));
#36261=CARTESIAN_POINT('Ctrl Pts',(3.78959439439235,1.,0.793516871680994));
#36262=CARTESIAN_POINT('Ctrl Pts',(3.79711921389897,-1.,0.793235612973274));
#36263=CARTESIAN_POINT('Ctrl Pts',(3.79711921389897,1.,0.793235612973274));
#36264=CARTESIAN_POINT('Ctrl Pts',(3.80459229925637,-1.,0.792882695234778));
#36265=CARTESIAN_POINT('Ctrl Pts',(3.80459229925637,1.,0.792882695234778));
#36266=CARTESIAN_POINT('Ctrl Pts',(3.81202588694756,-1.,0.792462483517635));
#36267=CARTESIAN_POINT('Ctrl Pts',(3.81202588694756,1.,0.792462483517635));
#36268=CARTESIAN_POINT('Ctrl Pts',(3.81944345442249,-1.,0.791981740718635));
#36269=CARTESIAN_POINT('Ctrl Pts',(3.81944345442249,1.,0.791981740718635));
#36270=CARTESIAN_POINT('Ctrl Pts',(3.82687033899792,-1.,0.791447528662369));
#36271=CARTESIAN_POINT('Ctrl Pts',(3.82687033899792,1.,0.791447528662369));
#36272=CARTESIAN_POINT('Ctrl Pts',(3.83432392054786,-1.,0.790865012705301));
#36273=CARTESIAN_POINT('Ctrl Pts',(3.83432392054786,1.,0.790865012705301));
#36274=CARTESIAN_POINT('Ctrl Pts',(3.84180762342454,-1.,0.790236124191243));
#36275=CARTESIAN_POINT('Ctrl Pts',(3.84180762342454,1.,0.790236124191243));
#36276=CARTESIAN_POINT('Ctrl Pts',(3.84931637808894,-1.,0.789560798155583));
#36277=CARTESIAN_POINT('Ctrl Pts',(3.84931637808894,1.,0.789560798155583));
#36278=CARTESIAN_POINT('Ctrl Pts',(3.85683995872529,-1.,0.788837734090672));
#36279=CARTESIAN_POINT('Ctrl Pts',(3.85683995872529,1.,0.788837734090672));
#36280=CARTESIAN_POINT('Ctrl Pts',(3.86436702561345,-1.,0.788065315093778));
#36281=CARTESIAN_POINT('Ctrl Pts',(3.86436702561345,1.,0.788065315093778));
#36282=CARTESIAN_POINT('Ctrl Pts',(3.87188916600912,-1.,0.787242527617999));
#36283=CARTESIAN_POINT('Ctrl Pts',(3.87188916600912,1.,0.787242527617999));
#36284=CARTESIAN_POINT('Ctrl Pts',(3.8794040281819,-1.,0.786369675812609));
#36285=CARTESIAN_POINT('Ctrl Pts',(3.8794040281819,1.,0.786369675812609));
#36286=CARTESIAN_POINT('Ctrl Pts',(3.88691313167398,-1.,0.785447890340731));
#36287=CARTESIAN_POINT('Ctrl Pts',(3.88691313167398,1.,0.785447890340731));
#36288=CARTESIAN_POINT('Ctrl Pts',(3.89442039235103,-1.,0.784478799358337));
#36289=CARTESIAN_POINT('Ctrl Pts',(3.89442039235103,1.,0.784478799358337));
#36290=CARTESIAN_POINT('Ctrl Pts',(3.9019303904397,-1.,0.783464141529082));
#36291=CARTESIAN_POINT('Ctrl Pts',(3.9019303904397,1.,0.783464141529082));
#36292=CARTESIAN_POINT('Ctrl Pts',(3.90944671004542,-1.,0.782405395622765));
#36293=CARTESIAN_POINT('Ctrl Pts',(3.90944671004542,1.,0.782405395622765));
#36294=CARTESIAN_POINT('Ctrl Pts',(3.91697036054676,-1.,0.781303428618367));
#36295=CARTESIAN_POINT('Ctrl Pts',(3.91697036054676,1.,0.781303428618367));
#36296=CARTESIAN_POINT('Ctrl Pts',(3.92450058323823,-1.,0.780158678615543));
#36297=CARTESIAN_POINT('Ctrl Pts',(3.92450058323823,1.,0.780158678615543));
#36298=CARTESIAN_POINT('Ctrl Pts',(3.93203552473174,-1.,0.778971308134821));
#36299=CARTESIAN_POINT('Ctrl Pts',(3.93203552473174,1.,0.778971308134821));
#36300=CARTESIAN_POINT('Ctrl Pts',(3.93957296768103,-1.,0.777741370568559));
#36301=CARTESIAN_POINT('Ctrl Pts',(3.93957296768103,1.,0.777741370568559));
#36302=CARTESIAN_POINT('Ctrl Pts',(3.94711101619447,-1.,0.776468966697922));
#36303=CARTESIAN_POINT('Ctrl Pts',(3.94711101619447,1.,0.776468966697922));
#36304=CARTESIAN_POINT('Ctrl Pts',(3.9546488545231,-1.,0.775154418039352));
#36305=CARTESIAN_POINT('Ctrl Pts',(3.9546488545231,1.,0.775154418039352));
#36306=CARTESIAN_POINT('Ctrl Pts',(3.96218649639807,-1.,0.773798212026566));
#36307=CARTESIAN_POINT('Ctrl Pts',(3.96218649639807,1.,0.773798212026566));
#36308=CARTESIAN_POINT('Ctrl Pts',(3.96972446532772,-1.,0.772400931772137));
#36309=CARTESIAN_POINT('Ctrl Pts',(3.96972446532772,1.,0.772400931772137));
#36310=CARTESIAN_POINT('Ctrl Pts',(3.97726349165488,-1.,0.770963190030471));
#36311=CARTESIAN_POINT('Ctrl Pts',(3.97726349165488,1.,0.770963190030471));
#36312=CARTESIAN_POINT('Ctrl Pts',(3.98480422348451,-1.,0.769485566245545));
#36313=CARTESIAN_POINT('Ctrl Pts',(3.98480422348451,1.,0.769485566245545));
#36314=CARTESIAN_POINT('Ctrl Pts',(3.9923468788101,-1.,0.767968531377915));
#36315=CARTESIAN_POINT('Ctrl Pts',(3.9923468788101,1.,0.767968531377915));
#36316=CARTESIAN_POINT('Ctrl Pts',(3.99989129179622,-1.,0.766412457136064));
#36317=CARTESIAN_POINT('Ctrl Pts',(3.99989129179622,1.,0.766412457136064));
#36318=CARTESIAN_POINT('Ctrl Pts',(4.00743706791509,-1.,0.764817648785198));
#36319=CARTESIAN_POINT('Ctrl Pts',(4.00743706791509,1.,0.764817648785198));
#36320=CARTESIAN_POINT('Ctrl Pts',(4.01498370680496,-1.,0.763184371182936));
#36321=CARTESIAN_POINT('Ctrl Pts',(4.01498370680496,1.,0.763184371182936));
#36322=CARTESIAN_POINT('Ctrl Pts',(4.02253072741268,-1.,0.761512875859805));
#36323=CARTESIAN_POINT('Ctrl Pts',(4.02253072741268,1.,0.761512875859805));
#36324=CARTESIAN_POINT('Ctrl Pts',(4.03007781954412,-1.,0.759803433243752));
#36325=CARTESIAN_POINT('Ctrl Pts',(4.03007781954412,1.,0.759803433243752));
#36326=CARTESIAN_POINT('Ctrl Pts',(4.03762485803119,-1.,0.758056338884945));
#36327=CARTESIAN_POINT('Ctrl Pts',(4.03762485803119,1.,0.758056338884945));
#36328=CARTESIAN_POINT('Ctrl Pts',(4.04517182653997,-1.,0.756271902369581));
#36329=CARTESIAN_POINT('Ctrl Pts',(4.04517182653997,1.,0.756271902369581));
#36330=CARTESIAN_POINT('Ctrl Pts',(4.05271876687915,-1.,0.754450441816078));
#36331=CARTESIAN_POINT('Ctrl Pts',(4.05271876687915,1.,0.754450441816078));
#36332=CARTESIAN_POINT('Ctrl Pts',(4.06026572221515,-1.,0.752592276483073));
#36333=CARTESIAN_POINT('Ctrl Pts',(4.06026572221515,1.,0.752592276483073));
#36334=CARTESIAN_POINT('Ctrl Pts',(4.06781267242378,-1.,0.750697720484037));
#36335=CARTESIAN_POINT('Ctrl Pts',(4.06781267242378,1.,0.750697720484037));
#36336=CARTESIAN_POINT('Ctrl Pts',(4.07535951056152,-1.,0.748767076680558));
#36337=CARTESIAN_POINT('Ctrl Pts',(4.07535951056152,1.,0.748767076680558));
#36338=CARTESIAN_POINT('Ctrl Pts',(4.08290608095642,-1.,0.746800631492316));
#36339=CARTESIAN_POINT('Ctrl Pts',(4.08290608095642,1.,0.746800631492316));
#36340=CARTESIAN_POINT('Ctrl Pts',(4.09045220253573,-1.,0.744798649706501));
#36341=CARTESIAN_POINT('Ctrl Pts',(4.09045220253573,1.,0.744798649706501));
#36342=CARTESIAN_POINT('Ctrl Pts',(4.09799769702611,-1.,0.742761369689842));
#36343=CARTESIAN_POINT('Ctrl Pts',(4.09799769702611,1.,0.742761369689842));
#36344=CARTESIAN_POINT('Ctrl Pts',(4.10554241757547,-1.,0.740688998553377));
#36345=CARTESIAN_POINT('Ctrl Pts',(4.10554241757547,1.,0.740688998553377));
#36346=CARTESIAN_POINT('Ctrl Pts',(4.11308626951927,-1.,0.738581708225844));
#36347=CARTESIAN_POINT('Ctrl Pts',(4.11308626951927,1.,0.738581708225844));
#36348=CARTESIAN_POINT('Ctrl Pts',(4.120629196238,-1.,0.736439634331345));
#36349=CARTESIAN_POINT('Ctrl Pts',(4.120629196238,1.,0.736439634331345));
#36350=CARTESIAN_POINT('Ctrl Pts',(4.12666277570844,-1.,0.734698226764093));
#36351=CARTESIAN_POINT('Ctrl Pts',(4.12666277570844,1.,0.734698226764093));
#36352=CARTESIAN_POINT('Ctrl Pts',(4.13118752795207,-1.,0.733376589323547));
#36353=CARTESIAN_POINT('Ctrl Pts',(4.13118752795207,1.,0.733376589323547));
#36354=CARTESIAN_POINT('Ctrl Pts',(4.1342038373684,-1.,0.73248857513516));
#36355=CARTESIAN_POINT('Ctrl Pts',(4.1342038373684,1.,0.73248857513516));
#36356=CARTESIAN_POINT('Ctrl Pts',(4.13571194405636,-1.,0.732042837400621));
#36357=CARTESIAN_POINT('Ctrl Pts',(4.13571194405636,1.,0.732042837400621));
#36358=CARTESIAN_POINT('',(3.66661143271685,1.,0.786422660831985));
#36359=CARTESIAN_POINT('Ctrl Pts',(3.66661143271685,-1.,0.786422660831986));
#36360=CARTESIAN_POINT('Ctrl Pts',(3.66661143271685,-0.666666666666667,
0.786422660831986));
#36361=CARTESIAN_POINT('Ctrl Pts',(3.66661143271685,-0.333333333333333,
0.786422660831986));
#36362=CARTESIAN_POINT('Ctrl Pts',(3.66661143271685,0.333333333333333,0.786422660831986));
#36363=CARTESIAN_POINT('Ctrl Pts',(3.66661143271685,0.666666666666667,0.786422660831986));
#36364=CARTESIAN_POINT('Ctrl Pts',(3.66661143271685,1.,0.786422660831986));
#36365=CARTESIAN_POINT('',(4.13571194405636,1.,0.732042837400621));
#36366=CARTESIAN_POINT('',(4.13571194405636,0.,0.732042837400621));
#36367=CARTESIAN_POINT('Ctrl Pts',(3.66661143271685,1.,0.786422660831985));
#36368=CARTESIAN_POINT('Ctrl Pts',(3.6666431041522,1.,0.786459983895432));
#36369=CARTESIAN_POINT('Ctrl Pts',(3.66680946938292,1.,0.786565919558984));
#36370=CARTESIAN_POINT('Ctrl Pts',(3.66743103898702,1.,0.786774337198063));
#36371=CARTESIAN_POINT('Ctrl Pts',(3.66907505398677,1.,0.787145041181546));
#36372=CARTESIAN_POINT('Ctrl Pts',(3.67252923663655,1.,0.787758799995743));
#36373=CARTESIAN_POINT('Ctrl Pts',(3.67777119516252,1.,0.788569566220286));
#36374=CARTESIAN_POINT('Ctrl Pts',(3.68428439783905,1.,0.789483546064387));
#36375=CARTESIAN_POINT('Ctrl Pts',(3.69172044327364,1.,0.790436284988788));
#36376=CARTESIAN_POINT('Ctrl Pts',(3.69968940808721,1.,0.79135657569598));
#36377=CARTESIAN_POINT('Ctrl Pts',(3.70781724021806,1.,0.792177688845818));
#36378=CARTESIAN_POINT('Ctrl Pts',(3.71580242396124,1.,0.792848377370287));
#36379=CARTESIAN_POINT('Ctrl Pts',(3.72348797293734,1.,0.793347023784205));
#36380=CARTESIAN_POINT('Ctrl Pts',(3.73086914695805,1.,0.793682750269684));
#36381=CARTESIAN_POINT('Ctrl Pts',(3.73803280541687,1.,0.793882700937017));
#36382=CARTESIAN_POINT('Ctrl Pts',(3.74511357728861,1.,0.793982700459952));
#36383=CARTESIAN_POINT('Ctrl Pts',(3.75224692493864,1.,0.794017347371378));
#36384=CARTESIAN_POINT('Ctrl Pts',(3.75951468666257,1.,0.794008429134908));
#36385=CARTESIAN_POINT('Ctrl Pts',(3.76692626931111,1.,0.793961083688992));
#36386=CARTESIAN_POINT('Ctrl Pts',(3.77444863801212,1.,0.793870523787408));
#36387=CARTESIAN_POINT('Ctrl Pts',(3.78202460377598,1.,0.793726235781301));
#36388=CARTESIAN_POINT('Ctrl Pts',(3.78959439439235,1.,0.793516871680994));
#36389=CARTESIAN_POINT('Ctrl Pts',(3.79711921389897,1.,0.793235612973274));
#36390=CARTESIAN_POINT('Ctrl Pts',(3.80459229925637,1.,0.792882695234778));
#36391=CARTESIAN_POINT('Ctrl Pts',(3.81202588694756,1.,0.792462483517635));
#36392=CARTESIAN_POINT('Ctrl Pts',(3.81944345442249,1.,0.791981740718635));
#36393=CARTESIAN_POINT('Ctrl Pts',(3.82687033899792,1.,0.791447528662369));
#36394=CARTESIAN_POINT('Ctrl Pts',(3.83432392054786,1.,0.790865012705301));
#36395=CARTESIAN_POINT('Ctrl Pts',(3.84180762342454,1.,0.790236124191243));
#36396=CARTESIAN_POINT('Ctrl Pts',(3.84931637808894,1.,0.789560798155583));
#36397=CARTESIAN_POINT('Ctrl Pts',(3.85683995872529,1.,0.788837734090672));
#36398=CARTESIAN_POINT('Ctrl Pts',(3.86436702561345,1.,0.788065315093778));
#36399=CARTESIAN_POINT('Ctrl Pts',(3.87188916600912,1.,0.787242527617999));
#36400=CARTESIAN_POINT('Ctrl Pts',(3.8794040281819,1.,0.786369675812609));
#36401=CARTESIAN_POINT('Ctrl Pts',(3.88691313167398,1.,0.785447890340731));
#36402=CARTESIAN_POINT('Ctrl Pts',(3.89442039235103,1.,0.784478799358337));
#36403=CARTESIAN_POINT('Ctrl Pts',(3.9019303904397,1.,0.783464141529082));
#36404=CARTESIAN_POINT('Ctrl Pts',(3.90944671004542,1.,0.782405395622765));
#36405=CARTESIAN_POINT('Ctrl Pts',(3.91697036054676,1.,0.781303428618367));
#36406=CARTESIAN_POINT('Ctrl Pts',(3.92450058323823,1.,0.780158678615543));
#36407=CARTESIAN_POINT('Ctrl Pts',(3.93203552473174,1.,0.778971308134821));
#36408=CARTESIAN_POINT('Ctrl Pts',(3.93957296768103,1.,0.777741370568559));
#36409=CARTESIAN_POINT('Ctrl Pts',(3.94711101619447,1.,0.776468966697922));
#36410=CARTESIAN_POINT('Ctrl Pts',(3.9546488545231,1.,0.775154418039352));
#36411=CARTESIAN_POINT('Ctrl Pts',(3.96218649639807,1.,0.773798212026566));
#36412=CARTESIAN_POINT('Ctrl Pts',(3.96972446532772,1.,0.772400931772137));
#36413=CARTESIAN_POINT('Ctrl Pts',(3.97726349165488,1.,0.770963190030471));
#36414=CARTESIAN_POINT('Ctrl Pts',(3.98480422348451,1.,0.769485566245545));
#36415=CARTESIAN_POINT('Ctrl Pts',(3.9923468788101,1.,0.767968531377915));
#36416=CARTESIAN_POINT('Ctrl Pts',(3.99989129179622,1.,0.766412457136064));
#36417=CARTESIAN_POINT('Ctrl Pts',(4.00743706791509,1.,0.764817648785198));
#36418=CARTESIAN_POINT('Ctrl Pts',(4.01498370680496,1.,0.763184371182936));
#36419=CARTESIAN_POINT('Ctrl Pts',(4.02253072741268,1.,0.761512875859805));
#36420=CARTESIAN_POINT('Ctrl Pts',(4.03007781954412,1.,0.759803433243752));
#36421=CARTESIAN_POINT('Ctrl Pts',(4.03762485803119,1.,0.758056338884945));
#36422=CARTESIAN_POINT('Ctrl Pts',(4.04517182653997,1.,0.756271902369581));
#36423=CARTESIAN_POINT('Ctrl Pts',(4.05271876687915,1.,0.754450441816078));
#36424=CARTESIAN_POINT('Ctrl Pts',(4.06026572221515,1.,0.752592276483073));
#36425=CARTESIAN_POINT('Ctrl Pts',(4.06781267242378,1.,0.750697720484037));
#36426=CARTESIAN_POINT('Ctrl Pts',(4.07535951056152,1.,0.748767076680558));
#36427=CARTESIAN_POINT('Ctrl Pts',(4.08290608095642,1.,0.746800631492316));
#36428=CARTESIAN_POINT('Ctrl Pts',(4.09045220253573,1.,0.744798649706501));
#36429=CARTESIAN_POINT('Ctrl Pts',(4.09799769702611,1.,0.742761369689842));
#36430=CARTESIAN_POINT('Ctrl Pts',(4.10554241757547,1.,0.740688998553377));
#36431=CARTESIAN_POINT('Ctrl Pts',(4.11308626951927,1.,0.738581708225844));
#36432=CARTESIAN_POINT('Ctrl Pts',(4.120629196238,1.,0.736439634331345));
#36433=CARTESIAN_POINT('Ctrl Pts',(4.12666277570844,1.,0.734698226764093));
#36434=CARTESIAN_POINT('Ctrl Pts',(4.13118752795207,1.,0.733376589323547));
#36435=CARTESIAN_POINT('Ctrl Pts',(4.1342038373684,1.,0.73248857513516));
#36436=CARTESIAN_POINT('Ctrl Pts',(4.13571194405636,1.,0.732042837400621));
#36437=CARTESIAN_POINT('Origin',(4.13571194405636,0.,0.732042837400621));
#36438=CARTESIAN_POINT('',(4.15950947128175,1.,0.581791163835816));
#36439=CARTESIAN_POINT('Origin',(0.,0.,0.));
#36440=CARTESIAN_POINT('',(3.62400312501245,1.,0.963899035117249));
#36441=CARTESIAN_POINT('Origin',(0.,1.,0.));
#36442=CARTESIAN_POINT('Ctrl Pts',(3.62400312501245,1.,0.963899035117249));
#36443=CARTESIAN_POINT('Ctrl Pts',(3.62400312501245,0.666666666666667,0.963899035117249));
#36444=CARTESIAN_POINT('Ctrl Pts',(3.62400312501245,0.333333333333333,0.963899035117249));
#36445=CARTESIAN_POINT('Ctrl Pts',(3.62400312501245,-0.333333333333333,
0.963899035117249));
#36446=CARTESIAN_POINT('Ctrl Pts',(3.62400312501245,-0.666666666666667,
0.96389903511725));
#36447=CARTESIAN_POINT('Ctrl Pts',(3.62400312501245,-1.,0.96389903511725));
#36448=CARTESIAN_POINT('Ctrl Pts',(4.01728681790024,-1.,1.22531898815164));
#36449=CARTESIAN_POINT('Ctrl Pts',(4.01728681790024,1.,1.22531898815164));
#36450=CARTESIAN_POINT('Ctrl Pts',(4.0161454457032,-1.,1.22423716681447));
#36451=CARTESIAN_POINT('Ctrl Pts',(4.0161454457032,1.,1.22423716681447));
#36452=CARTESIAN_POINT('Ctrl Pts',(4.01386104434674,-1.,1.22207656456199));
#36453=CARTESIAN_POINT('Ctrl Pts',(4.01386104434674,1.,1.22207656456199));
#36454=CARTESIAN_POINT('Ctrl Pts',(4.01042947142681,-1.,1.21884478244983));
#36455=CARTESIAN_POINT('Ctrl Pts',(4.01042947142681,1.,1.21884478244983));
#36456=CARTESIAN_POINT('Ctrl Pts',(4.00584409524937,-1.,1.21455398918813));
#36457=CARTESIAN_POINT('Ctrl Pts',(4.00584409524937,1.,1.21455398918813));
#36458=CARTESIAN_POINT('Ctrl Pts',(4.00009577952534,-1.,1.20922097030107));
#36459=CARTESIAN_POINT('Ctrl Pts',(4.00009577952534,1.,1.20922097030107));
#36460=CARTESIAN_POINT('Ctrl Pts',(3.99433084800649,-1.,1.2039185237544));
#36461=CARTESIAN_POINT('Ctrl Pts',(3.99433084800649,1.,1.2039185237544));
#36462=CARTESIAN_POINT('Ctrl Pts',(3.98854928957287,-1.,1.19864679609596));
#36463=CARTESIAN_POINT('Ctrl Pts',(3.98854928957287,1.,1.19864679609596));
#36464=CARTESIAN_POINT('Ctrl Pts',(3.98275111052015,-1.,1.19340598349307));
#36465=CARTESIAN_POINT('Ctrl Pts',(3.98275111052015,1.,1.19340598349307));
#36466=CARTESIAN_POINT('Ctrl Pts',(3.97693634766926,-1.,1.18819633715285));
#36467=CARTESIAN_POINT('Ctrl Pts',(3.97693634766926,1.,1.18819633715285));
#36468=CARTESIAN_POINT('Ctrl Pts',(3.9711050516465,-1.,1.18301815039596));
#36469=CARTESIAN_POINT('Ctrl Pts',(3.9711050516465,1.,1.18301815039596));
#36470=CARTESIAN_POINT('Ctrl Pts',(3.96525726357682,-1.,1.17787174135446));
#36471=CARTESIAN_POINT('Ctrl Pts',(3.96525726357682,1.,1.17787174135446));
#36472=CARTESIAN_POINT('Ctrl Pts',(3.95939299213164,-1.,1.17275743590327));
#36473=CARTESIAN_POINT('Ctrl Pts',(3.95939299213164,1.,1.17275743590327));
#36474=CARTESIAN_POINT('Ctrl Pts',(3.95351219510062,-1.,1.16767555244495));
#36475=CARTESIAN_POINT('Ctrl Pts',(3.95351219510062,1.,1.16767555244495));
#36476=CARTESIAN_POINT('Ctrl Pts',(3.9476147478092,-1.,1.16262637999261));
#36477=CARTESIAN_POINT('Ctrl Pts',(3.9476147478092,1.,1.16262637999261));
#36478=CARTESIAN_POINT('Ctrl Pts',(3.94170046685542,-1.,1.15761018341061));
#36479=CARTESIAN_POINT('Ctrl Pts',(3.94170046685542,1.,1.15761018341061));
#36480=CARTESIAN_POINT('Ctrl Pts',(3.9357691705651,-1.,1.15262722716391));
#36481=CARTESIAN_POINT('Ctrl Pts',(3.9357691705651,1.,1.15262722716391));
#36482=CARTESIAN_POINT('Ctrl Pts',(3.92982073294334,-1.,1.14767779451147));
#36483=CARTESIAN_POINT('Ctrl Pts',(3.92982073294334,1.,1.14767779451147));
#36484=CARTESIAN_POINT('Ctrl Pts',(3.92385513133937,-1.,1.14276220561575));
#36485=CARTESIAN_POINT('Ctrl Pts',(3.92385513133937,1.,1.14276220561575));
#36486=CARTESIAN_POINT('Ctrl Pts',(3.91787251936688,-1.,1.13788084225511));
#36487=CARTESIAN_POINT('Ctrl Pts',(3.91787251936688,1.,1.13788084225511));
#36488=CARTESIAN_POINT('Ctrl Pts',(3.91187321145495,-1.,1.13303414693849));
#36489=CARTESIAN_POINT('Ctrl Pts',(3.91187321145495,1.,1.13303414693849));
#36490=CARTESIAN_POINT('Ctrl Pts',(3.90585753318622,-1.,1.12822258281518));
#36491=CARTESIAN_POINT('Ctrl Pts',(3.90585753318622,1.,1.12822258281518));
#36492=CARTESIAN_POINT('Ctrl Pts',(3.89982569749978,-1.,1.12344660099029));
#36493=CARTESIAN_POINT('Ctrl Pts',(3.89982569749978,1.,1.12344660099029));
#36494=CARTESIAN_POINT('Ctrl Pts',(3.89377768340362,-1.,1.11870660794609));
#36495=CARTESIAN_POINT('Ctrl Pts',(3.89377768340362,1.,1.11870660794609));
#36496=CARTESIAN_POINT('Ctrl Pts',(3.88771308285229,-1.,1.11400292434447));
#36497=CARTESIAN_POINT('Ctrl Pts',(3.88771308285229,1.,1.11400292434447));
#36498=CARTESIAN_POINT('Ctrl Pts',(3.88163105531791,-1.,1.10933577224029));
#36499=CARTESIAN_POINT('Ctrl Pts',(3.88163105531791,1.,1.10933577224029));
#36500=CARTESIAN_POINT('Ctrl Pts',(3.87553067187566,-1.,1.10470536603303));
#36501=CARTESIAN_POINT('Ctrl Pts',(3.87553067187566,1.,1.10470536603303));
#36502=CARTESIAN_POINT('Ctrl Pts',(3.86941120134872,-1.,1.10011198761203));
#36503=CARTESIAN_POINT('Ctrl Pts',(3.86941120134872,1.,1.10011198761203));
#36504=CARTESIAN_POINT('Ctrl Pts',(3.86327241021242,-1.,1.09555606505012));
#36505=CARTESIAN_POINT('Ctrl Pts',(3.86327241021242,1.,1.09555606505012));
#36506=CARTESIAN_POINT('Ctrl Pts',(3.85711487933911,-1.,1.09103825516288));
#36507=CARTESIAN_POINT('Ctrl Pts',(3.85711487933911,1.,1.09103825516288));
#36508=CARTESIAN_POINT('Ctrl Pts',(3.8509402522269,-1.,1.08655950846377));
#36509=CARTESIAN_POINT('Ctrl Pts',(3.8509402522269,1.,1.08655950846377));
#36510=CARTESIAN_POINT('Ctrl Pts',(3.84475048030615,-1.,1.08212087917986));
#36511=CARTESIAN_POINT('Ctrl Pts',(3.84475048030615,1.,1.08212087917986));
#36512=CARTESIAN_POINT('Ctrl Pts',(3.83854714117486,-1.,1.07772335353856));
#36513=CARTESIAN_POINT('Ctrl Pts',(3.83854714117486,1.,1.07772335353856));
#36514=CARTESIAN_POINT('Ctrl Pts',(3.83233071195145,-1.,1.0733676663346));
#36515=CARTESIAN_POINT('Ctrl Pts',(3.83233071195145,1.,1.0733676663346));
#36516=CARTESIAN_POINT('Ctrl Pts',(3.82609989967278,-1.,1.0690541318036));
#36517=CARTESIAN_POINT('Ctrl Pts',(3.82609989967278,1.,1.0690541318036));
#36518=CARTESIAN_POINT('Ctrl Pts',(3.81985083953012,-1.,1.06478244038931));
#36519=CARTESIAN_POINT('Ctrl Pts',(3.81985083953012,1.,1.06478244038931));
#36520=CARTESIAN_POINT('Ctrl Pts',(3.81357866117485,-1.,1.06055206187298));
#36521=CARTESIAN_POINT('Ctrl Pts',(3.81357866117485,1.,1.06055206187298));
#36522=CARTESIAN_POINT('Ctrl Pts',(3.80727913637784,-1.,1.05636266918643));
#36523=CARTESIAN_POINT('Ctrl Pts',(3.80727913637784,1.,1.05636266918643));
#36524=CARTESIAN_POINT('Ctrl Pts',(3.80095039790678,-1.,1.05221457990015));
#36525=CARTESIAN_POINT('Ctrl Pts',(3.80095039790678,1.,1.05221457990015));
#36526=CARTESIAN_POINT('Ctrl Pts',(3.79459440308793,-1.,1.04810913267641));
#36527=CARTESIAN_POINT('Ctrl Pts',(3.79459440308793,1.,1.04810913267641));
#36528=CARTESIAN_POINT('Ctrl Pts',(3.78821910787195,-1.,1.04404924374426));
#36529=CARTESIAN_POINT('Ctrl Pts',(3.78821910787195,1.,1.04404924374426));
#36530=CARTESIAN_POINT('Ctrl Pts',(3.78183535008192,-1.,1.04003862055804));
#36531=CARTESIAN_POINT('Ctrl Pts',(3.78183535008192,1.,1.04003862055804));
#36532=CARTESIAN_POINT('Ctrl Pts',(3.77545283140445,-1.,1.03608074678013));
#36533=CARTESIAN_POINT('Ctrl Pts',(3.77545283140445,1.,1.03608074678013));
#36534=CARTESIAN_POINT('Ctrl Pts',(3.76907609832522,-1.,1.0321778660492));
#36535=CARTESIAN_POINT('Ctrl Pts',(3.76907609832522,1.,1.0321778660492));
#36536=CARTESIAN_POINT('Ctrl Pts',(3.76270122291232,-1.,1.02833014458181));
#36537=CARTESIAN_POINT('Ctrl Pts',(3.76270122291232,1.,1.02833014458181));
#36538=CARTESIAN_POINT('Ctrl Pts',(3.75631037456194,-1.,1.0245342944466));
#36539=CARTESIAN_POINT('Ctrl Pts',(3.75631037456194,1.,1.0245342944466));
#36540=CARTESIAN_POINT('Ctrl Pts',(3.74987777155834,-1.,1.02078510487428));
#36541=CARTESIAN_POINT('Ctrl Pts',(3.74987777155834,1.,1.02078510487428));
#36542=CARTESIAN_POINT('Ctrl Pts',(3.74337942504959,-1.,1.01707794311079));
#36543=CARTESIAN_POINT('Ctrl Pts',(3.74337942504959,1.,1.01707794311079));
#36544=CARTESIAN_POINT('Ctrl Pts',(3.73680245055734,-1.,1.01341114319903));
#36545=CARTESIAN_POINT('Ctrl Pts',(3.73680245055734,1.,1.01341114319903));
#36546=CARTESIAN_POINT('Ctrl Pts',(3.73015276704426,-1.,1.00978798539496));
#36547=CARTESIAN_POINT('Ctrl Pts',(3.73015276704426,1.,1.00978798539496));
#36548=CARTESIAN_POINT('Ctrl Pts',(3.72346803750595,-1.,1.0062200073571));
#36549=CARTESIAN_POINT('Ctrl Pts',(3.72346803750595,1.,1.0062200073571));
#36550=CARTESIAN_POINT('Ctrl Pts',(3.71680667125118,-1.,1.00272423396822));
#36551=CARTESIAN_POINT('Ctrl Pts',(3.71680667125118,1.,1.00272423396822));
#36552=CARTESIAN_POINT('Ctrl Pts',(3.71022439713938,-1.,0.999317260756531));
#36553=CARTESIAN_POINT('Ctrl Pts',(3.71022439713938,1.,0.999317260756531));
#36554=CARTESIAN_POINT('Ctrl Pts',(3.70375282282138,-1.,0.996009819772518));
#36555=CARTESIAN_POINT('Ctrl Pts',(3.70375282282138,1.,0.996009819772518));
#36556=CARTESIAN_POINT('Ctrl Pts',(3.69738123415662,-1.,0.992802218332011));
#36557=CARTESIAN_POINT('Ctrl Pts',(3.69738123415662,1.,0.992802218332011));
#36558=CARTESIAN_POINT('Ctrl Pts',(3.69102682138846,-1.,0.989676715398559));
#36559=CARTESIAN_POINT('Ctrl Pts',(3.69102682138846,1.,0.989676715398559));
#36560=CARTESIAN_POINT('Ctrl Pts',(3.68455317926068,-1.,0.986602639863838));
#36561=CARTESIAN_POINT('Ctrl Pts',(3.68455317926068,1.,0.986602639863838));
#36562=CARTESIAN_POINT('Ctrl Pts',(3.67782408841715,-1.,0.98355079147042));
#36563=CARTESIAN_POINT('Ctrl Pts',(3.67782408841715,1.,0.98355079147042));
#36564=CARTESIAN_POINT('Ctrl Pts',(3.67074983340361,-1.,0.980505922458267));
#36565=CARTESIAN_POINT('Ctrl Pts',(3.67074983340361,1.,0.980505922458267));
#36566=CARTESIAN_POINT('Ctrl Pts',(3.66333049637475,-1.,0.977478312751618));
#36567=CARTESIAN_POINT('Ctrl Pts',(3.66333049637475,1.,0.977478312751618));
#36568=CARTESIAN_POINT('Ctrl Pts',(3.65571576735126,-1.,0.974519971354849));
#36569=CARTESIAN_POINT('Ctrl Pts',(3.65571576735126,1.,0.974519971354849));
#36570=CARTESIAN_POINT('Ctrl Pts',(3.64819756447455,-1.,0.971722122061341));
#36571=CARTESIAN_POINT('Ctrl Pts',(3.64819756447455,1.,0.971722122061341));
#36572=CARTESIAN_POINT('Ctrl Pts',(3.64113946505766,-1.,0.969195124675866));
#36573=CARTESIAN_POINT('Ctrl Pts',(3.64113946505766,1.,0.969195124675866));
#36574=CARTESIAN_POINT('Ctrl Pts',(3.63492122081143,-1.,0.967052554541386));
#36575=CARTESIAN_POINT('Ctrl Pts',(3.63492122081143,1.,0.967052554541386));
#36576=CARTESIAN_POINT('Ctrl Pts',(3.62988252139846,-1.,0.965395153165294));
#36577=CARTESIAN_POINT('Ctrl Pts',(3.62988252139846,1.,0.965395153165294));
#36578=CARTESIAN_POINT('Ctrl Pts',(3.62625391254797,-1.,0.964291001273288));
#36579=CARTESIAN_POINT('Ctrl Pts',(3.62625391254797,1.,0.964291001273288));
#36580=CARTESIAN_POINT('Ctrl Pts',(3.6245656860652,-1.,0.96387577453062));
#36581=CARTESIAN_POINT('Ctrl Pts',(3.6245656860652,1.,0.96387577453062));
#36582=CARTESIAN_POINT('Ctrl Pts',(3.62399933639914,-1.,0.963832486395052));
#36583=CARTESIAN_POINT('Ctrl Pts',(3.62399933639914,1.,0.963832486395052));
#36584=CARTESIAN_POINT('Ctrl Pts',(3.62393257642052,-1.,0.963922720982194));
#36585=CARTESIAN_POINT('Ctrl Pts',(3.62393257642052,1.,0.963922720982194));
#36586=CARTESIAN_POINT('Ctrl Pts',(3.62397690409552,-1.,0.963997613369571));
#36587=CARTESIAN_POINT('Ctrl Pts',(3.62397690409552,1.,0.963997613369571));
#36588=CARTESIAN_POINT('',(4.01728681790024,1.,1.22531898815164));
#36589=CARTESIAN_POINT('Ctrl Pts',(4.01728681790024,1.,1.22531898815164));
#36590=CARTESIAN_POINT('Ctrl Pts',(4.0161454457032,1.,1.22423716681447));
#36591=CARTESIAN_POINT('Ctrl Pts',(4.01386104434674,1.,1.22207656456199));
#36592=CARTESIAN_POINT('Ctrl Pts',(4.01042947142681,1.,1.21884478244983));
#36593=CARTESIAN_POINT('Ctrl Pts',(4.00584409524937,1.,1.21455398918813));
#36594=CARTESIAN_POINT('Ctrl Pts',(4.00009577952534,1.,1.20922097030107));
#36595=CARTESIAN_POINT('Ctrl Pts',(3.99433084800649,1.,1.2039185237544));
#36596=CARTESIAN_POINT('Ctrl Pts',(3.98854928957287,1.,1.19864679609596));
#36597=CARTESIAN_POINT('Ctrl Pts',(3.98275111052015,1.,1.19340598349307));
#36598=CARTESIAN_POINT('Ctrl Pts',(3.97693634766926,1.,1.18819633715285));
#36599=CARTESIAN_POINT('Ctrl Pts',(3.9711050516465,1.,1.18301815039596));
#36600=CARTESIAN_POINT('Ctrl Pts',(3.96525726357682,1.,1.17787174135446));
#36601=CARTESIAN_POINT('Ctrl Pts',(3.95939299213164,1.,1.17275743590327));
#36602=CARTESIAN_POINT('Ctrl Pts',(3.95351219510062,1.,1.16767555244495));
#36603=CARTESIAN_POINT('Ctrl Pts',(3.9476147478092,1.,1.16262637999261));
#36604=CARTESIAN_POINT('Ctrl Pts',(3.94170046685542,1.,1.15761018341061));
#36605=CARTESIAN_POINT('Ctrl Pts',(3.9357691705651,1.,1.15262722716391));
#36606=CARTESIAN_POINT('Ctrl Pts',(3.92982073294334,1.,1.14767779451147));
#36607=CARTESIAN_POINT('Ctrl Pts',(3.92385513133937,1.,1.14276220561575));
#36608=CARTESIAN_POINT('Ctrl Pts',(3.91787251936688,1.,1.13788084225511));
#36609=CARTESIAN_POINT('Ctrl Pts',(3.91187321145495,1.,1.13303414693849));
#36610=CARTESIAN_POINT('Ctrl Pts',(3.90585753318622,1.,1.12822258281518));
#36611=CARTESIAN_POINT('Ctrl Pts',(3.89982569749978,1.,1.12344660099029));
#36612=CARTESIAN_POINT('Ctrl Pts',(3.89377768340362,1.,1.11870660794609));
#36613=CARTESIAN_POINT('Ctrl Pts',(3.88771308285229,1.,1.11400292434447));
#36614=CARTESIAN_POINT('Ctrl Pts',(3.88163105531791,1.,1.10933577224029));
#36615=CARTESIAN_POINT('Ctrl Pts',(3.87553067187566,1.,1.10470536603303));
#36616=CARTESIAN_POINT('Ctrl Pts',(3.86941120134872,1.,1.10011198761203));
#36617=CARTESIAN_POINT('Ctrl Pts',(3.86327241021242,1.,1.09555606505012));
#36618=CARTESIAN_POINT('Ctrl Pts',(3.85711487933911,1.,1.09103825516288));
#36619=CARTESIAN_POINT('Ctrl Pts',(3.8509402522269,1.,1.08655950846377));
#36620=CARTESIAN_POINT('Ctrl Pts',(3.84475048030615,1.,1.08212087917986));
#36621=CARTESIAN_POINT('Ctrl Pts',(3.83854714117486,1.,1.07772335353856));
#36622=CARTESIAN_POINT('Ctrl Pts',(3.83233071195145,1.,1.0733676663346));
#36623=CARTESIAN_POINT('Ctrl Pts',(3.82609989967278,1.,1.0690541318036));
#36624=CARTESIAN_POINT('Ctrl Pts',(3.81985083953012,1.,1.06478244038931));
#36625=CARTESIAN_POINT('Ctrl Pts',(3.81357866117485,1.,1.06055206187298));
#36626=CARTESIAN_POINT('Ctrl Pts',(3.80727913637784,1.,1.05636266918643));
#36627=CARTESIAN_POINT('Ctrl Pts',(3.80095039790678,1.,1.05221457990015));
#36628=CARTESIAN_POINT('Ctrl Pts',(3.79459440308793,1.,1.04810913267641));
#36629=CARTESIAN_POINT('Ctrl Pts',(3.78821910787195,1.,1.04404924374426));
#36630=CARTESIAN_POINT('Ctrl Pts',(3.78183535008192,1.,1.04003862055804));
#36631=CARTESIAN_POINT('Ctrl Pts',(3.77545283140445,1.,1.03608074678013));
#36632=CARTESIAN_POINT('Ctrl Pts',(3.76907609832522,1.,1.0321778660492));
#36633=CARTESIAN_POINT('Ctrl Pts',(3.76270122291232,1.,1.02833014458181));
#36634=CARTESIAN_POINT('Ctrl Pts',(3.75631037456194,1.,1.0245342944466));
#36635=CARTESIAN_POINT('Ctrl Pts',(3.74987777155834,1.,1.02078510487428));
#36636=CARTESIAN_POINT('Ctrl Pts',(3.74337942504959,1.,1.01707794311079));
#36637=CARTESIAN_POINT('Ctrl Pts',(3.73680245055734,1.,1.01341114319903));
#36638=CARTESIAN_POINT('Ctrl Pts',(3.73015276704426,1.,1.00978798539496));
#36639=CARTESIAN_POINT('Ctrl Pts',(3.72346803750595,1.,1.0062200073571));
#36640=CARTESIAN_POINT('Ctrl Pts',(3.71680667125118,1.,1.00272423396822));
#36641=CARTESIAN_POINT('Ctrl Pts',(3.71022439713938,1.,0.999317260756531));
#36642=CARTESIAN_POINT('Ctrl Pts',(3.70375282282138,1.,0.996009819772518));
#36643=CARTESIAN_POINT('Ctrl Pts',(3.69738123415662,1.,0.992802218332011));
#36644=CARTESIAN_POINT('Ctrl Pts',(3.69102682138846,1.,0.989676715398559));
#36645=CARTESIAN_POINT('Ctrl Pts',(3.68455317926068,1.,0.986602639863838));
#36646=CARTESIAN_POINT('Ctrl Pts',(3.67782408841715,1.,0.98355079147042));
#36647=CARTESIAN_POINT('Ctrl Pts',(3.67074983340361,1.,0.980505922458267));
#36648=CARTESIAN_POINT('Ctrl Pts',(3.66333049637475,1.,0.977478312751618));
#36649=CARTESIAN_POINT('Ctrl Pts',(3.65571576735126,1.,0.974519971354849));
#36650=CARTESIAN_POINT('Ctrl Pts',(3.64819756447455,1.,0.971722122061341));
#36651=CARTESIAN_POINT('Ctrl Pts',(3.64113946505766,1.,0.969195124675866));
#36652=CARTESIAN_POINT('Ctrl Pts',(3.63492122081143,1.,0.967052554541386));
#36653=CARTESIAN_POINT('Ctrl Pts',(3.62988252139846,1.,0.965395153165294));
#36654=CARTESIAN_POINT('Ctrl Pts',(3.62652618145335,1.,0.964373850166458));
#36655=CARTESIAN_POINT('Ctrl Pts',(3.62489305727662,1.,0.963957782642844));
#36656=CARTESIAN_POINT('Ctrl Pts',(3.62424461507588,1.,0.963861297423241));
#36657=CARTESIAN_POINT('Ctrl Pts',(3.6240482887845,1.,0.963880158555582));
#36658=CARTESIAN_POINT('Ctrl Pts',(3.62400312501245,1.,0.963899035117249));
#36659=CARTESIAN_POINT('',(4.01728681790024,0.,1.22531898815164));
#36660=CARTESIAN_POINT('Ctrl Pts',(3.49848248301936,-1.,1.35022972712301));
#36661=CARTESIAN_POINT('Ctrl Pts',(3.49848248301936,1.,1.35022972712301));
#36662=CARTESIAN_POINT('Ctrl Pts',(3.4984026005375,-1.,1.35026426118402));
#36663=CARTESIAN_POINT('Ctrl Pts',(3.4984026005375,1.,1.35026426118402));
#36664=CARTESIAN_POINT('Ctrl Pts',(3.49840357193736,-1.,1.35037650303019));
#36665=CARTESIAN_POINT('Ctrl Pts',(3.49840357193736,1.,1.35037650303019));
#36666=CARTESIAN_POINT('Ctrl Pts',(3.49888720257132,-1.,1.35067437417484));
#36667=CARTESIAN_POINT('Ctrl Pts',(3.49888720257132,1.,1.35067437417484));
#36668=CARTESIAN_POINT('Ctrl Pts',(3.5004970706414,-1.,1.3513307633124));
#36669=CARTESIAN_POINT('Ctrl Pts',(3.5004970706414,1.,1.3513307633124));
#36670=CARTESIAN_POINT('Ctrl Pts',(3.50408168106261,-1.,1.35257032843486));
#36671=CARTESIAN_POINT('Ctrl Pts',(3.50408168106261,1.,1.35257032843486));
#36672=CARTESIAN_POINT('Ctrl Pts',(3.50913227059999,-1.,1.35419113575956));
#36673=CARTESIAN_POINT('Ctrl Pts',(3.50913227059999,1.,1.35419113575956));
#36674=CARTESIAN_POINT('Ctrl Pts',(3.51542230699556,-1.,1.35611275237152));
#36675=CARTESIAN_POINT('Ctrl Pts',(3.51542230699556,1.,1.35611275237152));
#36676=CARTESIAN_POINT('Ctrl Pts',(3.52261776116748,-1.,1.35821701528836));
#36677=CARTESIAN_POINT('Ctrl Pts',(3.52261776116748,1.,1.35821701528836));
#36678=CARTESIAN_POINT('Ctrl Pts',(3.530344649616,-1.,1.36037259643734));
#36679=CARTESIAN_POINT('Ctrl Pts',(3.530344649616,1.,1.36037259643734));
#36680=CARTESIAN_POINT('Ctrl Pts',(3.53824396424961,-1.,1.36245507339307));
#36681=CARTESIAN_POINT('Ctrl Pts',(3.53824396424961,1.,1.36245507339307));
#36682=CARTESIAN_POINT('Ctrl Pts',(3.54602591832973,-1.,1.36436666257598));
#36683=CARTESIAN_POINT('Ctrl Pts',(3.54602591832973,1.,1.36436666257598));
#36684=CARTESIAN_POINT('Ctrl Pts',(3.55353883995949,-1.,1.3660614545677));
#36685=CARTESIAN_POINT('Ctrl Pts',(3.55353883995949,1.,1.3660614545677));
#36686=CARTESIAN_POINT('Ctrl Pts',(3.56077662028649,-1.,1.36754771771233));
#36687=CARTESIAN_POINT('Ctrl Pts',(3.56077662028649,1.,1.36754771771233));
#36688=CARTESIAN_POINT('Ctrl Pts',(3.5678208030466,-1.,1.36886584973389));
#36689=CARTESIAN_POINT('Ctrl Pts',(3.5678208030466,1.,1.36886584973389));
#36690=CARTESIAN_POINT('Ctrl Pts',(3.57479875549486,-1.,1.37007229485659));
#36691=CARTESIAN_POINT('Ctrl Pts',(3.57479875549486,1.,1.37007229485659));
#36692=CARTESIAN_POINT('Ctrl Pts',(3.58183885982715,-1.,1.37122241663062));
#36693=CARTESIAN_POINT('Ctrl Pts',(3.58183885982715,1.,1.37122241663062));
#36694=CARTESIAN_POINT('Ctrl Pts',(3.58901853846365,-1.,1.37235053660976));
#36695=CARTESIAN_POINT('Ctrl Pts',(3.58901853846365,1.,1.37235053660976));
#36696=CARTESIAN_POINT('Ctrl Pts',(3.59634627869048,-1.,1.37346320103157));
#36697=CARTESIAN_POINT('Ctrl Pts',(3.59634627869048,1.,1.37346320103157));
#36698=CARTESIAN_POINT('Ctrl Pts',(3.60379020123988,-1.,1.37455051379623));
#36699=CARTESIAN_POINT('Ctrl Pts',(3.60379020123988,1.,1.37455051379623));
#36700=CARTESIAN_POINT('Ctrl Pts',(3.61129546591064,-1.,1.37559314436634));
#36701=CARTESIAN_POINT('Ctrl Pts',(3.61129546591064,1.,1.37559314436634));
#36702=CARTESIAN_POINT('Ctrl Pts',(3.6188048116042,-1.,1.37657053403107));
#36703=CARTESIAN_POINT('Ctrl Pts',(3.6188048116042,1.,1.37657053403107));
#36704=CARTESIAN_POINT('Ctrl Pts',(3.62628098665145,-1.,1.37746987919881));
#36705=CARTESIAN_POINT('Ctrl Pts',(3.62628098665145,1.,1.37746987919881));
#36706=CARTESIAN_POINT('Ctrl Pts',(3.63371727442486,-1.,1.37829035457339));
#36707=CARTESIAN_POINT('Ctrl Pts',(3.63371727442486,1.,1.37829035457339));
#36708=CARTESIAN_POINT('Ctrl Pts',(3.64112507791141,-1.,1.37903818567359));
#36709=CARTESIAN_POINT('Ctrl Pts',(3.64112507791141,1.,1.37903818567359));
#36710=CARTESIAN_POINT('Ctrl Pts',(3.64852652756456,-1.,1.37972372481603));
#36711=CARTESIAN_POINT('Ctrl Pts',(3.64852652756456,1.,1.37972372481603));
#36712=CARTESIAN_POINT('Ctrl Pts',(3.6559455440439,-1.,1.38035791051213));
#36713=CARTESIAN_POINT('Ctrl Pts',(3.6559455440439,1.,1.38035791051213));
#36714=CARTESIAN_POINT('Ctrl Pts',(3.66339848520857,-1.,1.38094856333552));
#36715=CARTESIAN_POINT('Ctrl Pts',(3.66339848520857,1.,1.38094856333552));
#36716=CARTESIAN_POINT('Ctrl Pts',(3.67088843112262,-1.,1.38149812653868));
#36717=CARTESIAN_POINT('Ctrl Pts',(3.67088843112262,1.,1.38149812653868));
#36718=CARTESIAN_POINT('Ctrl Pts',(3.67841038482414,-1.,1.3820057429062));
#36719=CARTESIAN_POINT('Ctrl Pts',(3.67841038482414,1.,1.3820057429062));
#36720=CARTESIAN_POINT('Ctrl Pts',(3.68595444983837,-1.,1.38246852827182));
#36721=CARTESIAN_POINT('Ctrl Pts',(3.68595444983837,1.,1.38246852827182));
#36722=CARTESIAN_POINT('Ctrl Pts',(3.69350967899526,-1.,1.38288311171651));
#36723=CARTESIAN_POINT('Ctrl Pts',(3.69350967899526,1.,1.38288311171651));
#36724=CARTESIAN_POINT('Ctrl Pts',(3.701067921679,-1.,1.38324717612865));
#36725=CARTESIAN_POINT('Ctrl Pts',(3.701067921679,1.,1.38324717612865));
#36726=CARTESIAN_POINT('Ctrl Pts',(3.70862680753347,-1.,1.38356065402124));
#36727=CARTESIAN_POINT('Ctrl Pts',(3.70862680753347,1.,1.38356065402124));
#36728=CARTESIAN_POINT('Ctrl Pts',(3.7161876605181,-1.,1.38382489984586));
#36729=CARTESIAN_POINT('Ctrl Pts',(3.7161876605181,1.,1.38382489984586));
#36730=CARTESIAN_POINT('Ctrl Pts',(3.72375409358803,-1.,1.3840421342895));
#36731=CARTESIAN_POINT('Ctrl Pts',(3.72375409358803,1.,1.3840421342895));
#36732=CARTESIAN_POINT('Ctrl Pts',(3.73133035859282,-1.,1.38421479111531));
#36733=CARTESIAN_POINT('Ctrl Pts',(3.73133035859282,1.,1.38421479111531));
#36734=CARTESIAN_POINT('Ctrl Pts',(3.73891976418104,-1.,1.38434489156458));
#36735=CARTESIAN_POINT('Ctrl Pts',(3.73891976418104,1.,1.38434489156458));
#36736=CARTESIAN_POINT('Ctrl Pts',(3.74652317167876,-1.,1.38443344984394));
#36737=CARTESIAN_POINT('Ctrl Pts',(3.74652317167876,1.,1.38443344984394));
#36738=CARTESIAN_POINT('Ctrl Pts',(3.7541397631875,-1.,1.38448077997163));
#36739=CARTESIAN_POINT('Ctrl Pts',(3.7541397631875,1.,1.38448077997163));
#36740=CARTESIAN_POINT('Ctrl Pts',(3.76176768271367,-1.,1.3844867525335));
#36741=CARTESIAN_POINT('Ctrl Pts',(3.76176768271367,1.,1.3844867525335));
#36742=CARTESIAN_POINT('Ctrl Pts',(3.76940473185779,-1.,1.38445107339518));
#36743=CARTESIAN_POINT('Ctrl Pts',(3.76940473185779,1.,1.38445107339518));
#36744=CARTESIAN_POINT('Ctrl Pts',(3.77704902230418,-1.,1.38437354551428));
#36745=CARTESIAN_POINT('Ctrl Pts',(3.77704902230418,1.,1.38437354551428));
#36746=CARTESIAN_POINT('Ctrl Pts',(3.78469969805082,-1.,1.38425435883756));
#36747=CARTESIAN_POINT('Ctrl Pts',(3.78469969805082,1.,1.38425435883756));
#36748=CARTESIAN_POINT('Ctrl Pts',(3.79235669640841,-1.,1.38409399694566));
#36749=CARTESIAN_POINT('Ctrl Pts',(3.79235669640841,1.,1.38409399694566));
#36750=CARTESIAN_POINT('Ctrl Pts',(3.80002044322111,-1.,1.38389311766682));
#36751=CARTESIAN_POINT('Ctrl Pts',(3.80002044322111,1.,1.38389311766682));
#36752=CARTESIAN_POINT('Ctrl Pts',(3.80769156398411,-1.,1.3836524404622));
#36753=CARTESIAN_POINT('Ctrl Pts',(3.80769156398411,1.,1.3836524404622));
#36754=CARTESIAN_POINT('Ctrl Pts',(3.81537060817811,-1.,1.38337263902782));
#36755=CARTESIAN_POINT('Ctrl Pts',(3.81537060817811,1.,1.38337263902782));
#36756=CARTESIAN_POINT('Ctrl Pts',(3.82305771743829,-1.,1.38305421262763));
#36757=CARTESIAN_POINT('Ctrl Pts',(3.82305771743829,1.,1.38305421262763));
#36758=CARTESIAN_POINT('Ctrl Pts',(3.8307526698229,-1.,1.38269750245138));
#36759=CARTESIAN_POINT('Ctrl Pts',(3.8307526698229,1.,1.38269750245138));
#36760=CARTESIAN_POINT('Ctrl Pts',(3.83845502790746,-1.,1.38230274828822));
#36761=CARTESIAN_POINT('Ctrl Pts',(3.83845502790746,1.,1.38230274828822));
#36762=CARTESIAN_POINT('Ctrl Pts',(3.84616425605764,-1.,1.38187013346109));
#36763=CARTESIAN_POINT('Ctrl Pts',(3.84616425605764,1.,1.38187013346109));
#36764=CARTESIAN_POINT('Ctrl Pts',(3.85387983979481,-1.,1.3813998311505));
#36765=CARTESIAN_POINT('Ctrl Pts',(3.85387983979481,1.,1.3813998311505));
#36766=CARTESIAN_POINT('Ctrl Pts',(3.86160143043959,-1.,1.3808920599299));
#36767=CARTESIAN_POINT('Ctrl Pts',(3.86160143043959,1.,1.3808920599299));
#36768=CARTESIAN_POINT('Ctrl Pts',(3.86932885813068,-1.,1.38034709213014));
#36769=CARTESIAN_POINT('Ctrl Pts',(3.86932885813068,1.,1.38034709213014));
#36770=CARTESIAN_POINT('Ctrl Pts',(3.87706205830532,-1.,1.37976523097073));
#36771=CARTESIAN_POINT('Ctrl Pts',(3.87706205830532,1.,1.37976523097073));
#36772=CARTESIAN_POINT('Ctrl Pts',(3.88480102249277,-1.,1.37914679719383));
#36773=CARTESIAN_POINT('Ctrl Pts',(3.88480102249277,1.,1.37914679719383));
#36774=CARTESIAN_POINT('Ctrl Pts',(3.89254574338496,-1.,1.3784921128802));
#36775=CARTESIAN_POINT('Ctrl Pts',(3.89254574338496,1.,1.3784921128802));
#36776=CARTESIAN_POINT('Ctrl Pts',(3.90029615196727,-1.,1.37780148512792));
#36777=CARTESIAN_POINT('Ctrl Pts',(3.90029615196727,1.,1.37780148512792));
#36778=CARTESIAN_POINT('Ctrl Pts',(3.90805209523486,-1.,1.3770751963402));
#36779=CARTESIAN_POINT('Ctrl Pts',(3.90805209523486,1.,1.3770751963402));
#36780=CARTESIAN_POINT('Ctrl Pts',(3.91581337462644,-1.,1.37631350505797));
#36781=CARTESIAN_POINT('Ctrl Pts',(3.91581337462644,1.,1.37631350505797));
#36782=CARTESIAN_POINT('Ctrl Pts',(3.92357976987672,-1.,1.37551664448242));
#36783=CARTESIAN_POINT('Ctrl Pts',(3.92357976987672,1.,1.37551664448242));
#36784=CARTESIAN_POINT('Ctrl Pts',(3.93135106761844,-1.,1.37468482215751));
#36785=CARTESIAN_POINT('Ctrl Pts',(3.93135106761844,1.,1.37468482215751));
#36786=CARTESIAN_POINT('Ctrl Pts',(3.93912709040818,-1.,1.37381821967165));
#36787=CARTESIAN_POINT('Ctrl Pts',(3.93912709040818,1.,1.37381821967165));
#36788=CARTESIAN_POINT('Ctrl Pts',(3.94690771785133,-1.,1.37291699202807));
#36789=CARTESIAN_POINT('Ctrl Pts',(3.94690771785133,1.,1.37291699202807));
#36790=CARTESIAN_POINT('Ctrl Pts',(3.95469287280914,-1.,1.37198126432386));
#36791=CARTESIAN_POINT('Ctrl Pts',(3.95469287280914,1.,1.37198126432386));
#36792=CARTESIAN_POINT('Ctrl Pts',(3.96092458506535,-1.,1.3712051561502));
#36793=CARTESIAN_POINT('Ctrl Pts',(3.96092458506535,1.,1.3712051561502));
#36794=CARTESIAN_POINT('Ctrl Pts',(3.96560037974645,-1.,1.37060761745635));
#36795=CARTESIAN_POINT('Ctrl Pts',(3.96560037974645,1.,1.37060761745635));
#36796=CARTESIAN_POINT('Ctrl Pts',(3.9687184694131,-1.,1.37020239094614));
#36797=CARTESIAN_POINT('Ctrl Pts',(3.9687184694131,1.,1.37020239094614));
#36798=CARTESIAN_POINT('Ctrl Pts',(3.97027773754922,-1.,1.36999806084573));
#36799=CARTESIAN_POINT('Ctrl Pts',(3.97027773754922,1.,1.36999806084573));
#36800=CARTESIAN_POINT('',(3.4984457533445,1.,1.35032489087101));
#36801=CARTESIAN_POINT('Ctrl Pts',(3.4984457533445,-1.,1.35032489087101));
#36802=CARTESIAN_POINT('Ctrl Pts',(3.4984457533445,-0.666666666666667,1.35032489087101));
#36803=CARTESIAN_POINT('Ctrl Pts',(3.4984457533445,-0.333333333333333,1.35032489087101));
#36804=CARTESIAN_POINT('Ctrl Pts',(3.4984457533445,0.333333333333333,1.35032489087101));
#36805=CARTESIAN_POINT('Ctrl Pts',(3.4984457533445,0.666666666666667,1.35032489087101));
#36806=CARTESIAN_POINT('Ctrl Pts',(3.4984457533445,1.,1.35032489087101));
#36807=CARTESIAN_POINT('',(3.97027773754922,1.,1.36999806084573));
#36808=CARTESIAN_POINT('',(3.97027773754922,0.,1.36999806084573));
#36809=CARTESIAN_POINT('Ctrl Pts',(3.4984457533445,1.,1.35032489087101));
#36810=CARTESIAN_POINT('Ctrl Pts',(3.49847119623846,1.,1.35036670892966));
#36811=CARTESIAN_POINT('Ctrl Pts',(3.49861894124827,1.,1.35049736560527));
#36812=CARTESIAN_POINT('Ctrl Pts',(3.49920025459723,1.,1.35080045218587));
#36813=CARTESIAN_POINT('Ctrl Pts',(3.5007660381649,1.,1.35142377279517));
#36814=CARTESIAN_POINT('Ctrl Pts',(3.50408168106261,1.,1.35257032843486));
#36815=CARTESIAN_POINT('Ctrl Pts',(3.50913227059999,1.,1.35419113575956));
#36816=CARTESIAN_POINT('Ctrl Pts',(3.51542230699556,1.,1.35611275237152));
#36817=CARTESIAN_POINT('Ctrl Pts',(3.52261776116748,1.,1.35821701528836));
#36818=CARTESIAN_POINT('Ctrl Pts',(3.530344649616,1.,1.36037259643734));
#36819=CARTESIAN_POINT('Ctrl Pts',(3.53824396424961,1.,1.36245507339307));
#36820=CARTESIAN_POINT('Ctrl Pts',(3.54602591832973,1.,1.36436666257598));
#36821=CARTESIAN_POINT('Ctrl Pts',(3.55353883995949,1.,1.3660614545677));
#36822=CARTESIAN_POINT('Ctrl Pts',(3.56077662028649,1.,1.36754771771233));
#36823=CARTESIAN_POINT('Ctrl Pts',(3.5678208030466,1.,1.36886584973389));
#36824=CARTESIAN_POINT('Ctrl Pts',(3.57479875549486,1.,1.37007229485659));
#36825=CARTESIAN_POINT('Ctrl Pts',(3.58183885982715,1.,1.37122241663062));
#36826=CARTESIAN_POINT('Ctrl Pts',(3.58901853846365,1.,1.37235053660976));
#36827=CARTESIAN_POINT('Ctrl Pts',(3.59634627869048,1.,1.37346320103157));
#36828=CARTESIAN_POINT('Ctrl Pts',(3.60379020123988,1.,1.37455051379623));
#36829=CARTESIAN_POINT('Ctrl Pts',(3.61129546591064,1.,1.37559314436634));
#36830=CARTESIAN_POINT('Ctrl Pts',(3.6188048116042,1.,1.37657053403107));
#36831=CARTESIAN_POINT('Ctrl Pts',(3.62628098665145,1.,1.37746987919881));
#36832=CARTESIAN_POINT('Ctrl Pts',(3.63371727442486,1.,1.37829035457339));
#36833=CARTESIAN_POINT('Ctrl Pts',(3.64112507791141,1.,1.37903818567359));
#36834=CARTESIAN_POINT('Ctrl Pts',(3.64852652756456,1.,1.37972372481603));
#36835=CARTESIAN_POINT('Ctrl Pts',(3.6559455440439,1.,1.38035791051213));
#36836=CARTESIAN_POINT('Ctrl Pts',(3.66339848520857,1.,1.38094856333552));
#36837=CARTESIAN_POINT('Ctrl Pts',(3.67088843112262,1.,1.38149812653868));
#36838=CARTESIAN_POINT('Ctrl Pts',(3.67841038482414,1.,1.3820057429062));
#36839=CARTESIAN_POINT('Ctrl Pts',(3.68595444983837,1.,1.38246852827182));
#36840=CARTESIAN_POINT('Ctrl Pts',(3.69350967899526,1.,1.38288311171651));
#36841=CARTESIAN_POINT('Ctrl Pts',(3.701067921679,1.,1.38324717612865));
#36842=CARTESIAN_POINT('Ctrl Pts',(3.70862680753347,1.,1.38356065402124));
#36843=CARTESIAN_POINT('Ctrl Pts',(3.7161876605181,1.,1.38382489984586));
#36844=CARTESIAN_POINT('Ctrl Pts',(3.72375409358803,1.,1.3840421342895));
#36845=CARTESIAN_POINT('Ctrl Pts',(3.73133035859282,1.,1.38421479111531));
#36846=CARTESIAN_POINT('Ctrl Pts',(3.73891976418104,1.,1.38434489156458));
#36847=CARTESIAN_POINT('Ctrl Pts',(3.74652317167876,1.,1.38443344984394));
#36848=CARTESIAN_POINT('Ctrl Pts',(3.7541397631875,1.,1.38448077997163));
#36849=CARTESIAN_POINT('Ctrl Pts',(3.76176768271367,1.,1.3844867525335));
#36850=CARTESIAN_POINT('Ctrl Pts',(3.76940473185779,1.,1.38445107339518));
#36851=CARTESIAN_POINT('Ctrl Pts',(3.77704902230418,1.,1.38437354551428));
#36852=CARTESIAN_POINT('Ctrl Pts',(3.78469969805082,1.,1.38425435883756));
#36853=CARTESIAN_POINT('Ctrl Pts',(3.79235669640841,1.,1.38409399694566));
#36854=CARTESIAN_POINT('Ctrl Pts',(3.80002044322111,1.,1.38389311766682));
#36855=CARTESIAN_POINT('Ctrl Pts',(3.80769156398411,1.,1.3836524404622));
#36856=CARTESIAN_POINT('Ctrl Pts',(3.81537060817811,1.,1.38337263902782));
#36857=CARTESIAN_POINT('Ctrl Pts',(3.82305771743829,1.,1.38305421262763));
#36858=CARTESIAN_POINT('Ctrl Pts',(3.8307526698229,1.,1.38269750245138));
#36859=CARTESIAN_POINT('Ctrl Pts',(3.83845502790746,1.,1.38230274828822));
#36860=CARTESIAN_POINT('Ctrl Pts',(3.84616425605764,1.,1.38187013346109));
#36861=CARTESIAN_POINT('Ctrl Pts',(3.85387983979481,1.,1.3813998311505));
#36862=CARTESIAN_POINT('Ctrl Pts',(3.86160143043959,1.,1.3808920599299));
#36863=CARTESIAN_POINT('Ctrl Pts',(3.86932885813068,1.,1.38034709213014));
#36864=CARTESIAN_POINT('Ctrl Pts',(3.87706205830532,1.,1.37976523097073));
#36865=CARTESIAN_POINT('Ctrl Pts',(3.88480102249277,1.,1.37914679719383));
#36866=CARTESIAN_POINT('Ctrl Pts',(3.89254574338496,1.,1.3784921128802));
#36867=CARTESIAN_POINT('Ctrl Pts',(3.90029615196727,1.,1.37780148512792));
#36868=CARTESIAN_POINT('Ctrl Pts',(3.90805209523486,1.,1.3770751963402));
#36869=CARTESIAN_POINT('Ctrl Pts',(3.91581337462644,1.,1.37631350505797));
#36870=CARTESIAN_POINT('Ctrl Pts',(3.92357976987672,1.,1.37551664448242));
#36871=CARTESIAN_POINT('Ctrl Pts',(3.93135106761844,1.,1.37468482215751));
#36872=CARTESIAN_POINT('Ctrl Pts',(3.93912709040818,1.,1.37381821967165));
#36873=CARTESIAN_POINT('Ctrl Pts',(3.94690771785133,1.,1.37291699202807));
#36874=CARTESIAN_POINT('Ctrl Pts',(3.95469287280914,1.,1.37198126432386));
#36875=CARTESIAN_POINT('Ctrl Pts',(3.96092458506535,1.,1.3712051561502));
#36876=CARTESIAN_POINT('Ctrl Pts',(3.96560037974645,1.,1.37060761745635));
#36877=CARTESIAN_POINT('Ctrl Pts',(3.9687184694131,1.,1.37020239094614));
#36878=CARTESIAN_POINT('Ctrl Pts',(3.97027773754922,1.,1.36999806084573));
#36879=CARTESIAN_POINT('Origin',(3.97027773754922,0.,1.36999806084573));
#36880=CARTESIAN_POINT('',(4.01728681790024,1.,1.22531898815164));
#36881=CARTESIAN_POINT('Origin',(0.,0.,0.));
#36882=CARTESIAN_POINT('',(3.42859860294378,1.,1.51895082866166));
#36883=CARTESIAN_POINT('Origin',(0.,1.,0.));
#36884=CARTESIAN_POINT('Ctrl Pts',(3.42859860294378,1.,1.51895082866166));
#36885=CARTESIAN_POINT('Ctrl Pts',(3.42859860294378,0.666666666666667,1.51895082866166));
#36886=CARTESIAN_POINT('Ctrl Pts',(3.42859860294378,0.333333333333333,1.51895082866166));
#36887=CARTESIAN_POINT('Ctrl Pts',(3.42859860294378,-0.333333333333333,
1.51895082866166));
#36888=CARTESIAN_POINT('Ctrl Pts',(3.42859860294378,-0.666666666666667,
1.51895082866166));
#36889=CARTESIAN_POINT('Ctrl Pts',(3.42859860294378,-1.,1.51895082866166));
#36890=CARTESIAN_POINT('Ctrl Pts',(3.77614523045147,-1.,1.83867539237861));
#36891=CARTESIAN_POINT('Ctrl Pts',(3.77614523045147,1.,1.83867539237861));
#36892=CARTESIAN_POINT('Ctrl Pts',(3.77518714458232,-1.,1.83742834010821));
#36893=CARTESIAN_POINT('Ctrl Pts',(3.77518714458232,1.,1.83742834010821));
#36894=CARTESIAN_POINT('Ctrl Pts',(3.77326886065484,-1.,1.83493697935064));
#36895=CARTESIAN_POINT('Ctrl Pts',(3.77326886065484,1.,1.83493697935064));
#36896=CARTESIAN_POINT('Ctrl Pts',(3.77038509819777,-1.,1.83120816956515));
#36897=CARTESIAN_POINT('Ctrl Pts',(3.77038509819777,1.,1.83120816956515));
#36898=CARTESIAN_POINT('Ctrl Pts',(3.76652740355856,-1.,1.82625289221933));
#36899=CARTESIAN_POINT('Ctrl Pts',(3.76652740355856,1.,1.82625289221933));
#36900=CARTESIAN_POINT('Ctrl Pts',(3.76168412709652,-1.,1.82008629694924));
#36901=CARTESIAN_POINT('Ctrl Pts',(3.76168412709652,1.,1.82008629694924));
#36902=CARTESIAN_POINT('Ctrl Pts',(3.75681965683995,-1.,1.81394729834032));
#36903=CARTESIAN_POINT('Ctrl Pts',(3.75681965683995,1.,1.81394729834032));
#36904=CARTESIAN_POINT('Ctrl Pts',(3.75193395888069,-1.,1.80783603939662));
#36905=CARTESIAN_POINT('Ctrl Pts',(3.75193395888069,1.,1.80783603939662));
#36906=CARTESIAN_POINT('Ctrl Pts',(3.74702700874954,-1.,1.80175271485519));
#36907=CARTESIAN_POINT('Ctrl Pts',(3.74702700874954,1.,1.80175271485519));
#36908=CARTESIAN_POINT('Ctrl Pts',(3.74209880351667,-1.,1.79569757859041));
#36909=CARTESIAN_POINT('Ctrl Pts',(3.74209880351667,1.,1.79569757859041));
#36910=CARTESIAN_POINT('Ctrl Pts',(3.73714934729962,-1.,1.78967092823139));
#36911=CARTESIAN_POINT('Ctrl Pts',(3.73714934729962,1.,1.78967092823139));
#36912=CARTESIAN_POINT('Ctrl Pts',(3.73217863095022,-1.,1.78367308442682));
#36913=CARTESIAN_POINT('Ctrl Pts',(3.73217863095022,1.,1.78367308442682));
#36914=CARTESIAN_POINT('Ctrl Pts',(3.72718661205504,-1.,1.77770437039606));
#36915=CARTESIAN_POINT('Ctrl Pts',(3.72718661205504,1.,1.77770437039606));
#36916=CARTESIAN_POINT('Ctrl Pts',(3.72217319911429,-1.,1.77176509401846));
#36917=CARTESIAN_POINT('Ctrl Pts',(3.72217319911429,1.,1.77176509401846));
#36918=CARTESIAN_POINT('Ctrl Pts',(3.71713822377675,-1.,1.76585552124549));
#36919=CARTESIAN_POINT('Ctrl Pts',(3.71713822377675,1.,1.76585552124549));
#36920=CARTESIAN_POINT('Ctrl Pts',(3.71208146346454,-1.,1.75997588499021));
#36921=CARTESIAN_POINT('Ctrl Pts',(3.71208146346454,1.,1.75997588499021));
#36922=CARTESIAN_POINT('Ctrl Pts',(3.70700269736876,-1.,1.75412641804148));
#36923=CARTESIAN_POINT('Ctrl Pts',(3.70700269736876,1.,1.75412641804148));
#36924=CARTESIAN_POINT('Ctrl Pts',(3.70190175673422,-1.,1.74830738046092));
#36925=CARTESIAN_POINT('Ctrl Pts',(3.70190175673422,1.,1.74830738046092));
#36926=CARTESIAN_POINT('Ctrl Pts',(3.6967785691046,-1.,1.74251908492589));
#36927=CARTESIAN_POINT('Ctrl Pts',(3.6967785691046,1.,1.74251908492589));
#36928=CARTESIAN_POINT('Ctrl Pts',(3.69163322647906,-1.,1.73676193254493));
#36929=CARTESIAN_POINT('Ctrl Pts',(3.69163322647906,1.,1.73676193254493));
#36930=CARTESIAN_POINT('Ctrl Pts',(3.68646597019188,-1.,1.73103640956647));
#36931=CARTESIAN_POINT('Ctrl Pts',(3.68646597019188,1.,1.73103640956647));
#36932=CARTESIAN_POINT('Ctrl Pts',(3.68127704936472,-1.,1.72534302437003));
#36933=CARTESIAN_POINT('Ctrl Pts',(3.68127704936472,1.,1.72534302437003));
#36934=CARTESIAN_POINT('Ctrl Pts',(3.67606660374665,-1.,1.71968225581787));
#36935=CARTESIAN_POINT('Ctrl Pts',(3.67606660374665,1.,1.71968225581787));
#36936=CARTESIAN_POINT('Ctrl Pts',(3.67083454901629,-1.,1.71405450210392));
#36937=CARTESIAN_POINT('Ctrl Pts',(3.67083454901629,1.,1.71405450210392));
#36938=CARTESIAN_POINT('Ctrl Pts',(3.6655804319893,-1.,1.70846001610983));
#36939=CARTESIAN_POINT('Ctrl Pts',(3.6655804319893,1.,1.70846001610983));
#36940=CARTESIAN_POINT('Ctrl Pts',(3.6603033877491,-1.,1.70289888566904));
#36941=CARTESIAN_POINT('Ctrl Pts',(3.6603033877491,1.,1.70289888566904));
#36942=CARTESIAN_POINT('Ctrl Pts',(3.65500246526798,-1.,1.69737117722559));
#36943=CARTESIAN_POINT('Ctrl Pts',(3.65500246526798,1.,1.69737117722559));
#36944=CARTESIAN_POINT('Ctrl Pts',(3.64967689827393,-1.,1.691877054817));
#36945=CARTESIAN_POINT('Ctrl Pts',(3.64967689827393,1.,1.691877054817));
#36946=CARTESIAN_POINT('Ctrl Pts',(3.64432638915199,-1.,1.68641690471455));
#36947=CARTESIAN_POINT('Ctrl Pts',(3.64432638915199,1.,1.68641690471455));
#36948=CARTESIAN_POINT('Ctrl Pts',(3.63895140887443,-1.,1.68099146651577));
#36949=CARTESIAN_POINT('Ctrl Pts',(3.63895140887443,1.,1.68099146651577));
#36950=CARTESIAN_POINT('Ctrl Pts',(3.63355343201211,-1.,1.67560193613145));
#36951=CARTESIAN_POINT('Ctrl Pts',(3.63355343201211,1.,1.67560193613145));
#36952=CARTESIAN_POINT('Ctrl Pts',(3.62813422105257,-1.,1.67024966008037));
#36953=CARTESIAN_POINT('Ctrl Pts',(3.62813422105257,1.,1.67024966008037));
#36954=CARTESIAN_POINT('Ctrl Pts',(3.62269517989104,-1.,1.66493585923853));
#36955=CARTESIAN_POINT('Ctrl Pts',(3.62269517989104,1.,1.66493585923853));
#36956=CARTESIAN_POINT('Ctrl Pts',(3.61723666482457,-1.,1.65966133399186));
#36957=CARTESIAN_POINT('Ctrl Pts',(3.61723666482457,1.,1.65966133399186));
#36958=CARTESIAN_POINT('Ctrl Pts',(3.61175734965129,-1.,1.65442619244327));
#36959=CARTESIAN_POINT('Ctrl Pts',(3.61175734965129,1.,1.65442619244327));
#36960=CARTESIAN_POINT('Ctrl Pts',(3.60625346556992,-1.,1.64922952425833));
#36961=CARTESIAN_POINT('Ctrl Pts',(3.60625346556992,1.,1.64922952425833));
#36962=CARTESIAN_POINT('Ctrl Pts',(3.6007202851384,-1.,1.6440700438558));
#36963=CARTESIAN_POINT('Ctrl Pts',(3.6007202851384,1.,1.6440700438558));
#36964=CARTESIAN_POINT('Ctrl Pts',(3.59515368334887,-1.,1.63894676675349));
#36965=CARTESIAN_POINT('Ctrl Pts',(3.59515368334887,1.,1.63894676675349));
#36966=CARTESIAN_POINT('Ctrl Pts',(3.58955176627876,-1.,1.63385971451259));
#36967=CARTESIAN_POINT('Ctrl Pts',(3.58955176627876,1.,1.63385971451259));
#36968=CARTESIAN_POINT('Ctrl Pts',(3.5839162577435,-1.,1.62881051550748));
#36969=CARTESIAN_POINT('Ctrl Pts',(3.5839162577435,1.,1.62881051550748));
#36970=CARTESIAN_POINT('Ctrl Pts',(3.57825455954405,-1.,1.62380329464851));
#36971=CARTESIAN_POINT('Ctrl Pts',(3.57825455954405,1.,1.62380329464851));
#36972=CARTESIAN_POINT('Ctrl Pts',(3.57257679609826,-1.,1.61884340915412));
#36973=CARTESIAN_POINT('Ctrl Pts',(3.57257679609826,1.,1.61884340915412));
#36974=CARTESIAN_POINT('Ctrl Pts',(3.56689200468404,-1.,1.61393581747522));
#36975=CARTESIAN_POINT('Ctrl Pts',(3.56689200468404,1.,1.61393581747522));
#36976=CARTESIAN_POINT('Ctrl Pts',(3.56120432482986,-1.,1.60908344685459));
#36977=CARTESIAN_POINT('Ctrl Pts',(3.56120432482986,1.,1.60908344685459));
#36978=CARTESIAN_POINT('Ctrl Pts',(3.55550985096117,-1.,1.60428584699848));
#36979=CARTESIAN_POINT('Ctrl Pts',(3.55550985096117,1.,1.60428584699848));
#36980=CARTESIAN_POINT('Ctrl Pts',(3.54979148634426,-1.,1.59953698113444));
#36981=CARTESIAN_POINT('Ctrl Pts',(3.54979148634426,1.,1.59953698113444));
#36982=CARTESIAN_POINT('Ctrl Pts',(3.544024581823,-1.,1.5948276694975));
#36983=CARTESIAN_POINT('Ctrl Pts',(3.544024581823,1.,1.5948276694975));
#36984=CARTESIAN_POINT('Ctrl Pts',(3.53818616861045,-1.,1.59014958368725));
#36985=CARTESIAN_POINT('Ctrl Pts',(3.53818616861045,1.,1.59014958368725));
#36986=CARTESIAN_POINT('Ctrl Pts',(3.53226378147068,-1.,1.58549906268083));
#36987=CARTESIAN_POINT('Ctrl Pts',(3.53226378147068,1.,1.58549906268083));
#36988=CARTESIAN_POINT('Ctrl Pts',(3.52626275334899,-1.,1.58088027227856));
#36989=CARTESIAN_POINT('Ctrl Pts',(3.52626275334899,1.,1.58088027227856));
#36990=CARTESIAN_POINT('Ctrl Pts',(3.52021847865961,-1.,1.5763104998818));
#36991=CARTESIAN_POINT('Ctrl Pts',(3.52021847865961,1.,1.5763104998818));
#36992=CARTESIAN_POINT('Ctrl Pts',(3.51418598431733,-1.,1.57181569799774));
#36993=CARTESIAN_POINT('Ctrl Pts',(3.51418598431733,1.,1.57181569799774));
#36994=CARTESIAN_POINT('Ctrl Pts',(3.50821771695427,-1.,1.56742097575041));
#36995=CARTESIAN_POINT('Ctrl Pts',(3.50821771695427,1.,1.56742097575041));
#36996=CARTESIAN_POINT('Ctrl Pts',(3.50234321621607,-1.,1.56314187758689));
#36997=CARTESIAN_POINT('Ctrl Pts',(3.50234321621607,1.,1.56314187758689));
#36998=CARTESIAN_POINT('Ctrl Pts',(3.49655185179623,-1.,1.55897703097859));
#36999=CARTESIAN_POINT('Ctrl Pts',(3.49655185179623,1.,1.55897703097859));
#37000=CARTESIAN_POINT('Ctrl Pts',(3.49076460877317,-1.,1.5548959590107));
#37001=CARTESIAN_POINT('Ctrl Pts',(3.49076460877317,1.,1.5548959590107));
#37002=CARTESIAN_POINT('Ctrl Pts',(3.48485155928414,-1.,1.55084702970382));
#37003=CARTESIAN_POINT('Ctrl Pts',(3.48485155928414,1.,1.55084702970382));
#37004=CARTESIAN_POINT('Ctrl Pts',(3.47868272898599,-1.,1.54678009290207));
#37005=CARTESIAN_POINT('Ctrl Pts',(3.47868272898599,1.,1.54678009290207));
#37006=CARTESIAN_POINT('Ctrl Pts',(3.47217189224576,-1.,1.54266605398152));
#37007=CARTESIAN_POINT('Ctrl Pts',(3.47217189224576,1.,1.54266605398152));
#37008=CARTESIAN_POINT('Ctrl Pts',(3.46531752207222,-1.,1.53851507915533));
#37009=CARTESIAN_POINT('Ctrl Pts',(3.46531752207222,1.,1.53851507915533));
#37010=CARTESIAN_POINT('Ctrl Pts',(3.45825932955273,-1.,1.53440195378902));
#37011=CARTESIAN_POINT('Ctrl Pts',(3.45825932955273,1.,1.53440195378902));
#37012=CARTESIAN_POINT('Ctrl Pts',(3.45127136828667,-1.,1.530462444618));
#37013=CARTESIAN_POINT('Ctrl Pts',(3.45127136828667,1.,1.530462444618));
#37014=CARTESIAN_POINT('Ctrl Pts',(3.44469547527,-1.,1.52686242875717));
#37015=CARTESIAN_POINT('Ctrl Pts',(3.44469547527,1.,1.52686242875717));
#37016=CARTESIAN_POINT('Ctrl Pts',(3.43888895974182,-1.,1.52377348950429));
#37017=CARTESIAN_POINT('Ctrl Pts',(3.43888895974182,1.,1.52377348950429));
#37018=CARTESIAN_POINT('Ctrl Pts',(3.43417156977749,-1.,1.52134826724227));
#37019=CARTESIAN_POINT('Ctrl Pts',(3.43417156977749,1.,1.52134826724227));
#37020=CARTESIAN_POINT('Ctrl Pts',(3.43076036253384,-1.,1.51969006980792));
#37021=CARTESIAN_POINT('Ctrl Pts',(3.43076036253384,1.,1.51969006980792));
#37022=CARTESIAN_POINT('Ctrl Pts',(3.42915787669388,-1.,1.51901585838879));
#37023=CARTESIAN_POINT('Ctrl Pts',(3.42915787669388,1.,1.51901585838879));
#37024=CARTESIAN_POINT('Ctrl Pts',(3.42860527148835,-1.,1.51888450659497));
#37025=CARTESIAN_POINT('Ctrl Pts',(3.42860527148835,1.,1.51888450659497));
#37026=CARTESIAN_POINT('Ctrl Pts',(3.42852521763648,-1.,1.51896318668306));
#37027=CARTESIAN_POINT('Ctrl Pts',(3.42852521763648,1.,1.51896318668306));
#37028=CARTESIAN_POINT('Ctrl Pts',(3.42855728381368,-1.,1.519044091397));
#37029=CARTESIAN_POINT('Ctrl Pts',(3.42855728381368,1.,1.519044091397));
#37030=CARTESIAN_POINT('',(3.77614523045147,1.,1.83867539237861));
#37031=CARTESIAN_POINT('Ctrl Pts',(3.77614523045147,1.,1.83867539237861));
#37032=CARTESIAN_POINT('Ctrl Pts',(3.77518714458232,1.,1.83742834010821));
#37033=CARTESIAN_POINT('Ctrl Pts',(3.77326886065484,1.,1.83493697935064));
#37034=CARTESIAN_POINT('Ctrl Pts',(3.77038509819777,1.,1.83120816956515));
#37035=CARTESIAN_POINT('Ctrl Pts',(3.76652740355856,1.,1.82625289221933));
#37036=CARTESIAN_POINT('Ctrl Pts',(3.76168412709652,1.,1.82008629694924));
#37037=CARTESIAN_POINT('Ctrl Pts',(3.75681965683995,1.,1.81394729834032));
#37038=CARTESIAN_POINT('Ctrl Pts',(3.75193395888069,1.,1.80783603939662));
#37039=CARTESIAN_POINT('Ctrl Pts',(3.74702700874954,1.,1.80175271485519));
#37040=CARTESIAN_POINT('Ctrl Pts',(3.74209880351667,1.,1.79569757859041));
#37041=CARTESIAN_POINT('Ctrl Pts',(3.73714934729962,1.,1.78967092823139));
#37042=CARTESIAN_POINT('Ctrl Pts',(3.73217863095022,1.,1.78367308442682));
#37043=CARTESIAN_POINT('Ctrl Pts',(3.72718661205504,1.,1.77770437039606));
#37044=CARTESIAN_POINT('Ctrl Pts',(3.72217319911429,1.,1.77176509401846));
#37045=CARTESIAN_POINT('Ctrl Pts',(3.71713822377675,1.,1.76585552124549));
#37046=CARTESIAN_POINT('Ctrl Pts',(3.71208146346454,1.,1.75997588499021));
#37047=CARTESIAN_POINT('Ctrl Pts',(3.70700269736876,1.,1.75412641804148));
#37048=CARTESIAN_POINT('Ctrl Pts',(3.70190175673422,1.,1.74830738046092));
#37049=CARTESIAN_POINT('Ctrl Pts',(3.6967785691046,1.,1.74251908492589));
#37050=CARTESIAN_POINT('Ctrl Pts',(3.69163322647906,1.,1.73676193254493));
#37051=CARTESIAN_POINT('Ctrl Pts',(3.68646597019188,1.,1.73103640956647));
#37052=CARTESIAN_POINT('Ctrl Pts',(3.68127704936472,1.,1.72534302437003));
#37053=CARTESIAN_POINT('Ctrl Pts',(3.67606660374665,1.,1.71968225581787));
#37054=CARTESIAN_POINT('Ctrl Pts',(3.67083454901629,1.,1.71405450210392));
#37055=CARTESIAN_POINT('Ctrl Pts',(3.6655804319893,1.,1.70846001610983));
#37056=CARTESIAN_POINT('Ctrl Pts',(3.6603033877491,1.,1.70289888566904));
#37057=CARTESIAN_POINT('Ctrl Pts',(3.65500246526798,1.,1.69737117722559));
#37058=CARTESIAN_POINT('Ctrl Pts',(3.64967689827393,1.,1.691877054817));
#37059=CARTESIAN_POINT('Ctrl Pts',(3.64432638915199,1.,1.68641690471455));
#37060=CARTESIAN_POINT('Ctrl Pts',(3.63895140887443,1.,1.68099146651577));
#37061=CARTESIAN_POINT('Ctrl Pts',(3.63355343201211,1.,1.67560193613145));
#37062=CARTESIAN_POINT('Ctrl Pts',(3.62813422105257,1.,1.67024966008037));
#37063=CARTESIAN_POINT('Ctrl Pts',(3.62269517989104,1.,1.66493585923853));
#37064=CARTESIAN_POINT('Ctrl Pts',(3.61723666482457,1.,1.65966133399186));
#37065=CARTESIAN_POINT('Ctrl Pts',(3.61175734965129,1.,1.65442619244327));
#37066=CARTESIAN_POINT('Ctrl Pts',(3.60625346556992,1.,1.64922952425833));
#37067=CARTESIAN_POINT('Ctrl Pts',(3.6007202851384,1.,1.6440700438558));
#37068=CARTESIAN_POINT('Ctrl Pts',(3.59515368334887,1.,1.63894676675349));
#37069=CARTESIAN_POINT('Ctrl Pts',(3.58955176627876,1.,1.63385971451259));
#37070=CARTESIAN_POINT('Ctrl Pts',(3.5839162577435,1.,1.62881051550748));
#37071=CARTESIAN_POINT('Ctrl Pts',(3.57825455954405,1.,1.62380329464851));
#37072=CARTESIAN_POINT('Ctrl Pts',(3.57257679609826,1.,1.61884340915412));
#37073=CARTESIAN_POINT('Ctrl Pts',(3.56689200468404,1.,1.61393581747522));
#37074=CARTESIAN_POINT('Ctrl Pts',(3.56120432482986,1.,1.60908344685459));
#37075=CARTESIAN_POINT('Ctrl Pts',(3.55550985096117,1.,1.60428584699848));
#37076=CARTESIAN_POINT('Ctrl Pts',(3.54979148634426,1.,1.59953698113444));
#37077=CARTESIAN_POINT('Ctrl Pts',(3.544024581823,1.,1.5948276694975));
#37078=CARTESIAN_POINT('Ctrl Pts',(3.53818616861045,1.,1.59014958368725));
#37079=CARTESIAN_POINT('Ctrl Pts',(3.53226378147068,1.,1.58549906268083));
#37080=CARTESIAN_POINT('Ctrl Pts',(3.52626275334899,1.,1.58088027227856));
#37081=CARTESIAN_POINT('Ctrl Pts',(3.52021847865961,1.,1.5763104998818));
#37082=CARTESIAN_POINT('Ctrl Pts',(3.51418598431733,1.,1.57181569799774));
#37083=CARTESIAN_POINT('Ctrl Pts',(3.50821771695427,1.,1.56742097575041));
#37084=CARTESIAN_POINT('Ctrl Pts',(3.50234321621607,1.,1.56314187758689));
#37085=CARTESIAN_POINT('Ctrl Pts',(3.49655185179623,1.,1.55897703097859));
#37086=CARTESIAN_POINT('Ctrl Pts',(3.49076460877317,1.,1.5548959590107));
#37087=CARTESIAN_POINT('Ctrl Pts',(3.48485155928414,1.,1.55084702970382));
#37088=CARTESIAN_POINT('Ctrl Pts',(3.47868272898599,1.,1.54678009290207));
#37089=CARTESIAN_POINT('Ctrl Pts',(3.47217189224576,1.,1.54266605398152));
#37090=CARTESIAN_POINT('Ctrl Pts',(3.46531752207222,1.,1.53851507915533));
#37091=CARTESIAN_POINT('Ctrl Pts',(3.45825932955273,1.,1.53440195378902));
#37092=CARTESIAN_POINT('Ctrl Pts',(3.45127136828667,1.,1.530462444618));
#37093=CARTESIAN_POINT('Ctrl Pts',(3.44469547527,1.,1.52686242875717));
#37094=CARTESIAN_POINT('Ctrl Pts',(3.43888895974182,1.,1.52377348950429));
#37095=CARTESIAN_POINT('Ctrl Pts',(3.43417156977749,1.,1.52134826724227));
#37096=CARTESIAN_POINT('Ctrl Pts',(3.4310163189349,1.,1.5198144909343));
#37097=CARTESIAN_POINT('Ctrl Pts',(3.42946838852728,1.,1.51914806898539));
#37098=CARTESIAN_POINT('Ctrl Pts',(3.42884302333978,1.,1.51895133295017));
#37099=CARTESIAN_POINT('Ctrl Pts',(3.42864616361967,1.,1.51893924967231));
#37100=CARTESIAN_POINT('Ctrl Pts',(3.42859860294378,1.,1.51895082866166));
#37101=CARTESIAN_POINT('',(3.77614523045147,0.,1.83867539237861));
#37102=CARTESIAN_POINT('Ctrl Pts',(3.24418789321065,-1.,1.88088939428811));
#37103=CARTESIAN_POINT('Ctrl Pts',(3.24418789321065,1.,1.88088939428811));
#37104=CARTESIAN_POINT('Ctrl Pts',(3.24410359189733,-1.,1.8809110068042));
#37105=CARTESIAN_POINT('Ctrl Pts',(3.24410359189733,1.,1.8809110068042));
#37106=CARTESIAN_POINT('Ctrl Pts',(3.24408699284449,-1.,1.8810220187274));
#37107=CARTESIAN_POINT('Ctrl Pts',(3.24408699284449,1.,1.8810220187274));
#37108=CARTESIAN_POINT('Ctrl Pts',(3.24451807186964,-1.,1.88139187908347));
#37109=CARTESIAN_POINT('Ctrl Pts',(3.24451807186964,1.,1.88139187908347));
#37110=CARTESIAN_POINT('Ctrl Pts',(3.24600543790876,-1.,1.88229202583187));
#37111=CARTESIAN_POINT('Ctrl Pts',(3.24600543790876,1.,1.88229202583187));
#37112=CARTESIAN_POINT('Ctrl Pts',(3.24935200512055,-1.,1.88407708646435));
#37113=CARTESIAN_POINT('Ctrl Pts',(3.24935200512055,1.,1.88407708646435));
#37114=CARTESIAN_POINT('Ctrl Pts',(3.25408686339298,-1.,1.88646802523372));
#37115=CARTESIAN_POINT('Ctrl Pts',(3.25408686339298,1.,1.88646802523372));
#37116=CARTESIAN_POINT('Ctrl Pts',(3.2599988519361,-1.,1.88934996203508));
#37117=CARTESIAN_POINT('Ctrl Pts',(3.2599988519361,1.,1.88934996203508));
#37118=CARTESIAN_POINT('Ctrl Pts',(3.2667765388833,-1.,1.89255393500769));
#37119=CARTESIAN_POINT('Ctrl Pts',(3.2667765388833,1.,1.89255393500769));
#37120=CARTESIAN_POINT('Ctrl Pts',(3.27407108932908,-1.,1.89589172903662));
#37121=CARTESIAN_POINT('Ctrl Pts',(3.27407108932908,1.,1.89589172903662));
#37122=CARTESIAN_POINT('Ctrl Pts',(3.28154737912287,-1.,1.89918429230425));
#37123=CARTESIAN_POINT('Ctrl Pts',(3.28154737912287,1.,1.89918429230425));
#37124=CARTESIAN_POINT('Ctrl Pts',(3.28893448600364,-1.,1.9022897124757));
#37125=CARTESIAN_POINT('Ctrl Pts',(3.28893448600364,1.,1.9022897124757));
#37126=CARTESIAN_POINT('Ctrl Pts',(3.29608978722258,-1.,1.9051389186417));
#37127=CARTESIAN_POINT('Ctrl Pts',(3.29608978722258,1.,1.9051389186417));
#37128=CARTESIAN_POINT('Ctrl Pts',(3.30300595568341,-1.,1.90773912171424));
#37129=CARTESIAN_POINT('Ctrl Pts',(3.30300595568341,1.,1.90773912171424));
#37130=CARTESIAN_POINT('Ctrl Pts',(3.30975721158694,-1.,1.91014297830502));
#37131=CARTESIAN_POINT('Ctrl Pts',(3.30975721158694,1.,1.91014297830502));
#37132=CARTESIAN_POINT('Ctrl Pts',(3.31646052426395,-1.,1.91242616234459));
#37133=CARTESIAN_POINT('Ctrl Pts',(3.31646052426395,1.,1.91242616234459));
#37134=CARTESIAN_POINT('Ctrl Pts',(3.32323403454507,-1.,1.91466343916612));
#37135=CARTESIAN_POINT('Ctrl Pts',(3.32323403454507,1.,1.91466343916612));
#37136=CARTESIAN_POINT('Ctrl Pts',(3.33014884257812,-1.,1.91690081930297));
#37137=CARTESIAN_POINT('Ctrl Pts',(3.33014884257812,1.,1.91690081930297));
#37138=CARTESIAN_POINT('Ctrl Pts',(3.33721230709948,-1.,1.91914609610173));
#37139=CARTESIAN_POINT('Ctrl Pts',(3.33721230709948,1.,1.91914609610173));
#37140=CARTESIAN_POINT('Ctrl Pts',(3.34439448941915,-1.,1.92138450828378));
#37141=CARTESIAN_POINT('Ctrl Pts',(3.34439448941915,1.,1.92138450828378));
#37142=CARTESIAN_POINT('Ctrl Pts',(3.35164424847206,-1.,1.92358838440518));
#37143=CARTESIAN_POINT('Ctrl Pts',(3.35164424847206,1.,1.92358838440518));
#37144=CARTESIAN_POINT('Ctrl Pts',(3.35890824422976,-1.,1.92572846125763));
#37145=CARTESIAN_POINT('Ctrl Pts',(3.35890824422976,1.,1.92572846125763));
#37146=CARTESIAN_POINT('Ctrl Pts',(3.36615168657597,-1.,1.92778626543803));
#37147=CARTESIAN_POINT('Ctrl Pts',(3.36615168657597,1.,1.92778626543803));
#37148=CARTESIAN_POINT('Ctrl Pts',(3.37336807068078,-1.,1.92975993109897));
#37149=CARTESIAN_POINT('Ctrl Pts',(3.37336807068078,1.,1.92975993109897));
#37150=CARTESIAN_POINT('Ctrl Pts',(3.38056768525577,-1.,1.93165739093292));
#37151=CARTESIAN_POINT('Ctrl Pts',(3.38056768525577,1.,1.93165739093292));
#37152=CARTESIAN_POINT('Ctrl Pts',(3.38777076883267,-1.,1.93349233176794));
#37153=CARTESIAN_POINT('Ctrl Pts',(3.38777076883267,1.,1.93349233176794));
#37154=CARTESIAN_POINT('Ctrl Pts',(3.39499923640789,-1.,1.93527929945982));
#37155=CARTESIAN_POINT('Ctrl Pts',(3.39499923640789,1.,1.93527929945982));
#37156=CARTESIAN_POINT('Ctrl Pts',(3.40226802104093,-1.,1.93702857723089));
#37157=CARTESIAN_POINT('Ctrl Pts',(3.40226802104093,1.,1.93702857723089));
#37158=CARTESIAN_POINT('Ctrl Pts',(3.40957978266622,-1.,1.93874306008132));
#37159=CARTESIAN_POINT('Ctrl Pts',(3.40957978266622,1.,1.93874306008132));
#37160=CARTESIAN_POINT('Ctrl Pts',(3.41692971994082,-1.,1.94042111965237));
#37161=CARTESIAN_POINT('Ctrl Pts',(3.41692971994082,1.,1.94042111965237));
#37162=CARTESIAN_POINT('Ctrl Pts',(3.42430850941497,-1.,1.94205835913692));
#37163=CARTESIAN_POINT('Ctrl Pts',(3.42430850941497,1.,1.94205835913692));
#37164=CARTESIAN_POINT('Ctrl Pts',(3.43170586602436,-1.,1.94364973660285));
#37165=CARTESIAN_POINT('Ctrl Pts',(3.43170586602436,1.,1.94364973660285));
#37166=CARTESIAN_POINT('Ctrl Pts',(3.43911410197693,-1.,1.94519168842883));
#37167=CARTESIAN_POINT('Ctrl Pts',(3.43911410197693,1.,1.94519168842883));
#37168=CARTESIAN_POINT('Ctrl Pts',(3.44653088665685,-1.,1.94668377715332));
#37169=CARTESIAN_POINT('Ctrl Pts',(3.44653088665685,1.,1.94668377715332));
#37170=CARTESIAN_POINT('Ctrl Pts',(3.45395731584051,-1.,1.94812754766524));
#37171=CARTESIAN_POINT('Ctrl Pts',(3.45395731584051,1.,1.94812754766524));
#37172=CARTESIAN_POINT('Ctrl Pts',(3.46139661060959,-1.,1.94952575850196));
#37173=CARTESIAN_POINT('Ctrl Pts',(3.46139661060959,1.,1.94952575850196));
#37174=CARTESIAN_POINT('Ctrl Pts',(3.4688525897419,-1.,1.95088147859876));
#37175=CARTESIAN_POINT('Ctrl Pts',(3.4688525897419,1.,1.95088147859876));
#37176=CARTESIAN_POINT('Ctrl Pts',(3.47632820495926,-1.,1.95219722189878));
#37177=CARTESIAN_POINT('Ctrl Pts',(3.47632820495926,1.,1.95219722189878));
#37178=CARTESIAN_POINT('Ctrl Pts',(3.48382414832648,-1.,1.95347412486316));
#37179=CARTESIAN_POINT('Ctrl Pts',(3.48382414832648,1.,1.95347412486316));
#37180=CARTESIAN_POINT('Ctrl Pts',(3.49133956289154,-1.,1.95471236969653));
#37181=CARTESIAN_POINT('Ctrl Pts',(3.49133956289154,1.,1.95471236969653));
#37182=CARTESIAN_POINT('Ctrl Pts',(3.49887263575602,-1.,1.9559115382367));
#37183=CARTESIAN_POINT('Ctrl Pts',(3.49887263575602,1.,1.9559115382367));
#37184=CARTESIAN_POINT('Ctrl Pts',(3.50642124159913,-1.,1.95707099606514));
#37185=CARTESIAN_POINT('Ctrl Pts',(3.50642124159913,1.,1.95707099606514));
#37186=CARTESIAN_POINT('Ctrl Pts',(3.51398354617772,-1.,1.95819025316768));
#37187=CARTESIAN_POINT('Ctrl Pts',(3.51398354617772,1.,1.95819025316768));
#37188=CARTESIAN_POINT('Ctrl Pts',(3.52155867431438,-1.,1.95926936324436));
#37189=CARTESIAN_POINT('Ctrl Pts',(3.52155867431438,1.,1.95926936324436));
#37190=CARTESIAN_POINT('Ctrl Pts',(3.52914648844289,-1.,1.96030879411534));
#37191=CARTESIAN_POINT('Ctrl Pts',(3.52914648844289,1.,1.96030879411534));
#37192=CARTESIAN_POINT('Ctrl Pts',(3.53674730625759,-1.,1.96130926212661));
#37193=CARTESIAN_POINT('Ctrl Pts',(3.53674730625759,1.,1.96130926212661));
#37194=CARTESIAN_POINT('Ctrl Pts',(3.54436163300425,-1.,1.96227157573058));
#37195=CARTESIAN_POINT('Ctrl Pts',(3.54436163300425,1.,1.96227157573058));
#37196=CARTESIAN_POINT('Ctrl Pts',(3.55198990600929,-1.,1.96319648628667));
#37197=CARTESIAN_POINT('Ctrl Pts',(3.55198990600929,1.,1.96319648628667));
#37198=CARTESIAN_POINT('Ctrl Pts',(3.55963218706201,-1.,1.96408450906868));
#37199=CARTESIAN_POINT('Ctrl Pts',(3.55963218706201,1.,1.96408450906868));
#37200=CARTESIAN_POINT('Ctrl Pts',(3.56728820357933,-1.,1.96493594634643));
#37201=CARTESIAN_POINT('Ctrl Pts',(3.56728820357933,1.,1.96493594634643));
#37202=CARTESIAN_POINT('Ctrl Pts',(3.57495748601088,-1.,1.96575096652857));
#37203=CARTESIAN_POINT('Ctrl Pts',(3.57495748601088,1.,1.96575096652857));
#37204=CARTESIAN_POINT('Ctrl Pts',(3.58263947663884,-1.,1.9665296668894));
#37205=CARTESIAN_POINT('Ctrl Pts',(3.58263947663884,1.,1.9665296668894));
#37206=CARTESIAN_POINT('Ctrl Pts',(3.5903336402273,-1.,1.96727213799507));
#37207=CARTESIAN_POINT('Ctrl Pts',(3.5903336402273,1.,1.96727213799507));
#37208=CARTESIAN_POINT('Ctrl Pts',(3.59803959819725,-1.,1.96797854118257));
#37209=CARTESIAN_POINT('Ctrl Pts',(3.59803959819725,1.,1.96797854118257));
#37210=CARTESIAN_POINT('Ctrl Pts',(3.60575714017676,-1.,1.96864911885775));
#37211=CARTESIAN_POINT('Ctrl Pts',(3.60575714017676,1.,1.96864911885775));
#37212=CARTESIAN_POINT('Ctrl Pts',(3.61348615496393,-1.,1.96928416040712));
#37213=CARTESIAN_POINT('Ctrl Pts',(3.61348615496393,1.,1.96928416040712));
#37214=CARTESIAN_POINT('Ctrl Pts',(3.62122658401722,-1.,1.96988398129888));
#37215=CARTESIAN_POINT('Ctrl Pts',(3.62122658401722,1.,1.96988398129888));
#37216=CARTESIAN_POINT('Ctrl Pts',(3.62897836973397,-1.,1.97044889850518));
#37217=CARTESIAN_POINT('Ctrl Pts',(3.62897836973397,1.,1.97044889850518));
#37218=CARTESIAN_POINT('Ctrl Pts',(3.63674139590853,-1.,1.97097920454698));
#37219=CARTESIAN_POINT('Ctrl Pts',(3.63674139590853,1.,1.97097920454698));
#37220=CARTESIAN_POINT('Ctrl Pts',(3.64451546724221,-1.,1.97147515441539));
#37221=CARTESIAN_POINT('Ctrl Pts',(3.64451546724221,1.,1.97147515441539));
#37222=CARTESIAN_POINT('Ctrl Pts',(3.65230034717364,-1.,1.97193697240645));
#37223=CARTESIAN_POINT('Ctrl Pts',(3.65230034717364,1.,1.97193697240645));
#37224=CARTESIAN_POINT('Ctrl Pts',(3.66009578166865,-1.,1.97236485439317));
#37225=CARTESIAN_POINT('Ctrl Pts',(3.66009578166865,1.,1.97236485439317));
#37226=CARTESIAN_POINT('Ctrl Pts',(3.66790152751984,-1.,1.9727589719863));
#37227=CARTESIAN_POINT('Ctrl Pts',(3.66790152751984,1.,1.9727589719863));
#37228=CARTESIAN_POINT('Ctrl Pts',(3.67571738106175,-1.,1.97311947678035));
#37229=CARTESIAN_POINT('Ctrl Pts',(3.67571738106175,1.,1.97311947678035));
#37230=CARTESIAN_POINT('Ctrl Pts',(3.68354319913416,-1.,1.97344650303631));
#37231=CARTESIAN_POINT('Ctrl Pts',(3.68354319913416,1.,1.97344650303631));
#37232=CARTESIAN_POINT('Ctrl Pts',(3.69137888597855,-1.,1.97374016224397));
#37233=CARTESIAN_POINT('Ctrl Pts',(3.69137888597855,1.,1.97374016224397));
#37234=CARTESIAN_POINT('Ctrl Pts',(3.69765528558292,-1.,1.97394846382289));
#37235=CARTESIAN_POINT('Ctrl Pts',(3.69765528558292,1.,1.97394846382289));
#37236=CARTESIAN_POINT('Ctrl Pts',(3.70236698911837,-1.,1.97408973726149));
#37237=CARTESIAN_POINT('Ctrl Pts',(3.70236698911837,1.,1.97408973726149));
#37238=CARTESIAN_POINT('Ctrl Pts',(3.7055100813194,-1.,1.974177276451));
#37239=CARTESIAN_POINT('Ctrl Pts',(3.7055100813194,1.,1.974177276451));
#37240=CARTESIAN_POINT('Ctrl Pts',(3.70708211654725,-1.,1.97421938526992));
#37241=CARTESIAN_POINT('Ctrl Pts',(3.70708211654725,1.,1.97421938526992));
#37242=CARTESIAN_POINT('',(3.24413672884902,1.,1.88097764062542));
#37243=CARTESIAN_POINT('Ctrl Pts',(3.24413672884902,-1.,1.88097764062542));
#37244=CARTESIAN_POINT('Ctrl Pts',(3.24413672884902,-0.666666666666667,
1.88097764062542));
#37245=CARTESIAN_POINT('Ctrl Pts',(3.24413672884902,-0.333333333333333,
1.88097764062542));
#37246=CARTESIAN_POINT('Ctrl Pts',(3.24413672884902,0.333333333333333,1.88097764062542));
#37247=CARTESIAN_POINT('Ctrl Pts',(3.24413672884902,0.666666666666667,1.88097764062541));
#37248=CARTESIAN_POINT('Ctrl Pts',(3.24413672884902,1.,1.88097764062541));
#37249=CARTESIAN_POINT('',(3.70708211654725,1.,1.97421938526992));
#37250=CARTESIAN_POINT('',(3.70708211654725,0.,1.97421938526992));
#37251=CARTESIAN_POINT('Ctrl Pts',(3.24413672884902,1.,1.88097764062542));
#37252=CARTESIAN_POINT('Ctrl Pts',(3.24415531671311,1.,1.88102292397987));
#37253=CARTESIAN_POINT('Ctrl Pts',(3.24428080352952,1.,1.88117508446657));
#37254=CARTESIAN_POINT('Ctrl Pts',(3.24480754675942,1.,1.88156537699118));
#37255=CARTESIAN_POINT('Ctrl Pts',(3.24625654410705,1.,1.88242596600422));
#37256=CARTESIAN_POINT('Ctrl Pts',(3.24935200512055,1.,1.88407708646435));
#37257=CARTESIAN_POINT('Ctrl Pts',(3.25408686339298,1.,1.88646802523372));
#37258=CARTESIAN_POINT('Ctrl Pts',(3.2599988519361,1.,1.88934996203508));
#37259=CARTESIAN_POINT('Ctrl Pts',(3.2667765388833,1.,1.89255393500769));
#37260=CARTESIAN_POINT('Ctrl Pts',(3.27407108932908,1.,1.89589172903662));
#37261=CARTESIAN_POINT('Ctrl Pts',(3.28154737912287,1.,1.89918429230425));
#37262=CARTESIAN_POINT('Ctrl Pts',(3.28893448600364,1.,1.9022897124757));
#37263=CARTESIAN_POINT('Ctrl Pts',(3.29608978722258,1.,1.9051389186417));
#37264=CARTESIAN_POINT('Ctrl Pts',(3.30300595568341,1.,1.90773912171424));
#37265=CARTESIAN_POINT('Ctrl Pts',(3.30975721158694,1.,1.91014297830502));
#37266=CARTESIAN_POINT('Ctrl Pts',(3.31646052426395,1.,1.91242616234459));
#37267=CARTESIAN_POINT('Ctrl Pts',(3.32323403454507,1.,1.91466343916612));
#37268=CARTESIAN_POINT('Ctrl Pts',(3.33014884257812,1.,1.91690081930297));
#37269=CARTESIAN_POINT('Ctrl Pts',(3.33721230709948,1.,1.91914609610173));
#37270=CARTESIAN_POINT('Ctrl Pts',(3.34439448941915,1.,1.92138450828378));
#37271=CARTESIAN_POINT('Ctrl Pts',(3.35164424847206,1.,1.92358838440518));
#37272=CARTESIAN_POINT('Ctrl Pts',(3.35890824422976,1.,1.92572846125763));
#37273=CARTESIAN_POINT('Ctrl Pts',(3.36615168657597,1.,1.92778626543803));
#37274=CARTESIAN_POINT('Ctrl Pts',(3.37336807068078,1.,1.92975993109897));
#37275=CARTESIAN_POINT('Ctrl Pts',(3.38056768525577,1.,1.93165739093292));
#37276=CARTESIAN_POINT('Ctrl Pts',(3.38777076883267,1.,1.93349233176794));
#37277=CARTESIAN_POINT('Ctrl Pts',(3.39499923640789,1.,1.93527929945982));
#37278=CARTESIAN_POINT('Ctrl Pts',(3.40226802104093,1.,1.93702857723089));
#37279=CARTESIAN_POINT('Ctrl Pts',(3.40957978266622,1.,1.93874306008132));
#37280=CARTESIAN_POINT('Ctrl Pts',(3.41692971994082,1.,1.94042111965237));
#37281=CARTESIAN_POINT('Ctrl Pts',(3.42430850941497,1.,1.94205835913692));
#37282=CARTESIAN_POINT('Ctrl Pts',(3.43170586602436,1.,1.94364973660285));
#37283=CARTESIAN_POINT('Ctrl Pts',(3.43911410197693,1.,1.94519168842883));
#37284=CARTESIAN_POINT('Ctrl Pts',(3.44653088665685,1.,1.94668377715332));
#37285=CARTESIAN_POINT('Ctrl Pts',(3.45395731584051,1.,1.94812754766524));
#37286=CARTESIAN_POINT('Ctrl Pts',(3.46139661060959,1.,1.94952575850196));
#37287=CARTESIAN_POINT('Ctrl Pts',(3.4688525897419,1.,1.95088147859876));
#37288=CARTESIAN_POINT('Ctrl Pts',(3.47632820495926,1.,1.95219722189878));
#37289=CARTESIAN_POINT('Ctrl Pts',(3.48382414832648,1.,1.95347412486316));
#37290=CARTESIAN_POINT('Ctrl Pts',(3.49133956289154,1.,1.95471236969653));
#37291=CARTESIAN_POINT('Ctrl Pts',(3.49887263575602,1.,1.9559115382367));
#37292=CARTESIAN_POINT('Ctrl Pts',(3.50642124159913,1.,1.95707099606514));
#37293=CARTESIAN_POINT('Ctrl Pts',(3.51398354617772,1.,1.95819025316768));
#37294=CARTESIAN_POINT('Ctrl Pts',(3.52155867431438,1.,1.95926936324436));
#37295=CARTESIAN_POINT('Ctrl Pts',(3.52914648844289,1.,1.96030879411534));
#37296=CARTESIAN_POINT('Ctrl Pts',(3.53674730625759,1.,1.96130926212661));
#37297=CARTESIAN_POINT('Ctrl Pts',(3.54436163300425,1.,1.96227157573058));
#37298=CARTESIAN_POINT('Ctrl Pts',(3.55198990600929,1.,1.96319648628667));
#37299=CARTESIAN_POINT('Ctrl Pts',(3.55963218706201,1.,1.96408450906868));
#37300=CARTESIAN_POINT('Ctrl Pts',(3.56728820357933,1.,1.96493594634643));
#37301=CARTESIAN_POINT('Ctrl Pts',(3.57495748601088,1.,1.96575096652857));
#37302=CARTESIAN_POINT('Ctrl Pts',(3.58263947663884,1.,1.9665296668894));
#37303=CARTESIAN_POINT('Ctrl Pts',(3.5903336402273,1.,1.96727213799507));
#37304=CARTESIAN_POINT('Ctrl Pts',(3.59803959819725,1.,1.96797854118257));
#37305=CARTESIAN_POINT('Ctrl Pts',(3.60575714017676,1.,1.96864911885775));
#37306=CARTESIAN_POINT('Ctrl Pts',(3.61348615496393,1.,1.96928416040712));
#37307=CARTESIAN_POINT('Ctrl Pts',(3.62122658401722,1.,1.96988398129888));
#37308=CARTESIAN_POINT('Ctrl Pts',(3.62897836973397,1.,1.97044889850518));
#37309=CARTESIAN_POINT('Ctrl Pts',(3.63674139590853,1.,1.97097920454698));
#37310=CARTESIAN_POINT('Ctrl Pts',(3.64451546724221,1.,1.97147515441539));
#37311=CARTESIAN_POINT('Ctrl Pts',(3.65230034717364,1.,1.97193697240645));
#37312=CARTESIAN_POINT('Ctrl Pts',(3.66009578166865,1.,1.97236485439317));
#37313=CARTESIAN_POINT('Ctrl Pts',(3.66790152751984,1.,1.9727589719863));
#37314=CARTESIAN_POINT('Ctrl Pts',(3.67571738106175,1.,1.97311947678035));
#37315=CARTESIAN_POINT('Ctrl Pts',(3.68354319913416,1.,1.97344650303631));
#37316=CARTESIAN_POINT('Ctrl Pts',(3.69137888597855,1.,1.97374016224397));
#37317=CARTESIAN_POINT('Ctrl Pts',(3.69765528558292,1.,1.97394846382289));
#37318=CARTESIAN_POINT('Ctrl Pts',(3.70236698911837,1.,1.97408973726149));
#37319=CARTESIAN_POINT('Ctrl Pts',(3.7055100813194,1.,1.974177276451));
#37320=CARTESIAN_POINT('Ctrl Pts',(3.70708211654725,1.,1.97421938526992));
#37321=CARTESIAN_POINT('Origin',(3.70708211654725,0.,1.97421938526992));
#37322=CARTESIAN_POINT('',(3.77614523045147,1.,1.83867539237861));
#37323=CARTESIAN_POINT('Origin',(0.,0.,0.));
#37324=CARTESIAN_POINT('',(3.14877060440425,1.,2.03660101169564));
#37325=CARTESIAN_POINT('Origin',(0.,1.,0.));
#37326=CARTESIAN_POINT('Ctrl Pts',(3.14877060440425,1.,2.03660101169564));
#37327=CARTESIAN_POINT('Ctrl Pts',(3.14877060440425,0.666666666666667,2.03660101169564));
#37328=CARTESIAN_POINT('Ctrl Pts',(3.14877060440425,0.333333333333333,2.03660101169564));
#37329=CARTESIAN_POINT('Ctrl Pts',(3.14877060440425,-0.333333333333333,
2.03660101169564));
#37330=CARTESIAN_POINT('Ctrl Pts',(3.14877060440425,-0.666666666666667,
2.03660101169564));
#37331=CARTESIAN_POINT('Ctrl Pts',(3.14877060440425,-1.,2.03660101169564));
#37332=CARTESIAN_POINT('Ctrl Pts',(3.44202241512147,-1.,2.40675750623143));
#37333=CARTESIAN_POINT('Ctrl Pts',(3.44202241512147,1.,2.40675750623143));
#37334=CARTESIAN_POINT('Ctrl Pts',(3.44127120683402,-1.,2.40537592959345));
#37335=CARTESIAN_POINT('Ctrl Pts',(3.44127120683402,1.,2.40537592959345));
#37336=CARTESIAN_POINT('Ctrl Pts',(3.43976627485223,-1.,2.40261515590099));
#37337=CARTESIAN_POINT('Ctrl Pts',(3.43976627485223,1.,2.40261515590099));
#37338=CARTESIAN_POINT('Ctrl Pts',(3.43750133066036,-1.,2.39848113411429));
#37339=CARTESIAN_POINT('Ctrl Pts',(3.43750133066036,1.,2.39848113411429));
#37340=CARTESIAN_POINT('Ctrl Pts',(3.43446630680436,-1.,2.39298338805823));
#37341=CARTESIAN_POINT('Ctrl Pts',(3.43446630680436,1.,2.39298338805823));
#37342=CARTESIAN_POINT('Ctrl Pts',(3.43064732714472,-1.,2.38613505844641));
#37343=CARTESIAN_POINT('Ctrl Pts',(3.43064732714472,1.,2.38613505844641));
#37344=CARTESIAN_POINT('Ctrl Pts',(3.42680309755241,-1.,2.37931067029517));
#37345=CARTESIAN_POINT('Ctrl Pts',(3.42680309755241,1.,2.37931067029517));
#37346=CARTESIAN_POINT('Ctrl Pts',(3.42293356216595,-1.,2.37251035954351));
#37347=CARTESIAN_POINT('Ctrl Pts',(3.42293356216595,1.,2.37251035954351));
#37348=CARTESIAN_POINT('Ctrl Pts',(3.41903866635384,-1.,2.36573431470314));
#37349=CARTESIAN_POINT('Ctrl Pts',(3.41903866635384,1.,2.36573431470314));
#37350=CARTESIAN_POINT('Ctrl Pts',(3.4151183675076,-1.,2.35898278606449));
#37351=CARTESIAN_POINT('Ctrl Pts',(3.4151183675076,1.,2.35898278606449));
#37352=CARTESIAN_POINT('Ctrl Pts',(3.41117262313464,-1.,2.35225606823649));
#37353=CARTESIAN_POINT('Ctrl Pts',(3.41117262313464,1.,2.35225606823649));
#37354=CARTESIAN_POINT('Ctrl Pts',(3.40720137403888,-1.,2.34555447648901));
#37355=CARTESIAN_POINT('Ctrl Pts',(3.40720137403888,1.,2.34555447648901));
#37356=CARTESIAN_POINT('Ctrl Pts',(3.40320452776646,-1.,2.33887832342715));
#37357=CARTESIAN_POINT('Ctrl Pts',(3.40320452776646,1.,2.33887832342715));
#37358=CARTESIAN_POINT('Ctrl Pts',(3.39918194578115,-1.,2.33222789882601));
#37359=CARTESIAN_POINT('Ctrl Pts',(3.39918194578115,1.,2.33222789882601));
#37360=CARTESIAN_POINT('Ctrl Pts',(3.39513342020045,-1.,2.32560343902683));
#37361=CARTESIAN_POINT('Ctrl Pts',(3.39513342020045,1.,2.32560343902683));
#37362=CARTESIAN_POINT('Ctrl Pts',(3.39105869475112,-1.,2.31900513925627));
#37363=CARTESIAN_POINT('Ctrl Pts',(3.39105869475112,1.,2.31900513925627));
#37364=CARTESIAN_POINT('Ctrl Pts',(3.38695751492659,-1.,2.31243319489505));
#37365=CARTESIAN_POINT('Ctrl Pts',(3.38695751492659,1.,2.31243319489505));
#37366=CARTESIAN_POINT('Ctrl Pts',(3.38282967336676,-1.,2.30588783640389));
#37367=CARTESIAN_POINT('Ctrl Pts',(3.38282967336676,1.,2.30588783640389));
#37368=CARTESIAN_POINT('Ctrl Pts',(3.37867504959382,-1.,2.29936936127588));
#37369=CARTESIAN_POINT('Ctrl Pts',(3.37867504959382,1.,2.29936936127588));
#37370=CARTESIAN_POINT('Ctrl Pts',(3.37449367172707,-1.,2.2928781800731));
#37371=CARTESIAN_POINT('Ctrl Pts',(3.37449367172707,1.,2.2928781800731));
#37372=CARTESIAN_POINT('Ctrl Pts',(3.37028570206357,-1.,2.28641481081045));
#37373=CARTESIAN_POINT('Ctrl Pts',(3.37028570206357,1.,2.28641481081045));
#37374=CARTESIAN_POINT('Ctrl Pts',(3.36605130712978,-1.,2.27997979457968));
#37375=CARTESIAN_POINT('Ctrl Pts',(3.36605130712978,1.,2.27997979457968));
#37376=CARTESIAN_POINT('Ctrl Pts',(3.36179055004369,-1.,2.27357362620902));
#37377=CARTESIAN_POINT('Ctrl Pts',(3.36179055004369,1.,2.27357362620902));
#37378=CARTESIAN_POINT('Ctrl Pts',(3.35750328523077,-1.,2.26719668579921));
#37379=CARTESIAN_POINT('Ctrl Pts',(3.35750328523077,1.,2.26719668579921));
#37380=CARTESIAN_POINT('Ctrl Pts',(3.35318902552676,-1.,2.26084915222484));
#37381=CARTESIAN_POINT('Ctrl Pts',(3.35318902552676,1.,2.26084915222484));
#37382=CARTESIAN_POINT('Ctrl Pts',(3.34884690292342,-1.,2.25453097693524));
#37383=CARTESIAN_POINT('Ctrl Pts',(3.34884690292342,1.,2.25453097693524));
#37384=CARTESIAN_POINT('Ctrl Pts',(3.34447596770768,-1.,2.24824207678288));
#37385=CARTESIAN_POINT('Ctrl Pts',(3.34447596770768,1.,2.24824207678288));
#37386=CARTESIAN_POINT('Ctrl Pts',(3.34007543738044,-1.,2.24198249391437));
#37387=CARTESIAN_POINT('Ctrl Pts',(3.34007543738044,1.,2.24198249391437));
#37388=CARTESIAN_POINT('Ctrl Pts',(3.33564495756478,-1.,2.2357525632881));
#37389=CARTESIAN_POINT('Ctrl Pts',(3.33564495756478,1.,2.2357525632881));
#37390=CARTESIAN_POINT('Ctrl Pts',(3.33118487773593,-1.,2.22955308907221));
#37391=CARTESIAN_POINT('Ctrl Pts',(3.33118487773593,1.,2.22955308907221));
#37392=CARTESIAN_POINT('Ctrl Pts',(3.32669646722871,-1.,2.22338548312759));
#37393=CARTESIAN_POINT('Ctrl Pts',(3.32669646722871,1.,2.22338548312759));
#37394=CARTESIAN_POINT('Ctrl Pts',(3.32218125618955,-1.,2.21725135110889));
#37395=CARTESIAN_POINT('Ctrl Pts',(3.32218125618955,1.,2.21725135110889));
#37396=CARTESIAN_POINT('Ctrl Pts',(3.31764044024231,-1.,2.21115211847872));
#37397=CARTESIAN_POINT('Ctrl Pts',(3.31764044024231,1.,2.21115211847872));
#37398=CARTESIAN_POINT('Ctrl Pts',(3.3130742460895,-1.,2.20508863150608));
#37399=CARTESIAN_POINT('Ctrl Pts',(3.3130742460895,1.,2.20508863150608));
#37400=CARTESIAN_POINT('Ctrl Pts',(3.30848134694596,-1.,2.19906078949925));
#37401=CARTESIAN_POINT('Ctrl Pts',(3.30848134694596,1.,2.19906078949925));
#37402=CARTESIAN_POINT('Ctrl Pts',(3.30385816281831,-1.,2.19306710376112));
#37403=CARTESIAN_POINT('Ctrl Pts',(3.30385816281831,1.,2.19306710376112));
#37404=CARTESIAN_POINT('Ctrl Pts',(3.29920022557635,-1.,2.18710556500325));
#37405=CARTESIAN_POINT('Ctrl Pts',(3.29920022557635,1.,2.18710556500325));
#37406=CARTESIAN_POINT('Ctrl Pts',(3.29450361500484,-1.,2.18117455557062));
#37407=CARTESIAN_POINT('Ctrl Pts',(3.29450361500484,1.,2.18117455557062));
#37408=CARTESIAN_POINT('Ctrl Pts',(3.28976645712566,-1.,2.17527380048422));
#37409=CARTESIAN_POINT('Ctrl Pts',(3.28976645712566,1.,2.17527380048422));
#37410=CARTESIAN_POINT('Ctrl Pts',(3.2849901997973,-1.,2.16940517773459));
#37411=CARTESIAN_POINT('Ctrl Pts',(3.2849901997973,1.,2.16940517773459));
#37412=CARTESIAN_POINT('Ctrl Pts',(3.28018150841414,-1.,2.16357391934434));
#37413=CARTESIAN_POINT('Ctrl Pts',(3.28018150841414,1.,2.16357391934434));
#37414=CARTESIAN_POINT('Ctrl Pts',(3.27534954469206,-1.,2.15778690038359));
#37415=CARTESIAN_POINT('Ctrl Pts',(3.27534954469206,1.,2.15778690038359));
#37416=CARTESIAN_POINT('Ctrl Pts',(3.27050245897244,-1.,2.15205043199818));
#37417=CARTESIAN_POINT('Ctrl Pts',(3.27050245897244,1.,2.15205043199818));
#37418=CARTESIAN_POINT('Ctrl Pts',(3.26564388189764,-1.,2.14636805295663));
#37419=CARTESIAN_POINT('Ctrl Pts',(3.26564388189764,1.,2.14636805295663));
#37420=CARTESIAN_POINT('Ctrl Pts',(3.26077002641868,-1.,2.14073870754258));
#37421=CARTESIAN_POINT('Ctrl Pts',(3.26077002641868,1.,2.14073870754258));
#37422=CARTESIAN_POINT('Ctrl Pts',(3.25586495065027,-1.,2.13515375878786));
#37423=CARTESIAN_POINT('Ctrl Pts',(3.25586495065027,1.,2.13515375878786));
#37424=CARTESIAN_POINT('Ctrl Pts',(3.25090574493994,-1.,2.1296002839681));
#37425=CARTESIAN_POINT('Ctrl Pts',(3.25090574493994,1.,2.1296002839681));
#37426=CARTESIAN_POINT('Ctrl Pts',(3.24587102613347,-1.,2.12406646410943));
#37427=CARTESIAN_POINT('Ctrl Pts',(3.24587102613347,1.,2.12406646410943));
#37428=CARTESIAN_POINT('Ctrl Pts',(3.24074905517282,-1.,2.11854673326972));
#37429=CARTESIAN_POINT('Ctrl Pts',(3.24074905517282,1.,2.11854673326972));
#37430=CARTESIAN_POINT('Ctrl Pts',(3.23554444767115,-1.,2.11304604021784));
#37431=CARTESIAN_POINT('Ctrl Pts',(3.23554444767115,1.,2.11304604021784));
#37432=CARTESIAN_POINT('Ctrl Pts',(3.23028945793334,-1.,2.1075869964248));
#37433=CARTESIAN_POINT('Ctrl Pts',(3.23028945793334,1.,2.1075869964248));
#37434=CARTESIAN_POINT('Ctrl Pts',(3.22503437553496,-1.,2.10220384298534));
#37435=CARTESIAN_POINT('Ctrl Pts',(3.22503437553496,1.,2.10220384298534));
#37436=CARTESIAN_POINT('Ctrl Pts',(3.21982707347067,-1.,2.09692958434933));
#37437=CARTESIAN_POINT('Ctrl Pts',(3.21982707347067,1.,2.09692958434933));
#37438=CARTESIAN_POINT('Ctrl Pts',(3.2146942960168,-1.,2.0917841946046));
#37439=CARTESIAN_POINT('Ctrl Pts',(3.2146942960168,1.,2.0917841946046));
#37440=CARTESIAN_POINT('Ctrl Pts',(3.20962575845433,-1.,2.08676465517435));
#37441=CARTESIAN_POINT('Ctrl Pts',(3.20962575845433,1.,2.08676465517435));
#37442=CARTESIAN_POINT('Ctrl Pts',(3.20454818630635,-1.,2.08182850370816));
#37443=CARTESIAN_POINT('Ctrl Pts',(3.20454818630635,1.,2.08182850370816));
#37444=CARTESIAN_POINT('Ctrl Pts',(3.19934132835879,-1.,2.0769044187063));
#37445=CARTESIAN_POINT('Ctrl Pts',(3.19934132835879,1.,2.0769044187063));
#37446=CARTESIAN_POINT('Ctrl Pts',(3.19388465568113,-1.,2.07192253497765));
#37447=CARTESIAN_POINT('Ctrl Pts',(3.19388465568113,1.,2.07192253497765));
#37448=CARTESIAN_POINT('Ctrl Pts',(3.18809755562297,-1.,2.06684062744065));
#37449=CARTESIAN_POINT('Ctrl Pts',(3.18809755562297,1.,2.06684062744065));
#37450=CARTESIAN_POINT('Ctrl Pts',(3.18197692964677,-1.,2.06166849827143));
#37451=CARTESIAN_POINT('Ctrl Pts',(3.18197692964677,1.,2.06166849827143));
#37452=CARTESIAN_POINT('Ctrl Pts',(3.17564906975592,-1.,2.05650186773279));
#37453=CARTESIAN_POINT('Ctrl Pts',(3.17564906975592,1.,2.05650186773279));
#37454=CARTESIAN_POINT('Ctrl Pts',(3.16936341689859,-1.,2.05151770247452));
#37455=CARTESIAN_POINT('Ctrl Pts',(3.16936341689859,1.,2.05151770247452));
#37456=CARTESIAN_POINT('Ctrl Pts',(3.16343165059235,-1.,2.0469333124766));
#37457=CARTESIAN_POINT('Ctrl Pts',(3.16343165059235,1.,2.0469333124766));
#37458=CARTESIAN_POINT('Ctrl Pts',(3.15817983946525,-1.,2.04297406404132));
#37459=CARTESIAN_POINT('Ctrl Pts',(3.15817983946525,1.,2.04297406404132));
#37460=CARTESIAN_POINT('Ctrl Pts',(3.1538999167466,-1.,2.03984073791432));
#37461=CARTESIAN_POINT('Ctrl Pts',(3.1538999167466,1.,2.03984073791432));
#37462=CARTESIAN_POINT('Ctrl Pts',(3.15079010635326,-1.,2.03766932526171));
#37463=CARTESIAN_POINT('Ctrl Pts',(3.15079010635326,1.,2.03766932526171));
#37464=CARTESIAN_POINT('Ctrl Pts',(3.14931281967585,-1.,2.03675273048882));
#37465=CARTESIAN_POINT('Ctrl Pts',(3.14931281967585,1.,2.03675273048882));
#37466=CARTESIAN_POINT('Ctrl Pts',(3.14878756590499,-1.,2.03653654935384));
#37467=CARTESIAN_POINT('Ctrl Pts',(3.14878756590499,1.,2.03653654935384));
#37468=CARTESIAN_POINT('Ctrl Pts',(3.14869618937138,-1.,2.036601737578));
#37469=CARTESIAN_POINT('Ctrl Pts',(3.14869618937138,1.,2.036601737578));
#37470=CARTESIAN_POINT('Ctrl Pts',(3.1487152044751,-1.,2.03668666247593));
#37471=CARTESIAN_POINT('Ctrl Pts',(3.1487152044751,1.,2.03668666247593));
#37472=CARTESIAN_POINT('',(3.44202241512147,1.,2.40675750623143));
#37473=CARTESIAN_POINT('Ctrl Pts',(3.44202241512147,1.,2.40675750623143));
#37474=CARTESIAN_POINT('Ctrl Pts',(3.44127120683402,1.,2.40537592959345));
#37475=CARTESIAN_POINT('Ctrl Pts',(3.43976627485223,1.,2.40261515590099));
#37476=CARTESIAN_POINT('Ctrl Pts',(3.43750133066036,1.,2.39848113411429));
#37477=CARTESIAN_POINT('Ctrl Pts',(3.43446630680436,1.,2.39298338805823));
#37478=CARTESIAN_POINT('Ctrl Pts',(3.43064732714472,1.,2.38613505844641));
#37479=CARTESIAN_POINT('Ctrl Pts',(3.42680309755241,1.,2.37931067029517));
#37480=CARTESIAN_POINT('Ctrl Pts',(3.42293356216595,1.,2.37251035954351));
#37481=CARTESIAN_POINT('Ctrl Pts',(3.41903866635384,1.,2.36573431470314));
#37482=CARTESIAN_POINT('Ctrl Pts',(3.4151183675076,1.,2.35898278606449));
#37483=CARTESIAN_POINT('Ctrl Pts',(3.41117262313464,1.,2.35225606823649));
#37484=CARTESIAN_POINT('Ctrl Pts',(3.40720137403888,1.,2.34555447648901));
#37485=CARTESIAN_POINT('Ctrl Pts',(3.40320452776646,1.,2.33887832342715));
#37486=CARTESIAN_POINT('Ctrl Pts',(3.39918194578115,1.,2.33222789882601));
#37487=CARTESIAN_POINT('Ctrl Pts',(3.39513342020045,1.,2.32560343902683));
#37488=CARTESIAN_POINT('Ctrl Pts',(3.39105869475112,1.,2.31900513925627));
#37489=CARTESIAN_POINT('Ctrl Pts',(3.38695751492659,1.,2.31243319489505));
#37490=CARTESIAN_POINT('Ctrl Pts',(3.38282967336676,1.,2.30588783640389));
#37491=CARTESIAN_POINT('Ctrl Pts',(3.37867504959382,1.,2.29936936127588));
#37492=CARTESIAN_POINT('Ctrl Pts',(3.37449367172707,1.,2.2928781800731));
#37493=CARTESIAN_POINT('Ctrl Pts',(3.37028570206357,1.,2.28641481081045));
#37494=CARTESIAN_POINT('Ctrl Pts',(3.36605130712978,1.,2.27997979457968));
#37495=CARTESIAN_POINT('Ctrl Pts',(3.36179055004369,1.,2.27357362620902));
#37496=CARTESIAN_POINT('Ctrl Pts',(3.35750328523077,1.,2.26719668579921));
#37497=CARTESIAN_POINT('Ctrl Pts',(3.35318902552676,1.,2.26084915222484));
#37498=CARTESIAN_POINT('Ctrl Pts',(3.34884690292342,1.,2.25453097693524));
#37499=CARTESIAN_POINT('Ctrl Pts',(3.34447596770768,1.,2.24824207678288));
#37500=CARTESIAN_POINT('Ctrl Pts',(3.34007543738044,1.,2.24198249391437));
#37501=CARTESIAN_POINT('Ctrl Pts',(3.33564495756478,1.,2.2357525632881));
#37502=CARTESIAN_POINT('Ctrl Pts',(3.33118487773593,1.,2.22955308907221));
#37503=CARTESIAN_POINT('Ctrl Pts',(3.32669646722871,1.,2.22338548312759));
#37504=CARTESIAN_POINT('Ctrl Pts',(3.32218125618955,1.,2.21725135110889));
#37505=CARTESIAN_POINT('Ctrl Pts',(3.31764044024231,1.,2.21115211847872));
#37506=CARTESIAN_POINT('Ctrl Pts',(3.3130742460895,1.,2.20508863150608));
#37507=CARTESIAN_POINT('Ctrl Pts',(3.30848134694596,1.,2.19906078949925));
#37508=CARTESIAN_POINT('Ctrl Pts',(3.30385816281831,1.,2.19306710376112));
#37509=CARTESIAN_POINT('Ctrl Pts',(3.29920022557635,1.,2.18710556500325));
#37510=CARTESIAN_POINT('Ctrl Pts',(3.29450361500484,1.,2.18117455557062));
#37511=CARTESIAN_POINT('Ctrl Pts',(3.28976645712566,1.,2.17527380048422));
#37512=CARTESIAN_POINT('Ctrl Pts',(3.2849901997973,1.,2.16940517773459));
#37513=CARTESIAN_POINT('Ctrl Pts',(3.28018150841414,1.,2.16357391934434));
#37514=CARTESIAN_POINT('Ctrl Pts',(3.27534954469206,1.,2.15778690038359));
#37515=CARTESIAN_POINT('Ctrl Pts',(3.27050245897244,1.,2.15205043199818));
#37516=CARTESIAN_POINT('Ctrl Pts',(3.26564388189764,1.,2.14636805295663));
#37517=CARTESIAN_POINT('Ctrl Pts',(3.26077002641868,1.,2.14073870754258));
#37518=CARTESIAN_POINT('Ctrl Pts',(3.25586495065027,1.,2.13515375878786));
#37519=CARTESIAN_POINT('Ctrl Pts',(3.25090574493994,1.,2.1296002839681));
#37520=CARTESIAN_POINT('Ctrl Pts',(3.24587102613347,1.,2.12406646410943));
#37521=CARTESIAN_POINT('Ctrl Pts',(3.24074905517282,1.,2.11854673326972));
#37522=CARTESIAN_POINT('Ctrl Pts',(3.23554444767115,1.,2.11304604021784));
#37523=CARTESIAN_POINT('Ctrl Pts',(3.23028945793334,1.,2.1075869964248));
#37524=CARTESIAN_POINT('Ctrl Pts',(3.22503437553496,1.,2.10220384298534));
#37525=CARTESIAN_POINT('Ctrl Pts',(3.21982707347067,1.,2.09692958434933));
#37526=CARTESIAN_POINT('Ctrl Pts',(3.2146942960168,1.,2.0917841946046));
#37527=CARTESIAN_POINT('Ctrl Pts',(3.20962575845433,1.,2.08676465517435));
#37528=CARTESIAN_POINT('Ctrl Pts',(3.20454818630635,1.,2.08182850370816));
#37529=CARTESIAN_POINT('Ctrl Pts',(3.19934132835879,1.,2.0769044187063));
#37530=CARTESIAN_POINT('Ctrl Pts',(3.19388465568113,1.,2.07192253497765));
#37531=CARTESIAN_POINT('Ctrl Pts',(3.18809755562297,1.,2.06684062744065));
#37532=CARTESIAN_POINT('Ctrl Pts',(3.18197692964677,1.,2.06166849827143));
#37533=CARTESIAN_POINT('Ctrl Pts',(3.17564906975592,1.,2.05650186773279));
#37534=CARTESIAN_POINT('Ctrl Pts',(3.16936341689859,1.,2.05151770247452));
#37535=CARTESIAN_POINT('Ctrl Pts',(3.16343165059235,1.,2.0469333124766));
#37536=CARTESIAN_POINT('Ctrl Pts',(3.15817983946525,1.,2.04297406404132));
#37537=CARTESIAN_POINT('Ctrl Pts',(3.1538999167466,1.,2.03984073791432));
#37538=CARTESIAN_POINT('Ctrl Pts',(3.15102344775396,1.,2.03783225496023));
#37539=CARTESIAN_POINT('Ctrl Pts',(3.14959882629936,1.,2.03693188810614));
#37540=CARTESIAN_POINT('Ctrl Pts',(3.14901193669147,1.,2.03663974554941));
#37541=CARTESIAN_POINT('Ctrl Pts',(3.1488193908823,1.,2.03659701539175));
#37542=CARTESIAN_POINT('Ctrl Pts',(3.14877060440425,1.,2.03660101169564));
#37543=CARTESIAN_POINT('',(3.44202241512147,0.,2.40675750623143));
#37544=CARTESIAN_POINT('Ctrl Pts',(2.91001063062876,-1.,2.36523532225181));
#37545=CARTESIAN_POINT('Ctrl Pts',(2.91001063062876,1.,2.36523532225181));
#37546=CARTESIAN_POINT('Ctrl Pts',(2.90992398626211,-1.,2.36524348105112));
#37547=CARTESIAN_POINT('Ctrl Pts',(2.90992398626211,1.,2.36524348105112));
#37548=CARTESIAN_POINT('Ctrl Pts',(2.90989022548032,-1.,2.36535052956938));
#37549=CARTESIAN_POINT('Ctrl Pts',(2.90989022548032,1.,2.36535052956938));
#37550=CARTESIAN_POINT('Ctrl Pts',(2.91025813830041,-1.,2.36578327194741));
#37551=CARTESIAN_POINT('Ctrl Pts',(2.91025813830041,1.,2.36578327194741));
#37552=CARTESIAN_POINT('Ctrl Pts',(2.9115863784204,-1.,2.36690501170627));
#37553=CARTESIAN_POINT('Ctrl Pts',(2.9115863784204,1.,2.36690501170627));
#37554=CARTESIAN_POINT('Ctrl Pts',(2.9146124988314,-1.,2.36919161373173));
#37555=CARTESIAN_POINT('Ctrl Pts',(2.9146124988314,1.,2.36919161373173));
#37556=CARTESIAN_POINT('Ctrl Pts',(2.91891503791411,-1.,2.37229381109821));
#37557=CARTESIAN_POINT('Ctrl Pts',(2.91891503791411,1.,2.37229381109821));
#37558=CARTESIAN_POINT('Ctrl Pts',(2.92430340582608,-1.,2.3760651052403));
#37559=CARTESIAN_POINT('Ctrl Pts',(2.92430340582608,1.,2.3760651052403));
#37560=CARTESIAN_POINT('Ctrl Pts',(2.93049643640206,-1.,2.38028989582073));
#37561=CARTESIAN_POINT('Ctrl Pts',(2.93049643640206,1.,2.38028989582073));
#37562=CARTESIAN_POINT('Ctrl Pts',(2.93717903280391,-1.,2.38472771516311));
#37563=CARTESIAN_POINT('Ctrl Pts',(2.93717903280391,1.,2.38472771516311));
#37564=CARTESIAN_POINT('Ctrl Pts',(2.94404820669076,-1.,2.38914929090759));
#37565=CARTESIAN_POINT('Ctrl Pts',(2.94404820669076,1.,2.38914929090759));
#37566=CARTESIAN_POINT('Ctrl Pts',(2.95085857128439,-1.,2.39337207631667));
#37567=CARTESIAN_POINT('Ctrl Pts',(2.95085857128439,1.,2.39337207631667));
#37568=CARTESIAN_POINT('Ctrl Pts',(2.95748006482942,-1.,2.39730553974517));
#37569=CARTESIAN_POINT('Ctrl Pts',(2.95748006482942,1.,2.39730553974517));
#37570=CARTESIAN_POINT('Ctrl Pts',(2.96390432240312,-1.,2.4009556571164));
#37571=CARTESIAN_POINT('Ctrl Pts',(2.96390432240312,1.,2.4009556571164));
#37572=CARTESIAN_POINT('Ctrl Pts',(2.9701964131236,-1.,2.40438604734919));
#37573=CARTESIAN_POINT('Ctrl Pts',(2.9701964131236,1.,2.40438604734919));
#37574=CARTESIAN_POINT('Ctrl Pts',(2.97646002822422,-1.,2.40768975073713));
#37575=CARTESIAN_POINT('Ctrl Pts',(2.97646002822422,1.,2.40768975073713));
#37576=CARTESIAN_POINT('Ctrl Pts',(2.98280015815107,-1.,2.41095909342571));
#37577=CARTESIAN_POINT('Ctrl Pts',(2.98280015815107,1.,2.41095909342571));
#37578=CARTESIAN_POINT('Ctrl Pts',(2.98927983005796,-1.,2.41425064199586));
#37579=CARTESIAN_POINT('Ctrl Pts',(2.98927983005796,1.,2.41425064199586));
#37580=CARTESIAN_POINT('Ctrl Pts',(2.99590509293503,-1.,2.41757324500514));
#37581=CARTESIAN_POINT('Ctrl Pts',(2.99590509293503,1.,2.41757324500514));
#37582=CARTESIAN_POINT('Ctrl Pts',(3.00264868585996,-1.,2.42090763946779));
#37583=CARTESIAN_POINT('Ctrl Pts',(3.00264868585996,1.,2.42090763946779));
#37584=CARTESIAN_POINT('Ctrl Pts',(3.00946442616658,-1.,2.42421849439613));
#37585=CARTESIAN_POINT('Ctrl Pts',(3.00946442616658,1.,2.42421849439613));
#37586=CARTESIAN_POINT('Ctrl Pts',(3.01630420830504,-1.,2.42746856264168));
#37587=CARTESIAN_POINT('Ctrl Pts',(3.01630420830504,1.,2.42746856264168));
#37588=CARTESIAN_POINT('Ctrl Pts',(3.02313656036004,-1.,2.43063415586637));
#37589=CARTESIAN_POINT('Ctrl Pts',(3.02313656036004,1.,2.43063415586637));
#37590=CARTESIAN_POINT('Ctrl Pts',(3.02995534946978,-1.,2.43371241361488));
#37591=CARTESIAN_POINT('Ctrl Pts',(3.02995534946978,1.,2.43371241361488));
#37592=CARTESIAN_POINT('Ctrl Pts',(3.03676949672821,-1.,2.43671278042414));
#37593=CARTESIAN_POINT('Ctrl Pts',(3.03676949672821,1.,2.43671278042414));
#37594=CARTESIAN_POINT('Ctrl Pts',(3.04359685040555,-1.,2.43965194061857));
#37595=CARTESIAN_POINT('Ctrl Pts',(3.04359685040555,1.,2.43965194061857));
#37596=CARTESIAN_POINT('Ctrl Pts',(3.05045678021504,-1.,2.44254768923105));
#37597=CARTESIAN_POINT('Ctrl Pts',(3.05045678021504,1.,2.44254768923105));
#37598=CARTESIAN_POINT('Ctrl Pts',(3.05736242671506,-1.,2.44541251892556));
#37599=CARTESIAN_POINT('Ctrl Pts',(3.05736242671506,1.,2.44541251892556));
#37600=CARTESIAN_POINT('Ctrl Pts',(3.06431596421405,-1.,2.44824970516544));
#37601=CARTESIAN_POINT('Ctrl Pts',(3.06431596421405,1.,2.44824970516544));
#37602=CARTESIAN_POINT('Ctrl Pts',(3.07131290521297,-1.,2.45105688854422));
#37603=CARTESIAN_POINT('Ctrl Pts',(3.07131290521297,1.,2.45105688854422));
#37604=CARTESIAN_POINT('Ctrl Pts',(3.07834472886139,-1.,2.4538282678779));
#37605=CARTESIAN_POINT('Ctrl Pts',(3.07834472886139,1.,2.4538282678779));
#37606=CARTESIAN_POINT('Ctrl Pts',(3.08540206545315,-1.,2.45655725437039));
#37607=CARTESIAN_POINT('Ctrl Pts',(3.08540206545315,1.,2.45655725437039));
#37608=CARTESIAN_POINT('Ctrl Pts',(3.09247787931887,-1.,2.4592391256388));
#37609=CARTESIAN_POINT('Ctrl Pts',(3.09247787931887,1.,2.4592391256388));
#37610=CARTESIAN_POINT('Ctrl Pts',(3.09956993697052,-1.,2.46187308501884));
#37611=CARTESIAN_POINT('Ctrl Pts',(3.09956993697052,1.,2.46187308501884));
#37612=CARTESIAN_POINT('Ctrl Pts',(3.1066790790198,-1.,2.46446082979646));
#37613=CARTESIAN_POINT('Ctrl Pts',(3.1066790790198,1.,2.46446082979646));
#37614=CARTESIAN_POINT('Ctrl Pts',(3.11380805536122,-1.,2.46700558843506));
#37615=CARTESIAN_POINT('Ctrl Pts',(3.11380805536122,1.,2.46700558843506));
#37616=CARTESIAN_POINT('Ctrl Pts',(3.12096015766983,-1.,2.46951098947469));
#37617=CARTESIAN_POINT('Ctrl Pts',(3.12096015766983,1.,2.46951098947469));
#37618=CARTESIAN_POINT('Ctrl Pts',(3.12813790805952,-1.,2.47197997765871));
#37619=CARTESIAN_POINT('Ctrl Pts',(3.12813790805952,1.,2.47197997765871));
#37620=CARTESIAN_POINT('Ctrl Pts',(3.13534181229295,-1.,2.47441378371932));
#37621=CARTESIAN_POINT('Ctrl Pts',(3.13534181229295,1.,2.47441378371932));
#37622=CARTESIAN_POINT('Ctrl Pts',(3.1425709954655,-1.,2.47681245356109));
#37623=CARTESIAN_POINT('Ctrl Pts',(3.1425709954655,1.,2.47681245356109));
#37624=CARTESIAN_POINT('Ctrl Pts',(3.14982373241352,-1.,2.47917529057029));
#37625=CARTESIAN_POINT('Ctrl Pts',(3.14982373241352,1.,2.47917529057029));
#37626=CARTESIAN_POINT('Ctrl Pts',(3.15709802322739,-1.,2.48150133566571));
#37627=CARTESIAN_POINT('Ctrl Pts',(3.15709802322739,1.,2.48150133566571));
#37628=CARTESIAN_POINT('Ctrl Pts',(3.16439213290161,-1.,2.48378981792725));
#37629=CARTESIAN_POINT('Ctrl Pts',(3.16439213290161,1.,2.48378981792725));
#37630=CARTESIAN_POINT('Ctrl Pts',(3.17170518863313,-1.,2.48604065348587));
#37631=CARTESIAN_POINT('Ctrl Pts',(3.17170518863313,1.,2.48604065348587));
#37632=CARTESIAN_POINT('Ctrl Pts',(3.17903698136622,-1.,2.48825428288201));
#37633=CARTESIAN_POINT('Ctrl Pts',(3.17903698136622,1.,2.48825428288201));
#37634=CARTESIAN_POINT('Ctrl Pts',(3.18638771282266,-1.,2.49043146334059));
#37635=CARTESIAN_POINT('Ctrl Pts',(3.18638771282266,1.,2.49043146334059));
#37636=CARTESIAN_POINT('Ctrl Pts',(3.19375775555798,-1.,2.49257307239848));
#37637=CARTESIAN_POINT('Ctrl Pts',(3.19375775555798,1.,2.49257307239848));
#37638=CARTESIAN_POINT('Ctrl Pts',(3.20114742397588,-1.,2.49467992057755));
#37639=CARTESIAN_POINT('Ctrl Pts',(3.20114742397588,1.,2.49467992057755));
#37640=CARTESIAN_POINT('Ctrl Pts',(3.20855669849836,-1.,2.4967525264737));
#37641=CARTESIAN_POINT('Ctrl Pts',(3.20855669849836,1.,2.4967525264737));
#37642=CARTESIAN_POINT('Ctrl Pts',(3.21598526261286,-1.,2.4987911459939));
#37643=CARTESIAN_POINT('Ctrl Pts',(3.21598526261286,1.,2.4987911459939));
#37644=CARTESIAN_POINT('Ctrl Pts',(3.22343262620503,-1.,2.50079587201958));
#37645=CARTESIAN_POINT('Ctrl Pts',(3.22343262620503,1.,2.50079587201958));
#37646=CARTESIAN_POINT('Ctrl Pts',(3.23089822320646,-1.,2.50276671338111));
#37647=CARTESIAN_POINT('Ctrl Pts',(3.23089822320646,1.,2.50276671338111));
#37648=CARTESIAN_POINT('Ctrl Pts',(3.23838151080319,-1.,2.5047036758003));
#37649=CARTESIAN_POINT('Ctrl Pts',(3.23838151080319,1.,2.5047036758003));
#37650=CARTESIAN_POINT('Ctrl Pts',(3.24588208983849,-1.,2.506606859405));
#37651=CARTESIAN_POINT('Ctrl Pts',(3.24588208983849,1.,2.506606859405));
#37652=CARTESIAN_POINT('Ctrl Pts',(3.25339971460982,-1.,2.50847647070723));
#37653=CARTESIAN_POINT('Ctrl Pts',(3.25339971460982,1.,2.50847647070723));
#37654=CARTESIAN_POINT('Ctrl Pts',(3.26093423001434,-1.,2.51031277813486));
#37655=CARTESIAN_POINT('Ctrl Pts',(3.26093423001434,1.,2.51031277813486));
#37656=CARTESIAN_POINT('Ctrl Pts',(3.26848552888115,-1.,2.51211608411423));
#37657=CARTESIAN_POINT('Ctrl Pts',(3.26848552888115,1.,2.51211608411423));
#37658=CARTESIAN_POINT('Ctrl Pts',(3.27605350473142,-1.,2.513886692704));
#37659=CARTESIAN_POINT('Ctrl Pts',(3.27605350473142,1.,2.513886692704));
#37660=CARTESIAN_POINT('Ctrl Pts',(3.28363799702982,-1.,2.51562487464514));
#37661=CARTESIAN_POINT('Ctrl Pts',(3.28363799702982,1.,2.51562487464514));
#37662=CARTESIAN_POINT('Ctrl Pts',(3.2912387729927,-1.,2.51733085123797));
#37663=CARTESIAN_POINT('Ctrl Pts',(3.2912387729927,1.,2.51733085123797));
#37664=CARTESIAN_POINT('Ctrl Pts',(3.29885556388352,-1.,2.51900480701069));
#37665=CARTESIAN_POINT('Ctrl Pts',(3.29885556388352,1.,2.51900480701069));
#37666=CARTESIAN_POINT('Ctrl Pts',(3.30648808815442,-1.,2.52064689568511));
#37667=CARTESIAN_POINT('Ctrl Pts',(3.30648808815442,1.,2.52064689568511));
#37668=CARTESIAN_POINT('Ctrl Pts',(3.31413607874645,-1.,2.52225724871313));
#37669=CARTESIAN_POINT('Ctrl Pts',(3.31413607874645,1.,2.52225724871313));
#37670=CARTESIAN_POINT('Ctrl Pts',(3.32179931078699,-1.,2.5238359839626));
#37671=CARTESIAN_POINT('Ctrl Pts',(3.32179931078699,1.,2.5238359839626));
#37672=CARTESIAN_POINT('Ctrl Pts',(3.32947762187533,-1.,2.52538321164634));
#37673=CARTESIAN_POINT('Ctrl Pts',(3.32947762187533,1.,2.52538321164634));
#37674=CARTESIAN_POINT('Ctrl Pts',(3.33717089999103,-1.,2.52689902690158));
#37675=CARTESIAN_POINT('Ctrl Pts',(3.33717089999103,1.,2.52689902690158));
#37676=CARTESIAN_POINT('Ctrl Pts',(3.34333744115511,-1.,2.52808660915689));
#37677=CARTESIAN_POINT('Ctrl Pts',(3.34333744115511,1.,2.52808660915689));
#37678=CARTESIAN_POINT('Ctrl Pts',(3.34796903576663,-1.,2.52896321610703));
#37679=CARTESIAN_POINT('Ctrl Pts',(3.34796903576663,1.,2.52896321610703));
#37680=CARTESIAN_POINT('Ctrl Pts',(3.35105973714071,-1.,2.5295413654909));
#37681=CARTESIAN_POINT('Ctrl Pts',(3.35105973714071,1.,2.5295413654909));
#37682=CARTESIAN_POINT('Ctrl Pts',(3.35260583073571,-1.,2.52982887637028));
#37683=CARTESIAN_POINT('Ctrl Pts',(3.35260583073571,1.,2.52982887637028));
#37684=CARTESIAN_POINT('',(2.90994629141676,1.,2.36531447826073));
#37685=CARTESIAN_POINT('Ctrl Pts',(2.90994629141676,-1.,2.36531447826073));
#37686=CARTESIAN_POINT('Ctrl Pts',(2.90994629141676,-0.666666666666667,
2.36531447826073));
#37687=CARTESIAN_POINT('Ctrl Pts',(2.90994629141676,-0.333333333333333,
2.36531447826073));
#37688=CARTESIAN_POINT('Ctrl Pts',(2.90994629141676,0.333333333333333,2.36531447826073));
#37689=CARTESIAN_POINT('Ctrl Pts',(2.90994629141676,0.666666666666667,2.36531447826073));
#37690=CARTESIAN_POINT('Ctrl Pts',(2.90994629141676,1.,2.36531447826073));
#37691=CARTESIAN_POINT('',(3.35260583073571,1.,2.52982887637028));
#37692=CARTESIAN_POINT('',(3.35260583073571,0.,2.52982887637028));
#37693=CARTESIAN_POINT('Ctrl Pts',(2.90994629141676,1.,2.36531447826073));
#37694=CARTESIAN_POINT('Ctrl Pts',(2.90995756655606,1.,2.36536211188453));
#37695=CARTESIAN_POINT('Ctrl Pts',(2.91005770527719,1.,2.36553202948613));
#37696=CARTESIAN_POINT('Ctrl Pts',(2.91051690822156,1.,2.36599991765749));
#37697=CARTESIAN_POINT('Ctrl Pts',(2.91181344022548,1.,2.36707658451664));
#37698=CARTESIAN_POINT('Ctrl Pts',(2.9146124988314,1.,2.36919161373173));
#37699=CARTESIAN_POINT('Ctrl Pts',(2.91891503791411,1.,2.37229381109821));
#37700=CARTESIAN_POINT('Ctrl Pts',(2.92430340582608,1.,2.3760651052403));
#37701=CARTESIAN_POINT('Ctrl Pts',(2.93049643640206,1.,2.38028989582073));
#37702=CARTESIAN_POINT('Ctrl Pts',(2.93717903280391,1.,2.38472771516311));
#37703=CARTESIAN_POINT('Ctrl Pts',(2.94404820669076,1.,2.38914929090759));
#37704=CARTESIAN_POINT('Ctrl Pts',(2.95085857128439,1.,2.39337207631667));
#37705=CARTESIAN_POINT('Ctrl Pts',(2.95748006482942,1.,2.39730553974517));
#37706=CARTESIAN_POINT('Ctrl Pts',(2.96390432240312,1.,2.4009556571164));
#37707=CARTESIAN_POINT('Ctrl Pts',(2.9701964131236,1.,2.40438604734919));
#37708=CARTESIAN_POINT('Ctrl Pts',(2.97646002822422,1.,2.40768975073713));
#37709=CARTESIAN_POINT('Ctrl Pts',(2.98280015815107,1.,2.41095909342571));
#37710=CARTESIAN_POINT('Ctrl Pts',(2.98927983005796,1.,2.41425064199586));
#37711=CARTESIAN_POINT('Ctrl Pts',(2.99590509293503,1.,2.41757324500514));
#37712=CARTESIAN_POINT('Ctrl Pts',(3.00264868585996,1.,2.42090763946779));
#37713=CARTESIAN_POINT('Ctrl Pts',(3.00946442616658,1.,2.42421849439613));
#37714=CARTESIAN_POINT('Ctrl Pts',(3.01630420830504,1.,2.42746856264168));
#37715=CARTESIAN_POINT('Ctrl Pts',(3.02313656036004,1.,2.43063415586637));
#37716=CARTESIAN_POINT('Ctrl Pts',(3.02995534946978,1.,2.43371241361488));
#37717=CARTESIAN_POINT('Ctrl Pts',(3.03676949672821,1.,2.43671278042414));
#37718=CARTESIAN_POINT('Ctrl Pts',(3.04359685040555,1.,2.43965194061857));
#37719=CARTESIAN_POINT('Ctrl Pts',(3.05045678021504,1.,2.44254768923105));
#37720=CARTESIAN_POINT('Ctrl Pts',(3.05736242671506,1.,2.44541251892556));
#37721=CARTESIAN_POINT('Ctrl Pts',(3.06431596421405,1.,2.44824970516544));
#37722=CARTESIAN_POINT('Ctrl Pts',(3.07131290521297,1.,2.45105688854422));
#37723=CARTESIAN_POINT('Ctrl Pts',(3.07834472886139,1.,2.4538282678779));
#37724=CARTESIAN_POINT('Ctrl Pts',(3.08540206545315,1.,2.45655725437039));
#37725=CARTESIAN_POINT('Ctrl Pts',(3.09247787931887,1.,2.4592391256388));
#37726=CARTESIAN_POINT('Ctrl Pts',(3.09956993697052,1.,2.46187308501884));
#37727=CARTESIAN_POINT('Ctrl Pts',(3.1066790790198,1.,2.46446082979646));
#37728=CARTESIAN_POINT('Ctrl Pts',(3.11380805536122,1.,2.46700558843506));
#37729=CARTESIAN_POINT('Ctrl Pts',(3.12096015766983,1.,2.46951098947469));
#37730=CARTESIAN_POINT('Ctrl Pts',(3.12813790805952,1.,2.47197997765871));
#37731=CARTESIAN_POINT('Ctrl Pts',(3.13534181229295,1.,2.47441378371932));
#37732=CARTESIAN_POINT('Ctrl Pts',(3.1425709954655,1.,2.47681245356109));
#37733=CARTESIAN_POINT('Ctrl Pts',(3.14982373241352,1.,2.47917529057029));
#37734=CARTESIAN_POINT('Ctrl Pts',(3.15709802322739,1.,2.48150133566571));
#37735=CARTESIAN_POINT('Ctrl Pts',(3.16439213290161,1.,2.48378981792725));
#37736=CARTESIAN_POINT('Ctrl Pts',(3.17170518863313,1.,2.48604065348587));
#37737=CARTESIAN_POINT('Ctrl Pts',(3.17903698136622,1.,2.48825428288201));
#37738=CARTESIAN_POINT('Ctrl Pts',(3.18638771282266,1.,2.49043146334059));
#37739=CARTESIAN_POINT('Ctrl Pts',(3.19375775555798,1.,2.49257307239848));
#37740=CARTESIAN_POINT('Ctrl Pts',(3.20114742397588,1.,2.49467992057755));
#37741=CARTESIAN_POINT('Ctrl Pts',(3.20855669849836,1.,2.4967525264737));
#37742=CARTESIAN_POINT('Ctrl Pts',(3.21598526261286,1.,2.4987911459939));
#37743=CARTESIAN_POINT('Ctrl Pts',(3.22343262620503,1.,2.50079587201958));
#37744=CARTESIAN_POINT('Ctrl Pts',(3.23089822320646,1.,2.50276671338111));
#37745=CARTESIAN_POINT('Ctrl Pts',(3.23838151080319,1.,2.5047036758003));
#37746=CARTESIAN_POINT('Ctrl Pts',(3.24588208983849,1.,2.506606859405));
#37747=CARTESIAN_POINT('Ctrl Pts',(3.25339971460982,1.,2.50847647070723));
#37748=CARTESIAN_POINT('Ctrl Pts',(3.26093423001434,1.,2.51031277813486));
#37749=CARTESIAN_POINT('Ctrl Pts',(3.26848552888115,1.,2.51211608411423));
#37750=CARTESIAN_POINT('Ctrl Pts',(3.27605350473142,1.,2.513886692704));
#37751=CARTESIAN_POINT('Ctrl Pts',(3.28363799702982,1.,2.51562487464514));
#37752=CARTESIAN_POINT('Ctrl Pts',(3.2912387729927,1.,2.51733085123797));
#37753=CARTESIAN_POINT('Ctrl Pts',(3.29885556388352,1.,2.51900480701069));
#37754=CARTESIAN_POINT('Ctrl Pts',(3.30648808815442,1.,2.52064689568511));
#37755=CARTESIAN_POINT('Ctrl Pts',(3.31413607874645,1.,2.52225724871313));
#37756=CARTESIAN_POINT('Ctrl Pts',(3.32179931078699,1.,2.5238359839626));
#37757=CARTESIAN_POINT('Ctrl Pts',(3.32947762187533,1.,2.52538321164634));
#37758=CARTESIAN_POINT('Ctrl Pts',(3.33717089999103,1.,2.52689902690158));
#37759=CARTESIAN_POINT('Ctrl Pts',(3.34333744115511,1.,2.52808660915689));
#37760=CARTESIAN_POINT('Ctrl Pts',(3.34796903576663,1.,2.52896321610703));
#37761=CARTESIAN_POINT('Ctrl Pts',(3.35105973714071,1.,2.5295413654909));
#37762=CARTESIAN_POINT('Ctrl Pts',(3.35260583073571,1.,2.52982887637028));
#37763=CARTESIAN_POINT('Origin',(3.35260583073571,0.,2.52982887637028));
#37764=CARTESIAN_POINT('',(3.44202241512147,1.,2.40675750623143));
#37765=CARTESIAN_POINT('Origin',(0.,0.,0.));
#37766=CARTESIAN_POINT('',(2.79140942341378,1.,2.50410331873042));
#37767=CARTESIAN_POINT('Origin',(0.,1.,0.));
#37768=CARTESIAN_POINT('Ctrl Pts',(2.79140942341378,1.,2.50410331873043));
#37769=CARTESIAN_POINT('Ctrl Pts',(2.79140942341378,0.666666666666667,2.50410331873043));
#37770=CARTESIAN_POINT('Ctrl Pts',(2.79140942341378,0.333333333333333,2.50410331873042));
#37771=CARTESIAN_POINT('Ctrl Pts',(2.79140942341378,-0.333333333333333,
2.50410331873042));
#37772=CARTESIAN_POINT('Ctrl Pts',(2.79140942341378,-0.666666666666667,
2.50410331873042));
#37773=CARTESIAN_POINT('Ctrl Pts',(2.79140942341378,-1.,2.50410331873042));
#37774=CARTESIAN_POINT('Ctrl Pts',(3.02314558451372,-1.,2.91557726271063));
#37775=CARTESIAN_POINT('Ctrl Pts',(3.02314558451372,1.,2.91557726271063));
#37776=CARTESIAN_POINT('Ctrl Pts',(3.02261975104912,-1.,2.91409518070707));
#37777=CARTESIAN_POINT('Ctrl Pts',(3.02261975104912,1.,2.91409518070707));
#37778=CARTESIAN_POINT('Ctrl Pts',(3.02156522743299,-1.,2.91113297349052));
#37779=CARTESIAN_POINT('Ctrl Pts',(3.02156522743299,1.,2.91113297349052));
#37780=CARTESIAN_POINT('Ctrl Pts',(3.01997487194926,-1.,2.90669553303902));
#37781=CARTESIAN_POINT('Ctrl Pts',(3.01997487194926,1.,2.90669553303902));
#37782=CARTESIAN_POINT('Ctrl Pts',(3.01783725123646,-1.,2.90079069102661));
#37783=CARTESIAN_POINT('Ctrl Pts',(3.01783725123646,1.,2.90079069102661));
#37784=CARTESIAN_POINT('Ctrl Pts',(3.01513660433291,-1.,2.8934292556764));
#37785=CARTESIAN_POINT('Ctrl Pts',(3.01513660433291,1.,2.8934292556764));
#37786=CARTESIAN_POINT('Ctrl Pts',(3.01240727309568,-1.,2.88608751706796));
#37787=CARTESIAN_POINT('Ctrl Pts',(3.01240727309568,1.,2.88608751706796));
#37788=CARTESIAN_POINT('Ctrl Pts',(3.0096491810855,-1.,2.87876560072799));
#37789=CARTESIAN_POINT('Ctrl Pts',(3.0096491810855,1.,2.87876560072799));
#37790=CARTESIAN_POINT('Ctrl Pts',(3.00686224485374,-1.,2.87146368430104));
#37791=CARTESIAN_POINT('Ctrl Pts',(3.00686224485374,1.,2.87146368430104));
#37792=CARTESIAN_POINT('Ctrl Pts',(3.00404638316245,-1.,2.86418200833065));
#37793=CARTESIAN_POINT('Ctrl Pts',(3.00404638316245,1.,2.86418200833065));
#37794=CARTESIAN_POINT('Ctrl Pts',(3.0012015079552,-1.,2.85692085715129));
#37795=CARTESIAN_POINT('Ctrl Pts',(3.0012015079552,1.,2.85692085715129));
#37796=CARTESIAN_POINT('Ctrl Pts',(2.99832751144566,-1.,2.84968053289104));
#37797=CARTESIAN_POINT('Ctrl Pts',(2.99832751144566,1.,2.84968053289104));
#37798=CARTESIAN_POINT('Ctrl Pts',(2.995424253416,-1.,2.84246132984334));
#37799=CARTESIAN_POINT('Ctrl Pts',(2.995424253416,1.,2.84246132984334));
#37800=CARTESIAN_POINT('Ctrl Pts',(2.99249155170479,-1.,2.83526351254383));
#37801=CARTESIAN_POINT('Ctrl Pts',(2.99249155170479,1.,2.83526351254383));
#37802=CARTESIAN_POINT('Ctrl Pts',(2.98952916401699,-1.,2.82808728190402));
#37803=CARTESIAN_POINT('Ctrl Pts',(2.98952916401699,1.,2.82808728190402));
#37804=CARTESIAN_POINT('Ctrl Pts',(2.98653680669434,-1.,2.82093279065704));
#37805=CARTESIAN_POINT('Ctrl Pts',(2.98653680669434,1.,2.82093279065704));
#37806=CARTESIAN_POINT('Ctrl Pts',(2.9835141977994,-1.,2.81380019196454));
#37807=CARTESIAN_POINT('Ctrl Pts',(2.9835141977994,1.,2.81380019196454));
#37808=CARTESIAN_POINT('Ctrl Pts',(2.98046109647299,-1.,2.80668968101162));
#37809=CARTESIAN_POINT('Ctrl Pts',(2.98046109647299,1.,2.80668968101162));
#37810=CARTESIAN_POINT('Ctrl Pts',(2.97737733718242,-1.,2.79960153278186));
#37811=CARTESIAN_POINT('Ctrl Pts',(2.97737733718242,1.,2.79960153278186));
#37812=CARTESIAN_POINT('Ctrl Pts',(2.97426288347475,-1.,2.79253615718147));
#37813=CARTESIAN_POINT('Ctrl Pts',(2.97426288347475,1.,2.79253615718147));
#37814=CARTESIAN_POINT('Ctrl Pts',(2.97111781461349,-1.,2.78549409123657));
#37815=CARTESIAN_POINT('Ctrl Pts',(2.97111781461349,1.,2.78549409123657));
#37816=CARTESIAN_POINT('Ctrl Pts',(2.9679422104295,-1.,2.77847589542767));
#37817=CARTESIAN_POINT('Ctrl Pts',(2.9679422104295,1.,2.77847589542767));
#37818=CARTESIAN_POINT('Ctrl Pts',(2.96473605585548,-1.,2.77148206836464));
#37819=CARTESIAN_POINT('Ctrl Pts',(2.96473605585548,1.,2.77148206836464));
#37820=CARTESIAN_POINT('Ctrl Pts',(2.96149914764832,-1.,2.76451296269571));
#37821=CARTESIAN_POINT('Ctrl Pts',(2.96149914764832,1.,2.76451296269571));
#37822=CARTESIAN_POINT('Ctrl Pts',(2.9582309766594,-1.,2.75756867888393));
#37823=CARTESIAN_POINT('Ctrl Pts',(2.9582309766594,1.,2.75756867888393));
#37824=CARTESIAN_POINT('Ctrl Pts',(2.95493069316211,-1.,2.75064903318996));
#37825=CARTESIAN_POINT('Ctrl Pts',(2.95493069316211,1.,2.75064903318996));
#37826=CARTESIAN_POINT('Ctrl Pts',(2.95159737214304,-1.,2.7437537949221));
#37827=CARTESIAN_POINT('Ctrl Pts',(2.95159737214304,1.,2.7437537949221));
#37828=CARTESIAN_POINT('Ctrl Pts',(2.94823023414381,-1.,2.73688288329825));
#37829=CARTESIAN_POINT('Ctrl Pts',(2.94823023414381,1.,2.73688288329825));
#37830=CARTESIAN_POINT('Ctrl Pts',(2.94482887675139,-1.,2.73003657371613));
#37831=CARTESIAN_POINT('Ctrl Pts',(2.94482887675139,1.,2.73003657371613));
#37832=CARTESIAN_POINT('Ctrl Pts',(2.94139351933882,-1.,2.72321571511322));
#37833=CARTESIAN_POINT('Ctrl Pts',(2.94139351933882,1.,2.72321571511322));
#37834=CARTESIAN_POINT('Ctrl Pts',(2.93792519474955,-1.,2.71642190053575));
#37835=CARTESIAN_POINT('Ctrl Pts',(2.93792519474955,1.,2.71642190053575));
#37836=CARTESIAN_POINT('Ctrl Pts',(2.93442516311167,-1.,2.70965695523776));
#37837=CARTESIAN_POINT('Ctrl Pts',(2.93442516311167,1.,2.70965695523776));
#37838=CARTESIAN_POINT('Ctrl Pts',(2.93089438233746,-1.,2.70292247416881));
#37839=CARTESIAN_POINT('Ctrl Pts',(2.93089438233746,1.,2.70292247416881));
#37840=CARTESIAN_POINT('Ctrl Pts',(2.92733294395268,-1.,2.69621932864302));
#37841=CARTESIAN_POINT('Ctrl Pts',(2.92733294395268,1.,2.69621932864302));
#37842=CARTESIAN_POINT('Ctrl Pts',(2.92373955325876,-1.,2.68954721165342));
#37843=CARTESIAN_POINT('Ctrl Pts',(2.92373955325876,1.,2.68954721165342));
#37844=CARTESIAN_POINT('Ctrl Pts',(2.92011090722152,-1.,2.68290409279689));
#37845=CARTESIAN_POINT('Ctrl Pts',(2.92011090722152,1.,2.68290409279689));
#37846=CARTESIAN_POINT('Ctrl Pts',(2.91644290704281,-1.,2.67628728855309));
#37847=CARTESIAN_POINT('Ctrl Pts',(2.91644290704281,1.,2.67628728855309));
#37848=CARTESIAN_POINT('Ctrl Pts',(2.91273193382876,-1.,2.66969458792627));
#37849=CARTESIAN_POINT('Ctrl Pts',(2.91273193382876,1.,2.66969458792627));
#37850=CARTESIAN_POINT('Ctrl Pts',(2.90897617968921,-1.,2.66312542616809));
#37851=CARTESIAN_POINT('Ctrl Pts',(2.90897617968921,1.,2.66312542616809));
#37852=CARTESIAN_POINT('Ctrl Pts',(2.90517678087467,-1.,2.65658188464287));
#37853=CARTESIAN_POINT('Ctrl Pts',(2.90517678087467,1.,2.65658188464287));
#37854=CARTESIAN_POINT('Ctrl Pts',(2.90133950224879,-1.,2.65007017365576));
#37855=CARTESIAN_POINT('Ctrl Pts',(2.90133950224879,1.,2.65007017365576));
#37856=CARTESIAN_POINT('Ctrl Pts',(2.89747231723361,-1.,2.64359851684146));
#37857=CARTESIAN_POINT('Ctrl Pts',(2.89747231723361,1.,2.64359851684146));
#37858=CARTESIAN_POINT('Ctrl Pts',(2.89358228854557,-1.,2.63717442263944));
#37859=CARTESIAN_POINT('Ctrl Pts',(2.89358228854557,1.,2.63717442263944));
#37860=CARTESIAN_POINT('Ctrl Pts',(2.88967244854243,-1.,2.63080195420771));
#37861=CARTESIAN_POINT('Ctrl Pts',(2.88967244854243,1.,2.63080195420771));
#37862=CARTESIAN_POINT('Ctrl Pts',(2.88573922195049,-1.,2.62447947640253));
#37863=CARTESIAN_POINT('Ctrl Pts',(2.88573922195049,1.,2.62447947640253));
#37864=CARTESIAN_POINT('Ctrl Pts',(2.88176821427502,-1.,2.61819596473087));
#37865=CARTESIAN_POINT('Ctrl Pts',(2.88176821427502,1.,2.61819596473087));
#37866=CARTESIAN_POINT('Ctrl Pts',(2.87773881947885,-1.,2.61193507170928));
#37867=CARTESIAN_POINT('Ctrl Pts',(2.87773881947885,1.,2.61193507170928));
#37868=CARTESIAN_POINT('Ctrl Pts',(2.87363176656475,-1.,2.6056817788128));
#37869=CARTESIAN_POINT('Ctrl Pts',(2.87363176656475,1.,2.6056817788128));
#37870=CARTESIAN_POINT('Ctrl Pts',(2.86943633170712,-1.,2.59942875223202));
#37871=CARTESIAN_POINT('Ctrl Pts',(2.86943633170712,1.,2.59942875223202));
#37872=CARTESIAN_POINT('Ctrl Pts',(2.86515629953528,-1.,2.59318160184921));
#37873=CARTESIAN_POINT('Ctrl Pts',(2.86515629953528,1.,2.59318160184921));
#37874=CARTESIAN_POINT('Ctrl Pts',(2.86081999003668,-1.,2.5869677064356));
#37875=CARTESIAN_POINT('Ctrl Pts',(2.86081999003668,1.,2.5869677064356));
#37876=CARTESIAN_POINT('Ctrl Pts',(2.85647171715147,-1.,2.58082875254407));
#37877=CARTESIAN_POINT('Ctrl Pts',(2.85647171715147,1.,2.58082875254407));
#37878=CARTESIAN_POINT('Ctrl Pts',(2.85215360144482,-1.,2.57480482727128));
#37879=CARTESIAN_POINT('Ctrl Pts',(2.85215360144482,1.,2.57480482727128));
#37880=CARTESIAN_POINT('Ctrl Pts',(2.84788893329091,-1.,2.56891984251743));
#37881=CARTESIAN_POINT('Ctrl Pts',(2.84788893329091,1.,2.56891984251743));
#37882=CARTESIAN_POINT('Ctrl Pts',(2.84366802680211,-1.,2.56316920798489));
#37883=CARTESIAN_POINT('Ctrl Pts',(2.84366802680211,1.,2.56316920798489));
#37884=CARTESIAN_POINT('Ctrl Pts',(2.83942515220699,-1.,2.55749952145165));
#37885=CARTESIAN_POINT('Ctrl Pts',(2.83942515220699,1.,2.55749952145165));
#37886=CARTESIAN_POINT('Ctrl Pts',(2.83505269592412,-1.,2.55182152806964));
#37887=CARTESIAN_POINT('Ctrl Pts',(2.83505269592412,1.,2.55182152806964));
#37888=CARTESIAN_POINT('Ctrl Pts',(2.83044254225794,-1.,2.54604736792542));
#37889=CARTESIAN_POINT('Ctrl Pts',(2.83044254225794,1.,2.54604736792542));
#37890=CARTESIAN_POINT('Ctrl Pts',(2.82552167649157,-1.,2.54012272520141));
#37891=CARTESIAN_POINT('Ctrl Pts',(2.82552167649157,1.,2.54012272520141));
#37892=CARTESIAN_POINT('Ctrl Pts',(2.82028550483744,-1.,2.53405679667463));
#37893=CARTESIAN_POINT('Ctrl Pts',(2.82028550483744,1.,2.53405679667463));
#37894=CARTESIAN_POINT('Ctrl Pts',(2.8148437904867,-1.,2.52796388055457));
#37895=CARTESIAN_POINT('Ctrl Pts',(2.8148437904867,1.,2.52796388055457));
#37896=CARTESIAN_POINT('Ctrl Pts',(2.80941521967234,-1.,2.52205778589922));
#37897=CARTESIAN_POINT('Ctrl Pts',(2.80941521967234,1.,2.52205778589922));
#37898=CARTESIAN_POINT('Ctrl Pts',(2.80427363984939,-1.,2.51660190466067));
#37899=CARTESIAN_POINT('Ctrl Pts',(2.80427363984939,1.,2.51660190466067));
#37900=CARTESIAN_POINT('Ctrl Pts',(2.79970585014308,-1.,2.51186983687947));
#37901=CARTESIAN_POINT('Ctrl Pts',(2.79970585014308,1.,2.51186983687947));
#37902=CARTESIAN_POINT('Ctrl Pts',(2.7959687805717,-1.,2.50810555977564));
#37903=CARTESIAN_POINT('Ctrl Pts',(2.7959687805717,1.,2.50810555977564));
#37904=CARTESIAN_POINT('Ctrl Pts',(2.79323694088143,-1.,2.50547439929077));
#37905=CARTESIAN_POINT('Ctrl Pts',(2.79323694088143,1.,2.50547439929077));
#37906=CARTESIAN_POINT('Ctrl Pts',(2.79192122906739,-1.,2.50433799076945));
#37907=CARTESIAN_POINT('Ctrl Pts',(2.79192122906739,1.,2.50433799076945));
#37908=CARTESIAN_POINT('Ctrl Pts',(2.79143626022225,-1.,2.50404230339032));
#37909=CARTESIAN_POINT('Ctrl Pts',(2.79143626022225,1.,2.50404230339032));
#37910=CARTESIAN_POINT('Ctrl Pts',(2.79133581100044,-1.,2.50409239460011));
#37911=CARTESIAN_POINT('Ctrl Pts',(2.79133581100044,1.,2.50409239460011));
#37912=CARTESIAN_POINT('Ctrl Pts',(2.79134130681569,-1.,2.50417924854921));
#37913=CARTESIAN_POINT('Ctrl Pts',(2.79134130681569,1.,2.50417924854921));
#37914=CARTESIAN_POINT('',(3.02314558451372,1.,2.91557726271063));
#37915=CARTESIAN_POINT('Ctrl Pts',(3.02314558451372,1.,2.91557726271063));
#37916=CARTESIAN_POINT('Ctrl Pts',(3.02261975104912,1.,2.91409518070707));
#37917=CARTESIAN_POINT('Ctrl Pts',(3.02156522743299,1.,2.91113297349052));
#37918=CARTESIAN_POINT('Ctrl Pts',(3.01997487194926,1.,2.90669553303902));
#37919=CARTESIAN_POINT('Ctrl Pts',(3.01783725123646,1.,2.90079069102661));
#37920=CARTESIAN_POINT('Ctrl Pts',(3.01513660433291,1.,2.8934292556764));
#37921=CARTESIAN_POINT('Ctrl Pts',(3.01240727309568,1.,2.88608751706796));
#37922=CARTESIAN_POINT('Ctrl Pts',(3.0096491810855,1.,2.87876560072799));
#37923=CARTESIAN_POINT('Ctrl Pts',(3.00686224485374,1.,2.87146368430104));
#37924=CARTESIAN_POINT('Ctrl Pts',(3.00404638316245,1.,2.86418200833065));
#37925=CARTESIAN_POINT('Ctrl Pts',(3.0012015079552,1.,2.85692085715129));
#37926=CARTESIAN_POINT('Ctrl Pts',(2.99832751144566,1.,2.84968053289104));
#37927=CARTESIAN_POINT('Ctrl Pts',(2.995424253416,1.,2.84246132984334));
#37928=CARTESIAN_POINT('Ctrl Pts',(2.99249155170479,1.,2.83526351254383));
#37929=CARTESIAN_POINT('Ctrl Pts',(2.98952916401699,1.,2.82808728190402));
#37930=CARTESIAN_POINT('Ctrl Pts',(2.98653680669434,1.,2.82093279065704));
#37931=CARTESIAN_POINT('Ctrl Pts',(2.9835141977994,1.,2.81380019196454));
#37932=CARTESIAN_POINT('Ctrl Pts',(2.98046109647299,1.,2.80668968101162));
#37933=CARTESIAN_POINT('Ctrl Pts',(2.97737733718242,1.,2.79960153278186));
#37934=CARTESIAN_POINT('Ctrl Pts',(2.97426288347475,1.,2.79253615718147));
#37935=CARTESIAN_POINT('Ctrl Pts',(2.97111781461349,1.,2.78549409123657));
#37936=CARTESIAN_POINT('Ctrl Pts',(2.9679422104295,1.,2.77847589542767));
#37937=CARTESIAN_POINT('Ctrl Pts',(2.96473605585548,1.,2.77148206836464));
#37938=CARTESIAN_POINT('Ctrl Pts',(2.96149914764832,1.,2.76451296269571));
#37939=CARTESIAN_POINT('Ctrl Pts',(2.9582309766594,1.,2.75756867888393));
#37940=CARTESIAN_POINT('Ctrl Pts',(2.95493069316211,1.,2.75064903318996));
#37941=CARTESIAN_POINT('Ctrl Pts',(2.95159737214304,1.,2.7437537949221));
#37942=CARTESIAN_POINT('Ctrl Pts',(2.94823023414381,1.,2.73688288329825));
#37943=CARTESIAN_POINT('Ctrl Pts',(2.94482887675139,1.,2.73003657371613));
#37944=CARTESIAN_POINT('Ctrl Pts',(2.94139351933882,1.,2.72321571511322));
#37945=CARTESIAN_POINT('Ctrl Pts',(2.93792519474955,1.,2.71642190053575));
#37946=CARTESIAN_POINT('Ctrl Pts',(2.93442516311167,1.,2.70965695523776));
#37947=CARTESIAN_POINT('Ctrl Pts',(2.93089438233746,1.,2.70292247416881));
#37948=CARTESIAN_POINT('Ctrl Pts',(2.92733294395268,1.,2.69621932864302));
#37949=CARTESIAN_POINT('Ctrl Pts',(2.92373955325876,1.,2.68954721165342));
#37950=CARTESIAN_POINT('Ctrl Pts',(2.92011090722152,1.,2.68290409279689));
#37951=CARTESIAN_POINT('Ctrl Pts',(2.91644290704281,1.,2.67628728855309));
#37952=CARTESIAN_POINT('Ctrl Pts',(2.91273193382876,1.,2.66969458792627));
#37953=CARTESIAN_POINT('Ctrl Pts',(2.90897617968921,1.,2.66312542616809));
#37954=CARTESIAN_POINT('Ctrl Pts',(2.90517678087467,1.,2.65658188464287));
#37955=CARTESIAN_POINT('Ctrl Pts',(2.90133950224879,1.,2.65007017365576));
#37956=CARTESIAN_POINT('Ctrl Pts',(2.89747231723361,1.,2.64359851684146));
#37957=CARTESIAN_POINT('Ctrl Pts',(2.89358228854557,1.,2.63717442263944));
#37958=CARTESIAN_POINT('Ctrl Pts',(2.88967244854243,1.,2.63080195420771));
#37959=CARTESIAN_POINT('Ctrl Pts',(2.88573922195049,1.,2.62447947640253));
#37960=CARTESIAN_POINT('Ctrl Pts',(2.88176821427502,1.,2.61819596473087));
#37961=CARTESIAN_POINT('Ctrl Pts',(2.87773881947885,1.,2.61193507170928));
#37962=CARTESIAN_POINT('Ctrl Pts',(2.87363176656475,1.,2.6056817788128));
#37963=CARTESIAN_POINT('Ctrl Pts',(2.86943633170712,1.,2.59942875223202));
#37964=CARTESIAN_POINT('Ctrl Pts',(2.86515629953528,1.,2.59318160184921));
#37965=CARTESIAN_POINT('Ctrl Pts',(2.86081999003668,1.,2.5869677064356));
#37966=CARTESIAN_POINT('Ctrl Pts',(2.85647171715147,1.,2.58082875254407));
#37967=CARTESIAN_POINT('Ctrl Pts',(2.85215360144482,1.,2.57480482727128));
#37968=CARTESIAN_POINT('Ctrl Pts',(2.84788893329091,1.,2.56891984251743));
#37969=CARTESIAN_POINT('Ctrl Pts',(2.84366802680211,1.,2.56316920798489));
#37970=CARTESIAN_POINT('Ctrl Pts',(2.83942515220699,1.,2.55749952145165));
#37971=CARTESIAN_POINT('Ctrl Pts',(2.83505269592412,1.,2.55182152806964));
#37972=CARTESIAN_POINT('Ctrl Pts',(2.83044254225794,1.,2.54604736792542));
#37973=CARTESIAN_POINT('Ctrl Pts',(2.82552167649157,1.,2.54012272520141));
#37974=CARTESIAN_POINT('Ctrl Pts',(2.82028550483744,1.,2.53405679667463));
#37975=CARTESIAN_POINT('Ctrl Pts',(2.8148437904867,1.,2.52796388055457));
#37976=CARTESIAN_POINT('Ctrl Pts',(2.80941521967234,1.,2.52205778589922));
#37977=CARTESIAN_POINT('Ctrl Pts',(2.80427363984939,1.,2.51660190466067));
#37978=CARTESIAN_POINT('Ctrl Pts',(2.79970585014308,1.,2.51186983687947));
#37979=CARTESIAN_POINT('Ctrl Pts',(2.7959687805717,1.,2.50810555977564));
#37980=CARTESIAN_POINT('Ctrl Pts',(2.79344192164204,1.,2.50567182569153));
#37981=CARTESIAN_POINT('Ctrl Pts',(2.79217568804874,1.,2.50455968395235));
#37982=CARTESIAN_POINT('Ctrl Pts',(2.79164172519039,1.,2.50417932839344));
#37983=CARTESIAN_POINT('Ctrl Pts',(2.79145823440899,1.,2.50410700351426));
#37984=CARTESIAN_POINT('Ctrl Pts',(2.79140942341378,1.,2.50410331873042));
#37985=CARTESIAN_POINT('',(3.02314558451372,0.,2.91557726271063));
#37986=CARTESIAN_POINT('Ctrl Pts',(2.5041792485492,-1.,2.79134130681569));
#37987=CARTESIAN_POINT('Ctrl Pts',(2.5041792485492,1.,2.79134130681569));
#37988=CARTESIAN_POINT('Ctrl Pts',(2.50409239460108,-1.,2.7913358110015));
#37989=CARTESIAN_POINT('Ctrl Pts',(2.50409239460108,1.,2.7913358110015));
#37990=CARTESIAN_POINT('Ctrl Pts',(2.50404230339286,-1.,2.79143626022503));
#37991=CARTESIAN_POINT('Ctrl Pts',(2.50404230339286,1.,2.79143626022503));
#37992=CARTESIAN_POINT('Ctrl Pts',(2.5043379907732,-1.,2.79192122907148));
#37993=CARTESIAN_POINT('Ctrl Pts',(2.5043379907732,1.,2.79192122907148));
#37994=CARTESIAN_POINT('Ctrl Pts',(2.50547439929414,-1.,2.7932369408851));
#37995=CARTESIAN_POINT('Ctrl Pts',(2.50547439929414,1.,2.7932369408851));
#37996=CARTESIAN_POINT('Ctrl Pts',(2.5081055597767,-1.,2.79596878057287));
#37997=CARTESIAN_POINT('Ctrl Pts',(2.5081055597767,1.,2.79596878057287));
#37998=CARTESIAN_POINT('Ctrl Pts',(2.51186983687818,-1.,2.79970585014168));
#37999=CARTESIAN_POINT('Ctrl Pts',(2.51186983687818,1.,2.79970585014168));
#38000=CARTESIAN_POINT('Ctrl Pts',(2.51660190465805,-1.,2.80427363984653));
#38001=CARTESIAN_POINT('Ctrl Pts',(2.51660190465805,1.,2.80427363984653));
#38002=CARTESIAN_POINT('Ctrl Pts',(2.52205778589653,-1.,2.80941521966941));
#38003=CARTESIAN_POINT('Ctrl Pts',(2.52205778589653,1.,2.80941521966941));
#38004=CARTESIAN_POINT('Ctrl Pts',(2.52796388055278,-1.,2.81484379048475));
#38005=CARTESIAN_POINT('Ctrl Pts',(2.52796388055278,1.,2.81484379048475));
#38006=CARTESIAN_POINT('Ctrl Pts',(2.53405679667412,-1.,2.82028550483689));
#38007=CARTESIAN_POINT('Ctrl Pts',(2.53405679667412,1.,2.82028550483689));
#38008=CARTESIAN_POINT('Ctrl Pts',(2.54012272520199,-1.,2.8255216764922));
#38009=CARTESIAN_POINT('Ctrl Pts',(2.54012272520199,1.,2.8255216764922));
#38010=CARTESIAN_POINT('Ctrl Pts',(2.54604736792655,-1.,2.83044254225917));
#38011=CARTESIAN_POINT('Ctrl Pts',(2.54604736792655,1.,2.83044254225917));
#38012=CARTESIAN_POINT('Ctrl Pts',(2.55182152807077,-1.,2.83505269592536));
#38013=CARTESIAN_POINT('Ctrl Pts',(2.55182152807077,1.,2.83505269592536));
#38014=CARTESIAN_POINT('Ctrl Pts',(2.55749952145241,-1.,2.83942515220782));
#38015=CARTESIAN_POINT('Ctrl Pts',(2.55749952145241,1.,2.83942515220782));
#38016=CARTESIAN_POINT('Ctrl Pts',(2.56316920798513,-1.,2.84366802680237));
#38017=CARTESIAN_POINT('Ctrl Pts',(2.56316920798513,1.,2.84366802680237));
#38018=CARTESIAN_POINT('Ctrl Pts',(2.56891984251721,-1.,2.84788893329067));
#38019=CARTESIAN_POINT('Ctrl Pts',(2.56891984251721,1.,2.84788893329067));
#38020=CARTESIAN_POINT('Ctrl Pts',(2.57480482727081,-1.,2.85215360144431));
#38021=CARTESIAN_POINT('Ctrl Pts',(2.57480482727081,1.,2.85215360144431));
#38022=CARTESIAN_POINT('Ctrl Pts',(2.58082875254357,-1.,2.85647171715092));
#38023=CARTESIAN_POINT('Ctrl Pts',(2.58082875254357,1.,2.85647171715092));
#38024=CARTESIAN_POINT('Ctrl Pts',(2.58696770643524,-1.,2.86081999003629));
#38025=CARTESIAN_POINT('Ctrl Pts',(2.58696770643524,1.,2.86081999003629));
#38026=CARTESIAN_POINT('Ctrl Pts',(2.59318160184908,-1.,2.86515629953513));
#38027=CARTESIAN_POINT('Ctrl Pts',(2.59318160184908,1.,2.86515629953513));
#38028=CARTESIAN_POINT('Ctrl Pts',(2.5994287522321,-1.,2.86943633170722));
#38029=CARTESIAN_POINT('Ctrl Pts',(2.5994287522321,1.,2.86943633170722));
#38030=CARTESIAN_POINT('Ctrl Pts',(2.60568177881303,-1.,2.87363176656501));
#38031=CARTESIAN_POINT('Ctrl Pts',(2.60568177881303,1.,2.87363176656501));
#38032=CARTESIAN_POINT('Ctrl Pts',(2.61193507170955,-1.,2.87773881947916));
#38033=CARTESIAN_POINT('Ctrl Pts',(2.61193507170955,1.,2.87773881947916));
#38034=CARTESIAN_POINT('Ctrl Pts',(2.61819596473108,-1.,2.88176821427525));
#38035=CARTESIAN_POINT('Ctrl Pts',(2.61819596473108,1.,2.88176821427525));
#38036=CARTESIAN_POINT('Ctrl Pts',(2.62447947640262,-1.,2.88573922195059));
#38037=CARTESIAN_POINT('Ctrl Pts',(2.62447947640262,1.,2.88573922195059));
#38038=CARTESIAN_POINT('Ctrl Pts',(2.63080195420767,-1.,2.88967244854239));
#38039=CARTESIAN_POINT('Ctrl Pts',(2.63080195420767,1.,2.88967244854239));
#38040=CARTESIAN_POINT('Ctrl Pts',(2.63717442263932,-1.,2.89358228854544));
#38041=CARTESIAN_POINT('Ctrl Pts',(2.63717442263932,1.,2.89358228854544));
#38042=CARTESIAN_POINT('Ctrl Pts',(2.64359851684131,-1.,2.89747231723345));
#38043=CARTESIAN_POINT('Ctrl Pts',(2.64359851684131,1.,2.89747231723345));
#38044=CARTESIAN_POINT('Ctrl Pts',(2.65007017365564,-1.,2.90133950224867));
#38045=CARTESIAN_POINT('Ctrl Pts',(2.65007017365564,1.,2.90133950224867));
#38046=CARTESIAN_POINT('Ctrl Pts',(2.65658188464282,-1.,2.90517678087461));
#38047=CARTESIAN_POINT('Ctrl Pts',(2.65658188464282,1.,2.90517678087461));
#38048=CARTESIAN_POINT('Ctrl Pts',(2.6631254261681,-1.,2.90897617968923));
#38049=CARTESIAN_POINT('Ctrl Pts',(2.6631254261681,1.,2.90897617968923));
#38050=CARTESIAN_POINT('Ctrl Pts',(2.66969458792631,-1.,2.91273193382882));
#38051=CARTESIAN_POINT('Ctrl Pts',(2.66969458792631,1.,2.91273193382882));
#38052=CARTESIAN_POINT('Ctrl Pts',(2.67628728855312,-1.,2.91644290704285));
#38053=CARTESIAN_POINT('Ctrl Pts',(2.67628728855312,1.,2.91644290704285));
#38054=CARTESIAN_POINT('Ctrl Pts',(2.68290409279688,-1.,2.92011090722152));
#38055=CARTESIAN_POINT('Ctrl Pts',(2.68290409279688,1.,2.92011090722152));
#38056=CARTESIAN_POINT('Ctrl Pts',(2.68954721165339,-1.,2.92373955325875));
#38057=CARTESIAN_POINT('Ctrl Pts',(2.68954721165339,1.,2.92373955325875));
#38058=CARTESIAN_POINT('Ctrl Pts',(2.69621932864301,-1.,2.92733294395267));
#38059=CARTESIAN_POINT('Ctrl Pts',(2.69621932864301,1.,2.92733294395267));
#38060=CARTESIAN_POINT('Ctrl Pts',(2.70292247416885,-1.,2.9308943823375));
#38061=CARTESIAN_POINT('Ctrl Pts',(2.70292247416885,1.,2.9308943823375));
#38062=CARTESIAN_POINT('Ctrl Pts',(2.70965695523787,-1.,2.93442516311179));
#38063=CARTESIAN_POINT('Ctrl Pts',(2.70965695523787,1.,2.93442516311179));
#38064=CARTESIAN_POINT('Ctrl Pts',(2.71642190053592,-1.,2.93792519474972));
#38065=CARTESIAN_POINT('Ctrl Pts',(2.71642190053592,1.,2.93792519474972));
#38066=CARTESIAN_POINT('Ctrl Pts',(2.72321571511337,-1.,2.94139351933897));
#38067=CARTESIAN_POINT('Ctrl Pts',(2.72321571511337,1.,2.94139351933897));
#38068=CARTESIAN_POINT('Ctrl Pts',(2.73003657371616,-1.,2.94482887675143));
#38069=CARTESIAN_POINT('Ctrl Pts',(2.73003657371616,1.,2.94482887675143));
#38070=CARTESIAN_POINT('Ctrl Pts',(2.73688288329808,-1.,2.94823023414364));
#38071=CARTESIAN_POINT('Ctrl Pts',(2.73688288329808,1.,2.94823023414364));
#38072=CARTESIAN_POINT('Ctrl Pts',(2.74375379492172,-1.,2.95159737214266));
#38073=CARTESIAN_POINT('Ctrl Pts',(2.74375379492172,1.,2.95159737214266));
#38074=CARTESIAN_POINT('Ctrl Pts',(2.75064903318947,-1.,2.95493069316161));
#38075=CARTESIAN_POINT('Ctrl Pts',(2.75064903318947,1.,2.95493069316161));
#38076=CARTESIAN_POINT('Ctrl Pts',(2.7575686788835,-1.,2.95823097665896));
#38077=CARTESIAN_POINT('Ctrl Pts',(2.7575686788835,1.,2.95823097665896));
#38078=CARTESIAN_POINT('Ctrl Pts',(2.76451296269557,-1.,2.96149914764818));
#38079=CARTESIAN_POINT('Ctrl Pts',(2.76451296269557,1.,2.96149914764818));
#38080=CARTESIAN_POINT('Ctrl Pts',(2.77148206836498,-1.,2.96473605585583));
#38081=CARTESIAN_POINT('Ctrl Pts',(2.77148206836498,1.,2.96473605585583));
#38082=CARTESIAN_POINT('Ctrl Pts',(2.7784758954285,-1.,2.96794221043036));
#38083=CARTESIAN_POINT('Ctrl Pts',(2.7784758954285,1.,2.96794221043036));
#38084=CARTESIAN_POINT('Ctrl Pts',(2.78549409123769,-1.,2.97111781461465));
#38085=CARTESIAN_POINT('Ctrl Pts',(2.78549409123769,1.,2.97111781461465));
#38086=CARTESIAN_POINT('Ctrl Pts',(2.79253615718248,-1.,2.9742628834758));
#38087=CARTESIAN_POINT('Ctrl Pts',(2.79253615718248,1.,2.9742628834758));
#38088=CARTESIAN_POINT('Ctrl Pts',(2.7996015327823,-1.,2.97737733718287));
#38089=CARTESIAN_POINT('Ctrl Pts',(2.7996015327823,1.,2.97737733718287));
#38090=CARTESIAN_POINT('Ctrl Pts',(2.80668968101106,-1.,2.98046109647241));
#38091=CARTESIAN_POINT('Ctrl Pts',(2.80668968101106,1.,2.98046109647241));
#38092=CARTESIAN_POINT('Ctrl Pts',(2.81380019196286,-1.,2.98351419779767));
#38093=CARTESIAN_POINT('Ctrl Pts',(2.81380019196286,1.,2.98351419779767));
#38094=CARTESIAN_POINT('Ctrl Pts',(2.82093279065457,-1.,2.9865368066918));
#38095=CARTESIAN_POINT('Ctrl Pts',(2.82093279065457,1.,2.9865368066918));
#38096=CARTESIAN_POINT('Ctrl Pts',(2.82808728190157,-1.,2.98952916401446));
#38097=CARTESIAN_POINT('Ctrl Pts',(2.82808728190157,1.,2.98952916401446));
#38098=CARTESIAN_POINT('Ctrl Pts',(2.83526351254248,-1.,2.9924915517034));
#38099=CARTESIAN_POINT('Ctrl Pts',(2.83526351254248,1.,2.9924915517034));
#38100=CARTESIAN_POINT('Ctrl Pts',(2.84246132984415,-1.,2.99542425341685));
#38101=CARTESIAN_POINT('Ctrl Pts',(2.84246132984415,1.,2.99542425341685));
#38102=CARTESIAN_POINT('Ctrl Pts',(2.84968053289451,-1.,2.99832751144925));
#38103=CARTESIAN_POINT('Ctrl Pts',(2.84968053289451,1.,2.99832751144925));
#38104=CARTESIAN_POINT('Ctrl Pts',(2.85692085715685,-1.,3.00120150796095));
#38105=CARTESIAN_POINT('Ctrl Pts',(2.85692085715685,1.,3.00120150796095));
#38106=CARTESIAN_POINT('Ctrl Pts',(2.86418200833667,-1.,3.00404638316867));
#38107=CARTESIAN_POINT('Ctrl Pts',(2.86418200833667,1.,3.00404638316867));
#38108=CARTESIAN_POINT('Ctrl Pts',(2.87146368430501,-1.,3.00686224485784));
#38109=CARTESIAN_POINT('Ctrl Pts',(2.87146368430501,1.,3.00686224485784));
#38110=CARTESIAN_POINT('Ctrl Pts',(2.87876560072727,-1.,3.00964918108476));
#38111=CARTESIAN_POINT('Ctrl Pts',(2.87876560072727,1.,3.00964918108476));
#38112=CARTESIAN_POINT('Ctrl Pts',(2.8860875170608,-1.,3.01240727308829));
#38113=CARTESIAN_POINT('Ctrl Pts',(2.8860875170608,1.,3.01240727308829));
#38114=CARTESIAN_POINT('Ctrl Pts',(2.89342925566321,-1.,3.01513660431928));
#38115=CARTESIAN_POINT('Ctrl Pts',(2.89342925566321,1.,3.01513660431928));
#38116=CARTESIAN_POINT('Ctrl Pts',(2.9007906910105,-1.,3.01783725121981));
#38117=CARTESIAN_POINT('Ctrl Pts',(2.9007906910105,1.,3.01783725121981));
#38118=CARTESIAN_POINT('Ctrl Pts',(2.90669553302526,-1.,3.01997487193503));
#38119=CARTESIAN_POINT('Ctrl Pts',(2.90669553302526,1.,3.01997487193503));
#38120=CARTESIAN_POINT('Ctrl Pts',(2.91113297348212,-1.,3.02156522742431));
#38121=CARTESIAN_POINT('Ctrl Pts',(2.91113297348212,1.,3.02156522742431));
#38122=CARTESIAN_POINT('Ctrl Pts',(2.91409518070399,-1.,3.02261975104593));
#38123=CARTESIAN_POINT('Ctrl Pts',(2.91409518070399,1.,3.02261975104593));
#38124=CARTESIAN_POINT('Ctrl Pts',(2.91557726271063,-1.,3.02314558451372));
#38125=CARTESIAN_POINT('Ctrl Pts',(2.91557726271063,1.,3.02314558451372));
#38126=CARTESIAN_POINT('',(2.50410331873176,1.,2.79140942341258));
#38127=CARTESIAN_POINT('Ctrl Pts',(2.50410331873176,-1.,2.79140942341258));
#38128=CARTESIAN_POINT('Ctrl Pts',(2.50410331873176,-0.666666666666667,
2.79140942341258));
#38129=CARTESIAN_POINT('Ctrl Pts',(2.50410331873176,-0.333333333333333,
2.79140942341258));
#38130=CARTESIAN_POINT('Ctrl Pts',(2.50410331873176,0.333333333333333,2.79140942341258));
#38131=CARTESIAN_POINT('Ctrl Pts',(2.50410331873176,0.666666666666667,2.79140942341258));
#38132=CARTESIAN_POINT('Ctrl Pts',(2.50410331873176,1.,2.79140942341258));
#38133=CARTESIAN_POINT('',(2.91557726271063,1.,3.02314558451372));
#38134=CARTESIAN_POINT('',(2.91557726271063,0.,3.02314558451372));
#38135=CARTESIAN_POINT('Ctrl Pts',(2.50410331873176,1.,2.79140942341258));
#38136=CARTESIAN_POINT('Ctrl Pts',(2.50410700351493,1.,2.79145823440781));
#38137=CARTESIAN_POINT('Ctrl Pts',(2.50417932839313,1.,2.79164172518905));
#38138=CARTESIAN_POINT('Ctrl Pts',(2.50455968395146,1.,2.79217568804755));
#38139=CARTESIAN_POINT('Ctrl Pts',(2.50567182569081,1.,2.79344192164147));
#38140=CARTESIAN_POINT('Ctrl Pts',(2.5081055597767,1.,2.79596878057287));
#38141=CARTESIAN_POINT('Ctrl Pts',(2.51186983687818,1.,2.79970585014168));
#38142=CARTESIAN_POINT('Ctrl Pts',(2.51660190465805,1.,2.80427363984653));
#38143=CARTESIAN_POINT('Ctrl Pts',(2.52205778589653,1.,2.80941521966941));
#38144=CARTESIAN_POINT('Ctrl Pts',(2.52796388055278,1.,2.81484379048475));
#38145=CARTESIAN_POINT('Ctrl Pts',(2.53405679667412,1.,2.82028550483689));
#38146=CARTESIAN_POINT('Ctrl Pts',(2.54012272520199,1.,2.8255216764922));
#38147=CARTESIAN_POINT('Ctrl Pts',(2.54604736792655,1.,2.83044254225917));
#38148=CARTESIAN_POINT('Ctrl Pts',(2.55182152807077,1.,2.83505269592536));
#38149=CARTESIAN_POINT('Ctrl Pts',(2.55749952145241,1.,2.83942515220782));
#38150=CARTESIAN_POINT('Ctrl Pts',(2.56316920798513,1.,2.84366802680237));
#38151=CARTESIAN_POINT('Ctrl Pts',(2.56891984251721,1.,2.84788893329067));
#38152=CARTESIAN_POINT('Ctrl Pts',(2.57480482727081,1.,2.85215360144431));
#38153=CARTESIAN_POINT('Ctrl Pts',(2.58082875254357,1.,2.85647171715092));
#38154=CARTESIAN_POINT('Ctrl Pts',(2.58696770643524,1.,2.86081999003629));
#38155=CARTESIAN_POINT('Ctrl Pts',(2.59318160184908,1.,2.86515629953513));
#38156=CARTESIAN_POINT('Ctrl Pts',(2.5994287522321,1.,2.86943633170722));
#38157=CARTESIAN_POINT('Ctrl Pts',(2.60568177881303,1.,2.87363176656501));
#38158=CARTESIAN_POINT('Ctrl Pts',(2.61193507170955,1.,2.87773881947916));
#38159=CARTESIAN_POINT('Ctrl Pts',(2.61819596473108,1.,2.88176821427525));
#38160=CARTESIAN_POINT('Ctrl Pts',(2.62447947640262,1.,2.88573922195059));
#38161=CARTESIAN_POINT('Ctrl Pts',(2.63080195420767,1.,2.88967244854239));
#38162=CARTESIAN_POINT('Ctrl Pts',(2.63717442263932,1.,2.89358228854544));
#38163=CARTESIAN_POINT('Ctrl Pts',(2.64359851684131,1.,2.89747231723345));
#38164=CARTESIAN_POINT('Ctrl Pts',(2.65007017365564,1.,2.90133950224867));
#38165=CARTESIAN_POINT('Ctrl Pts',(2.65658188464282,1.,2.90517678087461));
#38166=CARTESIAN_POINT('Ctrl Pts',(2.6631254261681,1.,2.90897617968923));
#38167=CARTESIAN_POINT('Ctrl Pts',(2.66969458792631,1.,2.91273193382882));
#38168=CARTESIAN_POINT('Ctrl Pts',(2.67628728855312,1.,2.91644290704285));
#38169=CARTESIAN_POINT('Ctrl Pts',(2.68290409279688,1.,2.92011090722152));
#38170=CARTESIAN_POINT('Ctrl Pts',(2.68954721165339,1.,2.92373955325875));
#38171=CARTESIAN_POINT('Ctrl Pts',(2.69621932864301,1.,2.92733294395267));
#38172=CARTESIAN_POINT('Ctrl Pts',(2.70292247416885,1.,2.9308943823375));
#38173=CARTESIAN_POINT('Ctrl Pts',(2.70965695523787,1.,2.93442516311179));
#38174=CARTESIAN_POINT('Ctrl Pts',(2.71642190053592,1.,2.93792519474972));
#38175=CARTESIAN_POINT('Ctrl Pts',(2.72321571511337,1.,2.94139351933897));
#38176=CARTESIAN_POINT('Ctrl Pts',(2.73003657371616,1.,2.94482887675143));
#38177=CARTESIAN_POINT('Ctrl Pts',(2.73688288329808,1.,2.94823023414364));
#38178=CARTESIAN_POINT('Ctrl Pts',(2.74375379492172,1.,2.95159737214266));
#38179=CARTESIAN_POINT('Ctrl Pts',(2.75064903318947,1.,2.95493069316161));
#38180=CARTESIAN_POINT('Ctrl Pts',(2.7575686788835,1.,2.95823097665896));
#38181=CARTESIAN_POINT('Ctrl Pts',(2.76451296269557,1.,2.96149914764818));
#38182=CARTESIAN_POINT('Ctrl Pts',(2.77148206836498,1.,2.96473605585583));
#38183=CARTESIAN_POINT('Ctrl Pts',(2.7784758954285,1.,2.96794221043036));
#38184=CARTESIAN_POINT('Ctrl Pts',(2.78549409123769,1.,2.97111781461465));
#38185=CARTESIAN_POINT('Ctrl Pts',(2.79253615718248,1.,2.9742628834758));
#38186=CARTESIAN_POINT('Ctrl Pts',(2.7996015327823,1.,2.97737733718287));
#38187=CARTESIAN_POINT('Ctrl Pts',(2.80668968101106,1.,2.98046109647241));
#38188=CARTESIAN_POINT('Ctrl Pts',(2.81380019196286,1.,2.98351419779767));
#38189=CARTESIAN_POINT('Ctrl Pts',(2.82093279065457,1.,2.9865368066918));
#38190=CARTESIAN_POINT('Ctrl Pts',(2.82808728190157,1.,2.98952916401446));
#38191=CARTESIAN_POINT('Ctrl Pts',(2.83526351254248,1.,2.9924915517034));
#38192=CARTESIAN_POINT('Ctrl Pts',(2.84246132984415,1.,2.99542425341685));
#38193=CARTESIAN_POINT('Ctrl Pts',(2.84968053289451,1.,2.99832751144925));
#38194=CARTESIAN_POINT('Ctrl Pts',(2.85692085715685,1.,3.00120150796095));
#38195=CARTESIAN_POINT('Ctrl Pts',(2.86418200833667,1.,3.00404638316867));
#38196=CARTESIAN_POINT('Ctrl Pts',(2.87146368430501,1.,3.00686224485784));
#38197=CARTESIAN_POINT('Ctrl Pts',(2.87876560072727,1.,3.00964918108476));
#38198=CARTESIAN_POINT('Ctrl Pts',(2.8860875170608,1.,3.01240727308829));
#38199=CARTESIAN_POINT('Ctrl Pts',(2.89342925566321,1.,3.01513660431928));
#38200=CARTESIAN_POINT('Ctrl Pts',(2.9007906910105,1.,3.01783725121981));
#38201=CARTESIAN_POINT('Ctrl Pts',(2.90669553302526,1.,3.01997487193503));
#38202=CARTESIAN_POINT('Ctrl Pts',(2.91113297348212,1.,3.02156522742431));
#38203=CARTESIAN_POINT('Ctrl Pts',(2.91409518070399,1.,3.02261975104593));
#38204=CARTESIAN_POINT('Ctrl Pts',(2.91557726271063,1.,3.02314558451372));
#38205=CARTESIAN_POINT('Origin',(2.91557726271063,0.,3.02314558451372));
#38206=CARTESIAN_POINT('',(3.02314558451372,1.,2.91557726271063));
#38207=CARTESIAN_POINT('Origin',(0.,0.,0.));
#38208=CARTESIAN_POINT('',(2.36531447826213,1.,2.90994629141562));
#38209=CARTESIAN_POINT('Origin',(0.,1.,0.));
#38210=CARTESIAN_POINT('Ctrl Pts',(2.36531447826213,1.,2.90994629141563));
#38211=CARTESIAN_POINT('Ctrl Pts',(2.36531447826213,0.666666666666667,2.90994629141563));
#38212=CARTESIAN_POINT('Ctrl Pts',(2.36531447826213,0.333333333333333,2.90994629141563));
#38213=CARTESIAN_POINT('Ctrl Pts',(2.36531447826213,-0.333333333333333,
2.90994629141563));
#38214=CARTESIAN_POINT('Ctrl Pts',(2.36531447826213,-0.666666666666667,
2.90994629141563));
#38215=CARTESIAN_POINT('Ctrl Pts',(2.36531447826213,-1.,2.90994629141563));
#38216=CARTESIAN_POINT('Ctrl Pts',(2.52982887637028,-1.,3.35260583073571));
#38217=CARTESIAN_POINT('Ctrl Pts',(2.52982887637028,1.,3.35260583073571));
#38218=CARTESIAN_POINT('Ctrl Pts',(2.52954136549357,-1.,3.35105973714426));
#38219=CARTESIAN_POINT('Ctrl Pts',(2.52954136549357,1.,3.35105973714426));
#38220=CARTESIAN_POINT('Ctrl Pts',(2.5289632161143,-1.,3.34796903577628));
#38221=CARTESIAN_POINT('Ctrl Pts',(2.5289632161143,1.,3.34796903577628));
#38222=CARTESIAN_POINT('Ctrl Pts',(2.52808660916879,-1.,3.34333744117093));
#38223=CARTESIAN_POINT('Ctrl Pts',(2.52808660916879,1.,3.34333744117093));
#38224=CARTESIAN_POINT('Ctrl Pts',(2.52689902691551,-1.,3.33717090000955));
#38225=CARTESIAN_POINT('Ctrl Pts',(2.52689902691551,1.,3.33717090000955));
#38226=CARTESIAN_POINT('Ctrl Pts',(2.52538321165774,-1.,3.32947762189049));
#38227=CARTESIAN_POINT('Ctrl Pts',(2.52538321165774,1.,3.32947762189049));
#38228=CARTESIAN_POINT('Ctrl Pts',(2.52383598396878,-1.,3.32179931079521));
#38229=CARTESIAN_POINT('Ctrl Pts',(2.52383598396878,1.,3.32179931079521));
#38230=CARTESIAN_POINT('Ctrl Pts',(2.52225724871375,-1.,3.31413607874727));
#38231=CARTESIAN_POINT('Ctrl Pts',(2.52225724871375,1.,3.31413607874727));
#38232=CARTESIAN_POINT('Ctrl Pts',(2.52064689568167,-1.,3.30648808814986));
#38233=CARTESIAN_POINT('Ctrl Pts',(2.52064689568167,1.,3.30648808814986));
#38234=CARTESIAN_POINT('Ctrl Pts',(2.51900480700548,-1.,3.29885556387661));
#38235=CARTESIAN_POINT('Ctrl Pts',(2.51900480700548,1.,3.29885556387661));
#38236=CARTESIAN_POINT('Ctrl Pts',(2.51733085123316,-1.,3.2912387729863));
#38237=CARTESIAN_POINT('Ctrl Pts',(2.51733085123316,1.,3.2912387729863));
#38238=CARTESIAN_POINT('Ctrl Pts',(2.51562487464214,-1.,3.28363799702583));
#38239=CARTESIAN_POINT('Ctrl Pts',(2.51562487464214,1.,3.28363799702583));
#38240=CARTESIAN_POINT('Ctrl Pts',(2.51388669270329,-1.,3.27605350473048));
#38241=CARTESIAN_POINT('Ctrl Pts',(2.51388669270329,1.,3.27605350473048));
#38242=CARTESIAN_POINT('Ctrl Pts',(2.51211608411539,-1.,3.26848552888271));
#38243=CARTESIAN_POINT('Ctrl Pts',(2.51211608411539,1.,3.26848552888271));
#38244=CARTESIAN_POINT('Ctrl Pts',(2.51031277813697,-1.,3.26093423001716));
#38245=CARTESIAN_POINT('Ctrl Pts',(2.51031277813697,1.,3.26093423001716));
#38246=CARTESIAN_POINT('Ctrl Pts',(2.50847647070936,-1.,3.25339971461265));
#38247=CARTESIAN_POINT('Ctrl Pts',(2.50847647070936,1.,3.25339971461265));
#38248=CARTESIAN_POINT('Ctrl Pts',(2.50660685940645,-1.,3.24588208984042));
#38249=CARTESIAN_POINT('Ctrl Pts',(2.50660685940645,1.,3.24588208984042));
#38250=CARTESIAN_POINT('Ctrl Pts',(2.50470367580078,-1.,3.23838151080383));
#38251=CARTESIAN_POINT('Ctrl Pts',(2.50470367580078,1.,3.23838151080383));
#38252=CARTESIAN_POINT('Ctrl Pts',(2.50276671338074,-1.,3.23089822320596));
#38253=CARTESIAN_POINT('Ctrl Pts',(2.50276671338074,1.,3.23089822320596));
#38254=CARTESIAN_POINT('Ctrl Pts',(2.5007958720187,-1.,3.22343262620387));
#38255=CARTESIAN_POINT('Ctrl Pts',(2.5007958720187,1.,3.22343262620387));
#38256=CARTESIAN_POINT('Ctrl Pts',(2.49879114599293,-1.,3.21598526261157));
#38257=CARTESIAN_POINT('Ctrl Pts',(2.49879114599293,1.,3.21598526261157));
#38258=CARTESIAN_POINT('Ctrl Pts',(2.49675252647298,-1.,3.2085566984974));
#38259=CARTESIAN_POINT('Ctrl Pts',(2.49675252647298,1.,3.2085566984974));
#38260=CARTESIAN_POINT('Ctrl Pts',(2.49467992057726,-1.,3.20114742397549));
#38261=CARTESIAN_POINT('Ctrl Pts',(2.49467992057726,1.,3.20114742397549));
#38262=CARTESIAN_POINT('Ctrl Pts',(2.4925730723986,-1.,3.19375775555814));
#38263=CARTESIAN_POINT('Ctrl Pts',(2.4925730723986,1.,3.19375775555814));
#38264=CARTESIAN_POINT('Ctrl Pts',(2.49043146334095,-1.,3.18638771282315));
#38265=CARTESIAN_POINT('Ctrl Pts',(2.49043146334095,1.,3.18638771282315));
#38266=CARTESIAN_POINT('Ctrl Pts',(2.48825428288242,-1.,3.17903698136679));
#38267=CARTESIAN_POINT('Ctrl Pts',(2.48825428288242,1.,3.17903698136679));
#38268=CARTESIAN_POINT('Ctrl Pts',(2.48604065348619,-1.,3.17170518863357));
#38269=CARTESIAN_POINT('Ctrl Pts',(2.48604065348619,1.,3.17170518863357));
#38270=CARTESIAN_POINT('Ctrl Pts',(2.48378981792739,-1.,3.16439213290181));
#38271=CARTESIAN_POINT('Ctrl Pts',(2.48378981792739,1.,3.16439213290181));
#38272=CARTESIAN_POINT('Ctrl Pts',(2.48150133566568,-1.,3.15709802322735));
#38273=CARTESIAN_POINT('Ctrl Pts',(2.48150133566568,1.,3.15709802322735));
#38274=CARTESIAN_POINT('Ctrl Pts',(2.47917529057016,-1.,3.14982373241335));
#38275=CARTESIAN_POINT('Ctrl Pts',(2.47917529057016,1.,3.14982373241335));
#38276=CARTESIAN_POINT('Ctrl Pts',(2.47681245356095,-1.,3.14257099546531));
#38277=CARTESIAN_POINT('Ctrl Pts',(2.47681245356095,1.,3.14257099546531));
#38278=CARTESIAN_POINT('Ctrl Pts',(2.47441378371923,-1.,3.13534181229282));
#38279=CARTESIAN_POINT('Ctrl Pts',(2.47441378371923,1.,3.13534181229282));
#38280=CARTESIAN_POINT('Ctrl Pts',(2.47197997765868,-1.,3.12813790805948));
#38281=CARTESIAN_POINT('Ctrl Pts',(2.47197997765868,1.,3.12813790805948));
#38282=CARTESIAN_POINT('Ctrl Pts',(2.4695109894747,-1.,3.12096015766984));
#38283=CARTESIAN_POINT('Ctrl Pts',(2.4695109894747,1.,3.12096015766984));
#38284=CARTESIAN_POINT('Ctrl Pts',(2.46700558843507,-1.,3.11380805536124));
#38285=CARTESIAN_POINT('Ctrl Pts',(2.46700558843507,1.,3.11380805536124));
#38286=CARTESIAN_POINT('Ctrl Pts',(2.46446082979645,-1.,3.10667907901981));
#38287=CARTESIAN_POINT('Ctrl Pts',(2.46446082979645,1.,3.10667907901981));
#38288=CARTESIAN_POINT('Ctrl Pts',(2.4618730850188,-1.,3.09956993697048));
#38289=CARTESIAN_POINT('Ctrl Pts',(2.4618730850188,1.,3.09956993697048));
#38290=CARTESIAN_POINT('Ctrl Pts',(2.45923912563875,-1.,3.09247787931881));
#38291=CARTESIAN_POINT('Ctrl Pts',(2.45923912563875,1.,3.09247787931881));
#38292=CARTESIAN_POINT('Ctrl Pts',(2.45655725437037,-1.,3.08540206545313));
#38293=CARTESIAN_POINT('Ctrl Pts',(2.45655725437037,1.,3.08540206545313));
#38294=CARTESIAN_POINT('Ctrl Pts',(2.45382826787795,-1.,3.07834472886145));
#38295=CARTESIAN_POINT('Ctrl Pts',(2.45382826787795,1.,3.07834472886145));
#38296=CARTESIAN_POINT('Ctrl Pts',(2.45105688854432,-1.,3.0713129052131));
#38297=CARTESIAN_POINT('Ctrl Pts',(2.45105688854432,1.,3.0713129052131));
#38298=CARTESIAN_POINT('Ctrl Pts',(2.44824970516557,-1.,3.06431596421422));
#38299=CARTESIAN_POINT('Ctrl Pts',(2.44824970516557,1.,3.06431596421422));
#38300=CARTESIAN_POINT('Ctrl Pts',(2.44541251892568,-1.,3.05736242671521));
#38301=CARTESIAN_POINT('Ctrl Pts',(2.44541251892568,1.,3.05736242671521));
#38302=CARTESIAN_POINT('Ctrl Pts',(2.44254768923109,-1.,3.05045678021509));
#38303=CARTESIAN_POINT('Ctrl Pts',(2.44254768923109,1.,3.05045678021509));
#38304=CARTESIAN_POINT('Ctrl Pts',(2.43965194061849,-1.,3.04359685040545));
#38305=CARTESIAN_POINT('Ctrl Pts',(2.43965194061849,1.,3.04359685040545));
#38306=CARTESIAN_POINT('Ctrl Pts',(2.43671278042394,-1.,3.03676949672797));
#38307=CARTESIAN_POINT('Ctrl Pts',(2.43671278042394,1.,3.03676949672797));
#38308=CARTESIAN_POINT('Ctrl Pts',(2.43371241361462,-1.,3.02995534946946));
#38309=CARTESIAN_POINT('Ctrl Pts',(2.43371241361462,1.,3.02995534946946));
#38310=CARTESIAN_POINT('Ctrl Pts',(2.43063415586615,-1.,3.02313656035977));
#38311=CARTESIAN_POINT('Ctrl Pts',(2.43063415586615,1.,3.02313656035977));
#38312=CARTESIAN_POINT('Ctrl Pts',(2.4274685626416,-1.,3.01630420830494));
#38313=CARTESIAN_POINT('Ctrl Pts',(2.4274685626416,1.,3.01630420830494));
#38314=CARTESIAN_POINT('Ctrl Pts',(2.42421849439625,-1.,3.00946442616674));
#38315=CARTESIAN_POINT('Ctrl Pts',(2.42421849439625,1.,3.00946442616674));
#38316=CARTESIAN_POINT('Ctrl Pts',(2.42090763946812,-1.,3.00264868586038));
#38317=CARTESIAN_POINT('Ctrl Pts',(2.42090763946812,1.,3.00264868586038));
#38318=CARTESIAN_POINT('Ctrl Pts',(2.4175732450056,-1.,2.99590509293561));
#38319=CARTESIAN_POINT('Ctrl Pts',(2.4175732450056,1.,2.99590509293561));
#38320=CARTESIAN_POINT('Ctrl Pts',(2.4142506419963,-1.,2.98927983005851));
#38321=CARTESIAN_POINT('Ctrl Pts',(2.4142506419963,1.,2.98927983005851));
#38322=CARTESIAN_POINT('Ctrl Pts',(2.41095909342591,-1.,2.98280015815132));
#38323=CARTESIAN_POINT('Ctrl Pts',(2.41095909342591,1.,2.98280015815132));
#38324=CARTESIAN_POINT('Ctrl Pts',(2.40768975073691,-1.,2.97646002822395));
#38325=CARTESIAN_POINT('Ctrl Pts',(2.40768975073691,1.,2.97646002822395));
#38326=CARTESIAN_POINT('Ctrl Pts',(2.40438604734848,-1.,2.97019641312272));
#38327=CARTESIAN_POINT('Ctrl Pts',(2.40438604734848,1.,2.97019641312272));
#38328=CARTESIAN_POINT('Ctrl Pts',(2.40095565711535,-1.,2.96390432240181));
#38329=CARTESIAN_POINT('Ctrl Pts',(2.40095565711535,1.,2.96390432240181));
#38330=CARTESIAN_POINT('Ctrl Pts',(2.39730553974412,-1.,2.95748006482811));
#38331=CARTESIAN_POINT('Ctrl Pts',(2.39730553974412,1.,2.95748006482811));
#38332=CARTESIAN_POINT('Ctrl Pts',(2.39337207631613,-1.,2.95085857128372));
#38333=CARTESIAN_POINT('Ctrl Pts',(2.39337207631613,1.,2.95085857128372));
#38334=CARTESIAN_POINT('Ctrl Pts',(2.38914929090806,-1.,2.94404820669135));
#38335=CARTESIAN_POINT('Ctrl Pts',(2.38914929090806,1.,2.94404820669135));
#38336=CARTESIAN_POINT('Ctrl Pts',(2.38472771516476,-1.,2.93717903280599));
#38337=CARTESIAN_POINT('Ctrl Pts',(2.38472771516476,1.,2.93717903280599));
#38338=CARTESIAN_POINT('Ctrl Pts',(2.3802898958232,-1.,2.93049643640517));
#38339=CARTESIAN_POINT('Ctrl Pts',(2.3802898958232,1.,2.93049643640517));
#38340=CARTESIAN_POINT('Ctrl Pts',(2.37606510524271,-1.,2.92430340582912));
#38341=CARTESIAN_POINT('Ctrl Pts',(2.37606510524271,1.,2.92430340582912));
#38342=CARTESIAN_POINT('Ctrl Pts',(2.37229381109939,-1.,2.9189150379156));
#38343=CARTESIAN_POINT('Ctrl Pts',(2.37229381109939,1.,2.9189150379156));
#38344=CARTESIAN_POINT('Ctrl Pts',(2.36919161373074,-1.,2.91461249883016));
#38345=CARTESIAN_POINT('Ctrl Pts',(2.36919161373074,1.,2.91461249883016));
#38346=CARTESIAN_POINT('Ctrl Pts',(2.36690501170317,-1.,2.9115863784165));
#38347=CARTESIAN_POINT('Ctrl Pts',(2.36690501170317,1.,2.9115863784165));
#38348=CARTESIAN_POINT('Ctrl Pts',(2.36578327194396,-1.,2.91025813829606));
#38349=CARTESIAN_POINT('Ctrl Pts',(2.36578327194396,1.,2.91025813829606));
#38350=CARTESIAN_POINT('Ctrl Pts',(2.36535052956704,-1.,2.90989022547738));
#38351=CARTESIAN_POINT('Ctrl Pts',(2.36535052956704,1.,2.90989022547738));
#38352=CARTESIAN_POINT('Ctrl Pts',(2.36524348105023,-1.,2.90992398626098));
#38353=CARTESIAN_POINT('Ctrl Pts',(2.36524348105023,1.,2.90992398626098));
#38354=CARTESIAN_POINT('Ctrl Pts',(2.36523532225181,-1.,2.91001063062876));
#38355=CARTESIAN_POINT('Ctrl Pts',(2.36523532225181,1.,2.91001063062876));
#38356=CARTESIAN_POINT('',(2.52982887637028,1.,3.35260583073571));
#38357=CARTESIAN_POINT('Ctrl Pts',(2.52982887637028,1.,3.35260583073571));
#38358=CARTESIAN_POINT('Ctrl Pts',(2.52954136549357,1.,3.35105973714426));
#38359=CARTESIAN_POINT('Ctrl Pts',(2.5289632161143,1.,3.34796903577628));
#38360=CARTESIAN_POINT('Ctrl Pts',(2.52808660916879,1.,3.34333744117093));
#38361=CARTESIAN_POINT('Ctrl Pts',(2.52689902691551,1.,3.33717090000955));
#38362=CARTESIAN_POINT('Ctrl Pts',(2.52538321165774,1.,3.32947762189049));
#38363=CARTESIAN_POINT('Ctrl Pts',(2.52383598396878,1.,3.32179931079521));
#38364=CARTESIAN_POINT('Ctrl Pts',(2.52225724871375,1.,3.31413607874727));
#38365=CARTESIAN_POINT('Ctrl Pts',(2.52064689568167,1.,3.30648808814986));
#38366=CARTESIAN_POINT('Ctrl Pts',(2.51900480700548,1.,3.29885556387661));
#38367=CARTESIAN_POINT('Ctrl Pts',(2.51733085123316,1.,3.2912387729863));
#38368=CARTESIAN_POINT('Ctrl Pts',(2.51562487464214,1.,3.28363799702583));
#38369=CARTESIAN_POINT('Ctrl Pts',(2.51388669270329,1.,3.27605350473048));
#38370=CARTESIAN_POINT('Ctrl Pts',(2.51211608411539,1.,3.26848552888271));
#38371=CARTESIAN_POINT('Ctrl Pts',(2.51031277813697,1.,3.26093423001716));
#38372=CARTESIAN_POINT('Ctrl Pts',(2.50847647070936,1.,3.25339971461265));
#38373=CARTESIAN_POINT('Ctrl Pts',(2.50660685940645,1.,3.24588208984042));
#38374=CARTESIAN_POINT('Ctrl Pts',(2.50470367580078,1.,3.23838151080383));
#38375=CARTESIAN_POINT('Ctrl Pts',(2.50276671338074,1.,3.23089822320596));
#38376=CARTESIAN_POINT('Ctrl Pts',(2.5007958720187,1.,3.22343262620387));
#38377=CARTESIAN_POINT('Ctrl Pts',(2.49879114599293,1.,3.21598526261157));
#38378=CARTESIAN_POINT('Ctrl Pts',(2.49675252647298,1.,3.2085566984974));
#38379=CARTESIAN_POINT('Ctrl Pts',(2.49467992057726,1.,3.20114742397549));
#38380=CARTESIAN_POINT('Ctrl Pts',(2.4925730723986,1.,3.19375775555814));
#38381=CARTESIAN_POINT('Ctrl Pts',(2.49043146334095,1.,3.18638771282315));
#38382=CARTESIAN_POINT('Ctrl Pts',(2.48825428288242,1.,3.17903698136679));
#38383=CARTESIAN_POINT('Ctrl Pts',(2.48604065348619,1.,3.17170518863357));
#38384=CARTESIAN_POINT('Ctrl Pts',(2.48378981792739,1.,3.16439213290181));
#38385=CARTESIAN_POINT('Ctrl Pts',(2.48150133566568,1.,3.15709802322735));
#38386=CARTESIAN_POINT('Ctrl Pts',(2.47917529057016,1.,3.14982373241335));
#38387=CARTESIAN_POINT('Ctrl Pts',(2.47681245356095,1.,3.14257099546531));
#38388=CARTESIAN_POINT('Ctrl Pts',(2.47441378371923,1.,3.13534181229282));
#38389=CARTESIAN_POINT('Ctrl Pts',(2.47197997765868,1.,3.12813790805948));
#38390=CARTESIAN_POINT('Ctrl Pts',(2.4695109894747,1.,3.12096015766984));
#38391=CARTESIAN_POINT('Ctrl Pts',(2.46700558843507,1.,3.11380805536124));
#38392=CARTESIAN_POINT('Ctrl Pts',(2.46446082979645,1.,3.10667907901981));
#38393=CARTESIAN_POINT('Ctrl Pts',(2.4618730850188,1.,3.09956993697048));
#38394=CARTESIAN_POINT('Ctrl Pts',(2.45923912563875,1.,3.09247787931881));
#38395=CARTESIAN_POINT('Ctrl Pts',(2.45655725437037,1.,3.08540206545313));
#38396=CARTESIAN_POINT('Ctrl Pts',(2.45382826787795,1.,3.07834472886145));
#38397=CARTESIAN_POINT('Ctrl Pts',(2.45105688854432,1.,3.0713129052131));
#38398=CARTESIAN_POINT('Ctrl Pts',(2.44824970516557,1.,3.06431596421422));
#38399=CARTESIAN_POINT('Ctrl Pts',(2.44541251892568,1.,3.05736242671521));
#38400=CARTESIAN_POINT('Ctrl Pts',(2.44254768923109,1.,3.05045678021509));
#38401=CARTESIAN_POINT('Ctrl Pts',(2.43965194061849,1.,3.04359685040545));
#38402=CARTESIAN_POINT('Ctrl Pts',(2.43671278042394,1.,3.03676949672797));
#38403=CARTESIAN_POINT('Ctrl Pts',(2.43371241361462,1.,3.02995534946946));
#38404=CARTESIAN_POINT('Ctrl Pts',(2.43063415586615,1.,3.02313656035977));
#38405=CARTESIAN_POINT('Ctrl Pts',(2.4274685626416,1.,3.01630420830494));
#38406=CARTESIAN_POINT('Ctrl Pts',(2.42421849439625,1.,3.00946442616674));
#38407=CARTESIAN_POINT('Ctrl Pts',(2.42090763946812,1.,3.00264868586038));
#38408=CARTESIAN_POINT('Ctrl Pts',(2.4175732450056,1.,2.99590509293561));
#38409=CARTESIAN_POINT('Ctrl Pts',(2.4142506419963,1.,2.98927983005851));
#38410=CARTESIAN_POINT('Ctrl Pts',(2.41095909342591,1.,2.98280015815132));
#38411=CARTESIAN_POINT('Ctrl Pts',(2.40768975073691,1.,2.97646002822395));
#38412=CARTESIAN_POINT('Ctrl Pts',(2.40438604734848,1.,2.97019641312272));
#38413=CARTESIAN_POINT('Ctrl Pts',(2.40095565711535,1.,2.96390432240181));
#38414=CARTESIAN_POINT('Ctrl Pts',(2.39730553974412,1.,2.95748006482811));
#38415=CARTESIAN_POINT('Ctrl Pts',(2.39337207631613,1.,2.95085857128372));
#38416=CARTESIAN_POINT('Ctrl Pts',(2.38914929090806,1.,2.94404820669135));
#38417=CARTESIAN_POINT('Ctrl Pts',(2.38472771516476,1.,2.93717903280599));
#38418=CARTESIAN_POINT('Ctrl Pts',(2.3802898958232,1.,2.93049643640517));
#38419=CARTESIAN_POINT('Ctrl Pts',(2.37606510524271,1.,2.92430340582912));
#38420=CARTESIAN_POINT('Ctrl Pts',(2.37229381109939,1.,2.9189150379156));
#38421=CARTESIAN_POINT('Ctrl Pts',(2.36919161373074,1.,2.91461249883016));
#38422=CARTESIAN_POINT('Ctrl Pts',(2.36707658451709,1.,2.91181344022628));
#38423=CARTESIAN_POINT('Ctrl Pts',(2.36599991765853,1.,2.91051690822262));
#38424=CARTESIAN_POINT('Ctrl Pts',(2.36553202948741,1.,2.91005770527771));
#38425=CARTESIAN_POINT('Ctrl Pts',(2.3653621118858,1.,2.90995756655559));
#38426=CARTESIAN_POINT('Ctrl Pts',(2.36531447826213,1.,2.90994629141563));
#38427=CARTESIAN_POINT('',(2.52982887637028,0.,3.35260583073571));
#38428=CARTESIAN_POINT('Ctrl Pts',(2.03668666247593,-1.,3.1487152044751));
#38429=CARTESIAN_POINT('Ctrl Pts',(2.03668666247593,1.,3.1487152044751));
#38430=CARTESIAN_POINT('Ctrl Pts',(2.03660173757879,-1.,3.14869618937258));
#38431=CARTESIAN_POINT('Ctrl Pts',(2.03660173757879,1.,3.14869618937258));
#38432=CARTESIAN_POINT('Ctrl Pts',(2.03653654935591,-1.,3.14878756590812));
#38433=CARTESIAN_POINT('Ctrl Pts',(2.03653654935591,1.,3.14878756590812));
#38434=CARTESIAN_POINT('Ctrl Pts',(2.03675273049189,-1.,3.14931281968048));
#38435=CARTESIAN_POINT('Ctrl Pts',(2.03675273049189,1.,3.14931281968048));
#38436=CARTESIAN_POINT('Ctrl Pts',(2.03766932526445,-1.,3.15079010635742));
#38437=CARTESIAN_POINT('Ctrl Pts',(2.03766932526445,1.,3.15079010635742));
#38438=CARTESIAN_POINT('Ctrl Pts',(2.03984073791519,-1.,3.15389991674792));
#38439=CARTESIAN_POINT('Ctrl Pts',(2.03984073791519,1.,3.15389991674792));
#38440=CARTESIAN_POINT('Ctrl Pts',(2.04297406404027,-1.,3.15817983946367));
#38441=CARTESIAN_POINT('Ctrl Pts',(2.04297406404027,1.,3.15817983946367));
#38442=CARTESIAN_POINT('Ctrl Pts',(2.04693331247446,-1.,3.16343165058912));
#38443=CARTESIAN_POINT('Ctrl Pts',(2.04693331247446,1.,3.16343165058912));
#38444=CARTESIAN_POINT('Ctrl Pts',(2.05151770247233,-1.,3.16936341689527));
#38445=CARTESIAN_POINT('Ctrl Pts',(2.05151770247233,1.,3.16936341689527));
#38446=CARTESIAN_POINT('Ctrl Pts',(2.05650186773132,-1.,3.17564906975371));
#38447=CARTESIAN_POINT('Ctrl Pts',(2.05650186773132,1.,3.17564906975371));
#38448=CARTESIAN_POINT('Ctrl Pts',(2.06166849827101,-1.,3.18197692964614));
#38449=CARTESIAN_POINT('Ctrl Pts',(2.06166849827101,1.,3.18197692964614));
#38450=CARTESIAN_POINT('Ctrl Pts',(2.06684062744112,-1.,3.18809755562368));
#38451=CARTESIAN_POINT('Ctrl Pts',(2.06684062744112,1.,3.18809755562368));
#38452=CARTESIAN_POINT('Ctrl Pts',(2.07192253497857,-1.,3.19388465568252));
#38453=CARTESIAN_POINT('Ctrl Pts',(2.07192253497857,1.,3.19388465568252));
#38454=CARTESIAN_POINT('Ctrl Pts',(2.07690441870722,-1.,3.19934132836019));
#38455=CARTESIAN_POINT('Ctrl Pts',(2.07690441870722,1.,3.19934132836019));
#38456=CARTESIAN_POINT('Ctrl Pts',(2.08182850370878,-1.,3.2045481863073));
#38457=CARTESIAN_POINT('Ctrl Pts',(2.08182850370878,1.,3.2045481863073));
#38458=CARTESIAN_POINT('Ctrl Pts',(2.08676465517455,-1.,3.20962575845463));
#38459=CARTESIAN_POINT('Ctrl Pts',(2.08676465517455,1.,3.20962575845463));
#38460=CARTESIAN_POINT('Ctrl Pts',(2.09178419460443,-1.,3.21469429601654));
#38461=CARTESIAN_POINT('Ctrl Pts',(2.09178419460443,1.,3.21469429601654));
#38462=CARTESIAN_POINT('Ctrl Pts',(2.09692958434895,-1.,3.21982707347009));
#38463=CARTESIAN_POINT('Ctrl Pts',(2.09692958434895,1.,3.21982707347009));
#38464=CARTESIAN_POINT('Ctrl Pts',(2.10220384298492,-1.,3.22503437553434));
#38465=CARTESIAN_POINT('Ctrl Pts',(2.10220384298492,1.,3.22503437553434));
#38466=CARTESIAN_POINT('Ctrl Pts',(2.10758699642451,-1.,3.23028945793289));
#38467=CARTESIAN_POINT('Ctrl Pts',(2.10758699642451,1.,3.23028945793289));
#38468=CARTESIAN_POINT('Ctrl Pts',(2.11304604021773,-1.,3.23554444767099));
#38469=CARTESIAN_POINT('Ctrl Pts',(2.11304604021773,1.,3.23554444767099));
#38470=CARTESIAN_POINT('Ctrl Pts',(2.11854673326979,-1.,3.24074905517293));
#38471=CARTESIAN_POINT('Ctrl Pts',(2.11854673326979,1.,3.24074905517293));
#38472=CARTESIAN_POINT('Ctrl Pts',(2.12406646410962,-1.,3.24587102613376));
#38473=CARTESIAN_POINT('Ctrl Pts',(2.12406646410962,1.,3.24587102613376));
#38474=CARTESIAN_POINT('Ctrl Pts',(2.12960028396832,-1.,3.25090574494028));
#38475=CARTESIAN_POINT('Ctrl Pts',(2.12960028396832,1.,3.25090574494028));
#38476=CARTESIAN_POINT('Ctrl Pts',(2.13515375878803,-1.,3.25586495065054));
#38477=CARTESIAN_POINT('Ctrl Pts',(2.13515375878803,1.,3.25586495065054));
#38478=CARTESIAN_POINT('Ctrl Pts',(2.14073870754264,-1.,3.26077002641879));
#38479=CARTESIAN_POINT('Ctrl Pts',(2.14073870754264,1.,3.26077002641879));
#38480=CARTESIAN_POINT('Ctrl Pts',(2.1463680529566,-1.,3.26564388189759));
#38481=CARTESIAN_POINT('Ctrl Pts',(2.1463680529566,1.,3.26564388189759));
#38482=CARTESIAN_POINT('Ctrl Pts',(2.15205043199808,-1.,3.27050245897228));
#38483=CARTESIAN_POINT('Ctrl Pts',(2.15205043199808,1.,3.27050245897228));
#38484=CARTESIAN_POINT('Ctrl Pts',(2.15778690038347,-1.,3.27534954469187));
#38485=CARTESIAN_POINT('Ctrl Pts',(2.15778690038347,1.,3.27534954469187));
#38486=CARTESIAN_POINT('Ctrl Pts',(2.16357391934425,-1.,3.280181508414));
#38487=CARTESIAN_POINT('Ctrl Pts',(2.16357391934425,1.,3.280181508414));
#38488=CARTESIAN_POINT('Ctrl Pts',(2.16940517773455,-1.,3.28499019979724));
#38489=CARTESIAN_POINT('Ctrl Pts',(2.16940517773455,1.,3.28499019979724));
#38490=CARTESIAN_POINT('Ctrl Pts',(2.17527380048423,-1.,3.28976645712568));
#38491=CARTESIAN_POINT('Ctrl Pts',(2.17527380048423,1.,3.28976645712568));
#38492=CARTESIAN_POINT('Ctrl Pts',(2.18117455557065,-1.,3.2945036150049));
#38493=CARTESIAN_POINT('Ctrl Pts',(2.18117455557065,1.,3.2945036150049));
#38494=CARTESIAN_POINT('Ctrl Pts',(2.18710556500327,-1.,3.29920022557639));
#38495=CARTESIAN_POINT('Ctrl Pts',(2.18710556500327,1.,3.29920022557639));
#38496=CARTESIAN_POINT('Ctrl Pts',(2.19306710376111,-1.,3.30385816281831));
#38497=CARTESIAN_POINT('Ctrl Pts',(2.19306710376111,1.,3.30385816281831));
#38498=CARTESIAN_POINT('Ctrl Pts',(2.19906078949922,-1.,3.30848134694595));
#38499=CARTESIAN_POINT('Ctrl Pts',(2.19906078949922,1.,3.30848134694595));
#38500=CARTESIAN_POINT('Ctrl Pts',(2.20508863150607,-1.,3.31307424608949));
#38501=CARTESIAN_POINT('Ctrl Pts',(2.20508863150607,1.,3.31307424608949));
#38502=CARTESIAN_POINT('Ctrl Pts',(2.21115211847875,-1.,3.31764044024235));
#38503=CARTESIAN_POINT('Ctrl Pts',(2.21115211847875,1.,3.31764044024235));
#38504=CARTESIAN_POINT('Ctrl Pts',(2.21725135110898,-1.,3.32218125618968));
#38505=CARTESIAN_POINT('Ctrl Pts',(2.21725135110898,1.,3.32218125618968));
#38506=CARTESIAN_POINT('Ctrl Pts',(2.22338548312772,-1.,3.3266964672289));
#38507=CARTESIAN_POINT('Ctrl Pts',(2.22338548312772,1.,3.3266964672289));
#38508=CARTESIAN_POINT('Ctrl Pts',(2.22955308907233,-1.,3.33118487773611));
#38509=CARTESIAN_POINT('Ctrl Pts',(2.22955308907233,1.,3.33118487773611));
#38510=CARTESIAN_POINT('Ctrl Pts',(2.23575256328812,-1.,3.33564495756482));
#38511=CARTESIAN_POINT('Ctrl Pts',(2.23575256328812,1.,3.33564495756482));
#38512=CARTESIAN_POINT('Ctrl Pts',(2.24198249391422,-1.,3.34007543738025));
#38513=CARTESIAN_POINT('Ctrl Pts',(2.24198249391422,1.,3.34007543738025));
#38514=CARTESIAN_POINT('Ctrl Pts',(2.24824207678256,-1.,3.34447596770723));
#38515=CARTESIAN_POINT('Ctrl Pts',(2.24824207678256,1.,3.34447596770723));
#38516=CARTESIAN_POINT('Ctrl Pts',(2.25453097693483,-1.,3.34884690292285));
#38517=CARTESIAN_POINT('Ctrl Pts',(2.25453097693483,1.,3.34884690292285));
#38518=CARTESIAN_POINT('Ctrl Pts',(2.26084915222449,-1.,3.35318902552626));
#38519=CARTESIAN_POINT('Ctrl Pts',(2.26084915222449,1.,3.35318902552626));
#38520=CARTESIAN_POINT('Ctrl Pts',(2.26719668579909,-1.,3.35750328523061));
#38521=CARTESIAN_POINT('Ctrl Pts',(2.26719668579909,1.,3.35750328523061));
#38522=CARTESIAN_POINT('Ctrl Pts',(2.2735736262093,-1.,3.36179055004409));
#38523=CARTESIAN_POINT('Ctrl Pts',(2.2735736262093,1.,3.36179055004409));
#38524=CARTESIAN_POINT('Ctrl Pts',(2.27997979458037,-1.,3.36605130713076));
#38525=CARTESIAN_POINT('Ctrl Pts',(2.27997979458037,1.,3.36605130713076));
#38526=CARTESIAN_POINT('Ctrl Pts',(2.28641481081137,-1.,3.37028570206488));
#38527=CARTESIAN_POINT('Ctrl Pts',(2.28641481081137,1.,3.37028570206488));
#38528=CARTESIAN_POINT('Ctrl Pts',(2.29287818007393,-1.,3.37449367172826));
#38529=CARTESIAN_POINT('Ctrl Pts',(2.29287818007393,1.,3.37449367172826));
#38530=CARTESIAN_POINT('Ctrl Pts',(2.29936936127624,-1.,3.37867504959433));
#38531=CARTESIAN_POINT('Ctrl Pts',(2.29936936127624,1.,3.37867504959433));
#38532=CARTESIAN_POINT('Ctrl Pts',(2.30588783640343,-1.,3.3828296733661));
#38533=CARTESIAN_POINT('Ctrl Pts',(2.30588783640343,1.,3.3828296733661));
#38534=CARTESIAN_POINT('Ctrl Pts',(2.31243319489367,-1.,3.38695751492462));
#38535=CARTESIAN_POINT('Ctrl Pts',(2.31243319489367,1.,3.38695751492462));
#38536=CARTESIAN_POINT('Ctrl Pts',(2.31900513925424,-1.,3.39105869474822));
#38537=CARTESIAN_POINT('Ctrl Pts',(2.31900513925424,1.,3.39105869474822));
#38538=CARTESIAN_POINT('Ctrl Pts',(2.3256034390248,-1.,3.39513342019756));
#38539=CARTESIAN_POINT('Ctrl Pts',(2.3256034390248,1.,3.39513342019756));
#38540=CARTESIAN_POINT('Ctrl Pts',(2.33222789882489,-1.,3.39918194577956));
#38541=CARTESIAN_POINT('Ctrl Pts',(2.33222789882489,1.,3.39918194577956));
#38542=CARTESIAN_POINT('Ctrl Pts',(2.33887832342782,-1.,3.40320452776743));
#38543=CARTESIAN_POINT('Ctrl Pts',(2.33887832342782,1.,3.40320452776743));
#38544=CARTESIAN_POINT('Ctrl Pts',(2.34555447649188,-1.,3.40720137404297));
#38545=CARTESIAN_POINT('Ctrl Pts',(2.34555447649188,1.,3.40720137404297));
#38546=CARTESIAN_POINT('Ctrl Pts',(2.35225606824109,-1.,3.41117262314119));
#38547=CARTESIAN_POINT('Ctrl Pts',(2.35225606824109,1.,3.41117262314119));
#38548=CARTESIAN_POINT('Ctrl Pts',(2.35898278606946,-1.,3.41511836751469));
#38549=CARTESIAN_POINT('Ctrl Pts',(2.35898278606946,1.,3.41511836751469));
#38550=CARTESIAN_POINT('Ctrl Pts',(2.36573431470642,-1.,3.41903866635852));
#38551=CARTESIAN_POINT('Ctrl Pts',(2.36573431470642,1.,3.41903866635852));
#38552=CARTESIAN_POINT('Ctrl Pts',(2.37251035954292,-1.,3.42293356216511));
#38553=CARTESIAN_POINT('Ctrl Pts',(2.37251035954292,1.,3.42293356216511));
#38554=CARTESIAN_POINT('Ctrl Pts',(2.37931067028926,-1.,3.42680309754399));
#38555=CARTESIAN_POINT('Ctrl Pts',(2.37931067028926,1.,3.42680309754399));
#38556=CARTESIAN_POINT('Ctrl Pts',(2.38613505843552,-1.,3.4306473271292));
#38557=CARTESIAN_POINT('Ctrl Pts',(2.38613505843552,1.,3.4306473271292));
#38558=CARTESIAN_POINT('Ctrl Pts',(2.39298338804493,-1.,3.4344663067854));
#38559=CARTESIAN_POINT('Ctrl Pts',(2.39298338804493,1.,3.4344663067854));
#38560=CARTESIAN_POINT('Ctrl Pts',(2.39848113410292,-1.,3.43750133064416));
#38561=CARTESIAN_POINT('Ctrl Pts',(2.39848113410292,1.,3.43750133064416));
#38562=CARTESIAN_POINT('Ctrl Pts',(2.40261515589405,-1.,3.43976627484234));
#38563=CARTESIAN_POINT('Ctrl Pts',(2.40261515589405,1.,3.43976627484234));
#38564=CARTESIAN_POINT('Ctrl Pts',(2.4053759295909,-1.,3.44127120683039));
#38565=CARTESIAN_POINT('Ctrl Pts',(2.4053759295909,1.,3.44127120683039));
#38566=CARTESIAN_POINT('Ctrl Pts',(2.40675750623143,-1.,3.44202241512147));
#38567=CARTESIAN_POINT('Ctrl Pts',(2.40675750623143,1.,3.44202241512147));
#38568=CARTESIAN_POINT('',(2.03660101169714,1.,3.14877060440328));
#38569=CARTESIAN_POINT('Ctrl Pts',(2.03660101169714,-1.,3.14877060440327));
#38570=CARTESIAN_POINT('Ctrl Pts',(2.03660101169714,-0.666666666666667,
3.14877060440327));
#38571=CARTESIAN_POINT('Ctrl Pts',(2.03660101169714,-0.333333333333333,
3.14877060440327));
#38572=CARTESIAN_POINT('Ctrl Pts',(2.03660101169714,0.333333333333333,3.14877060440327));
#38573=CARTESIAN_POINT('Ctrl Pts',(2.03660101169714,0.666666666666667,3.14877060440327));
#38574=CARTESIAN_POINT('Ctrl Pts',(2.03660101169714,1.,3.14877060440327));
#38575=CARTESIAN_POINT('',(2.40675750623143,1.,3.44202241512147));
#38576=CARTESIAN_POINT('',(2.40675750623143,0.,3.44202241512147));
#38577=CARTESIAN_POINT('Ctrl Pts',(2.03660101169714,1.,3.14877060440328));
#38578=CARTESIAN_POINT('Ctrl Pts',(2.03659701539259,1.,3.14881939088124));
#38579=CARTESIAN_POINT('Ctrl Pts',(2.03663974554932,1.,3.1490119366901));
#38580=CARTESIAN_POINT('Ctrl Pts',(2.03693188810545,1.,3.14959882629805));
#38581=CARTESIAN_POINT('Ctrl Pts',(2.03783225495961,1.,3.15102344775328));
#38582=CARTESIAN_POINT('Ctrl Pts',(2.03984073791519,1.,3.15389991674792));
#38583=CARTESIAN_POINT('Ctrl Pts',(2.04297406404027,1.,3.15817983946367));
#38584=CARTESIAN_POINT('Ctrl Pts',(2.04693331247446,1.,3.16343165058912));
#38585=CARTESIAN_POINT('Ctrl Pts',(2.05151770247233,1.,3.16936341689527));
#38586=CARTESIAN_POINT('Ctrl Pts',(2.05650186773132,1.,3.17564906975371));
#38587=CARTESIAN_POINT('Ctrl Pts',(2.06166849827101,1.,3.18197692964614));
#38588=CARTESIAN_POINT('Ctrl Pts',(2.06684062744112,1.,3.18809755562368));
#38589=CARTESIAN_POINT('Ctrl Pts',(2.07192253497857,1.,3.19388465568252));
#38590=CARTESIAN_POINT('Ctrl Pts',(2.07690441870722,1.,3.19934132836019));
#38591=CARTESIAN_POINT('Ctrl Pts',(2.08182850370878,1.,3.2045481863073));
#38592=CARTESIAN_POINT('Ctrl Pts',(2.08676465517455,1.,3.20962575845463));
#38593=CARTESIAN_POINT('Ctrl Pts',(2.09178419460443,1.,3.21469429601654));
#38594=CARTESIAN_POINT('Ctrl Pts',(2.09692958434895,1.,3.21982707347009));
#38595=CARTESIAN_POINT('Ctrl Pts',(2.10220384298492,1.,3.22503437553434));
#38596=CARTESIAN_POINT('Ctrl Pts',(2.10758699642451,1.,3.23028945793289));
#38597=CARTESIAN_POINT('Ctrl Pts',(2.11304604021773,1.,3.23554444767099));
#38598=CARTESIAN_POINT('Ctrl Pts',(2.11854673326979,1.,3.24074905517293));
#38599=CARTESIAN_POINT('Ctrl Pts',(2.12406646410962,1.,3.24587102613376));
#38600=CARTESIAN_POINT('Ctrl Pts',(2.12960028396832,1.,3.25090574494028));
#38601=CARTESIAN_POINT('Ctrl Pts',(2.13515375878803,1.,3.25586495065054));
#38602=CARTESIAN_POINT('Ctrl Pts',(2.14073870754264,1.,3.26077002641879));
#38603=CARTESIAN_POINT('Ctrl Pts',(2.1463680529566,1.,3.26564388189759));
#38604=CARTESIAN_POINT('Ctrl Pts',(2.15205043199808,1.,3.27050245897228));
#38605=CARTESIAN_POINT('Ctrl Pts',(2.15778690038347,1.,3.27534954469187));
#38606=CARTESIAN_POINT('Ctrl Pts',(2.16357391934425,1.,3.280181508414));
#38607=CARTESIAN_POINT('Ctrl Pts',(2.16940517773455,1.,3.28499019979724));
#38608=CARTESIAN_POINT('Ctrl Pts',(2.17527380048423,1.,3.28976645712568));
#38609=CARTESIAN_POINT('Ctrl Pts',(2.18117455557065,1.,3.2945036150049));
#38610=CARTESIAN_POINT('Ctrl Pts',(2.18710556500327,1.,3.29920022557639));
#38611=CARTESIAN_POINT('Ctrl Pts',(2.19306710376111,1.,3.30385816281831));
#38612=CARTESIAN_POINT('Ctrl Pts',(2.19906078949922,1.,3.30848134694595));
#38613=CARTESIAN_POINT('Ctrl Pts',(2.20508863150607,1.,3.31307424608949));
#38614=CARTESIAN_POINT('Ctrl Pts',(2.21115211847875,1.,3.31764044024235));
#38615=CARTESIAN_POINT('Ctrl Pts',(2.21725135110898,1.,3.32218125618968));
#38616=CARTESIAN_POINT('Ctrl Pts',(2.22338548312772,1.,3.3266964672289));
#38617=CARTESIAN_POINT('Ctrl Pts',(2.22955308907233,1.,3.33118487773611));
#38618=CARTESIAN_POINT('Ctrl Pts',(2.23575256328812,1.,3.33564495756482));
#38619=CARTESIAN_POINT('Ctrl Pts',(2.24198249391422,1.,3.34007543738025));
#38620=CARTESIAN_POINT('Ctrl Pts',(2.24824207678256,1.,3.34447596770723));
#38621=CARTESIAN_POINT('Ctrl Pts',(2.25453097693483,1.,3.34884690292285));
#38622=CARTESIAN_POINT('Ctrl Pts',(2.26084915222449,1.,3.35318902552626));
#38623=CARTESIAN_POINT('Ctrl Pts',(2.26719668579909,1.,3.35750328523061));
#38624=CARTESIAN_POINT('Ctrl Pts',(2.2735736262093,1.,3.36179055004409));
#38625=CARTESIAN_POINT('Ctrl Pts',(2.27997979458037,1.,3.36605130713076));
#38626=CARTESIAN_POINT('Ctrl Pts',(2.28641481081137,1.,3.37028570206488));
#38627=CARTESIAN_POINT('Ctrl Pts',(2.29287818007393,1.,3.37449367172826));
#38628=CARTESIAN_POINT('Ctrl Pts',(2.29936936127624,1.,3.37867504959433));
#38629=CARTESIAN_POINT('Ctrl Pts',(2.30588783640343,1.,3.3828296733661));
#38630=CARTESIAN_POINT('Ctrl Pts',(2.31243319489367,1.,3.38695751492462));
#38631=CARTESIAN_POINT('Ctrl Pts',(2.31900513925424,1.,3.39105869474822));
#38632=CARTESIAN_POINT('Ctrl Pts',(2.3256034390248,1.,3.39513342019756));
#38633=CARTESIAN_POINT('Ctrl Pts',(2.33222789882489,1.,3.39918194577956));
#38634=CARTESIAN_POINT('Ctrl Pts',(2.33887832342782,1.,3.40320452776743));
#38635=CARTESIAN_POINT('Ctrl Pts',(2.34555447649188,1.,3.40720137404297));
#38636=CARTESIAN_POINT('Ctrl Pts',(2.35225606824109,1.,3.41117262314119));
#38637=CARTESIAN_POINT('Ctrl Pts',(2.35898278606946,1.,3.41511836751469));
#38638=CARTESIAN_POINT('Ctrl Pts',(2.36573431470642,1.,3.41903866635852));
#38639=CARTESIAN_POINT('Ctrl Pts',(2.37251035954292,1.,3.42293356216511));
#38640=CARTESIAN_POINT('Ctrl Pts',(2.37931067028926,1.,3.42680309754399));
#38641=CARTESIAN_POINT('Ctrl Pts',(2.38613505843552,1.,3.4306473271292));
#38642=CARTESIAN_POINT('Ctrl Pts',(2.39298338804493,1.,3.4344663067854));
#38643=CARTESIAN_POINT('Ctrl Pts',(2.39848113410292,1.,3.43750133064416));
#38644=CARTESIAN_POINT('Ctrl Pts',(2.40261515589405,1.,3.43976627484234));
#38645=CARTESIAN_POINT('Ctrl Pts',(2.4053759295909,1.,3.44127120683039));
#38646=CARTESIAN_POINT('Ctrl Pts',(2.40675750623143,1.,3.44202241512147));
#38647=CARTESIAN_POINT('Origin',(2.40675750623143,0.,3.44202241512147));
#38648=CARTESIAN_POINT('',(2.52982887637028,1.,3.35260583073571));
#38649=CARTESIAN_POINT('Origin',(0.,0.,0.));
#38650=CARTESIAN_POINT('',(1.88097764062697,1.,3.24413672884812));
#38651=CARTESIAN_POINT('Origin',(0.,1.,0.));
#38652=CARTESIAN_POINT('Ctrl Pts',(1.88097764062697,1.,3.24413672884812));
#38653=CARTESIAN_POINT('Ctrl Pts',(1.88097764062697,0.666666666666667,3.24413672884812));
#38654=CARTESIAN_POINT('Ctrl Pts',(1.88097764062697,0.333333333333333,3.24413672884812));
#38655=CARTESIAN_POINT('Ctrl Pts',(1.88097764062697,-0.333333333333333,
3.24413672884812));
#38656=CARTESIAN_POINT('Ctrl Pts',(1.88097764062697,-0.666666666666667,
3.24413672884812));
#38657=CARTESIAN_POINT('Ctrl Pts',(1.88097764062697,-1.,3.24413672884812));
#38658=CARTESIAN_POINT('Ctrl Pts',(1.97421938526992,-1.,3.70708211654725));
#38659=CARTESIAN_POINT('Ctrl Pts',(1.97421938526992,1.,3.70708211654725));
#38660=CARTESIAN_POINT('Ctrl Pts',(1.97417727645308,-1.,3.70551008132332));
#38661=CARTESIAN_POINT('Ctrl Pts',(1.97417727645308,1.,3.70551008132332));
#38662=CARTESIAN_POINT('Ctrl Pts',(1.97408973726715,-1.,3.70236698912904));
#38663=CARTESIAN_POINT('Ctrl Pts',(1.97408973726715,1.,3.70236698912904));
#38664=CARTESIAN_POINT('Ctrl Pts',(1.97394846383216,-1.,3.6976552856004));
#38665=CARTESIAN_POINT('Ctrl Pts',(1.97394846383216,1.,3.6976552856004));
#38666=CARTESIAN_POINT('Ctrl Pts',(1.97374016225483,-1.,3.69137888599902));
#38667=CARTESIAN_POINT('Ctrl Pts',(1.97374016225483,1.,3.69137888599902));
#38668=CARTESIAN_POINT('Ctrl Pts',(1.97344650304519,-1.,3.68354319915092));
#38669=CARTESIAN_POINT('Ctrl Pts',(1.97344650304519,1.,3.68354319915092));
#38670=CARTESIAN_POINT('Ctrl Pts',(1.97311947678516,-1.,3.67571738107084));
#38671=CARTESIAN_POINT('Ctrl Pts',(1.97311947678516,1.,3.67571738107084));
#38672=CARTESIAN_POINT('Ctrl Pts',(1.97275897198678,-1.,3.66790152752075));
#38673=CARTESIAN_POINT('Ctrl Pts',(1.97275897198678,1.,3.66790152752075));
#38674=CARTESIAN_POINT('Ctrl Pts',(1.9723648543905,-1.,3.6600957816636));
#38675=CARTESIAN_POINT('Ctrl Pts',(1.9723648543905,1.,3.6600957816636));
#38676=CARTESIAN_POINT('Ctrl Pts',(1.97193697240239,-1.,3.652300347166));
#38677=CARTESIAN_POINT('Ctrl Pts',(1.97193697240239,1.,3.652300347166));
#38678=CARTESIAN_POINT('Ctrl Pts',(1.97147515441164,-1.,3.64451546723514));
#38679=CARTESIAN_POINT('Ctrl Pts',(1.97147515441164,1.,3.64451546723514));
#38680=CARTESIAN_POINT('Ctrl Pts',(1.97097920454464,-1.,3.63674139590412));
#38681=CARTESIAN_POINT('Ctrl Pts',(1.97097920454464,1.,3.63674139590412));
#38682=CARTESIAN_POINT('Ctrl Pts',(1.97044889850463,-1.,3.62897836973293));
#38683=CARTESIAN_POINT('Ctrl Pts',(1.97044889850463,1.,3.62897836973293));
#38684=CARTESIAN_POINT('Ctrl Pts',(1.96988398129978,-1.,3.62122658401893));
#38685=CARTESIAN_POINT('Ctrl Pts',(1.96988398129978,1.,3.62122658401893));
#38686=CARTESIAN_POINT('Ctrl Pts',(1.96928416040877,-1.,3.61348615496704));
#38687=CARTESIAN_POINT('Ctrl Pts',(1.96928416040877,1.,3.61348615496704));
#38688=CARTESIAN_POINT('Ctrl Pts',(1.9686491188594,-1.,3.60575714017989));
#38689=CARTESIAN_POINT('Ctrl Pts',(1.9686491188594,1.,3.60575714017989));
#38690=CARTESIAN_POINT('Ctrl Pts',(1.96797854118369,-1.,3.59803959819938));
#38691=CARTESIAN_POINT('Ctrl Pts',(1.96797854118369,1.,3.59803959819938));
#38692=CARTESIAN_POINT('Ctrl Pts',(1.96727213799544,-1.,3.59033364022801));
#38693=CARTESIAN_POINT('Ctrl Pts',(1.96727213799544,1.,3.59033364022801));
#38694=CARTESIAN_POINT('Ctrl Pts',(1.96652966688911,-1.,3.58263947663829));
#38695=CARTESIAN_POINT('Ctrl Pts',(1.96652966688911,1.,3.58263947663829));
#38696=CARTESIAN_POINT('Ctrl Pts',(1.96575096652789,-1.,3.57495748600959));
#38697=CARTESIAN_POINT('Ctrl Pts',(1.96575096652789,1.,3.57495748600959));
#38698=CARTESIAN_POINT('Ctrl Pts',(1.96493594634567,-1.,3.56728820357791));
#38699=CARTESIAN_POINT('Ctrl Pts',(1.96493594634567,1.,3.56728820357791));
#38700=CARTESIAN_POINT('Ctrl Pts',(1.96408450906812,-1.,3.55963218706096));
#38701=CARTESIAN_POINT('Ctrl Pts',(1.96408450906812,1.,3.55963218706096));
#38702=CARTESIAN_POINT('Ctrl Pts',(1.96319648628644,-1.,3.55198990600886));
#38703=CARTESIAN_POINT('Ctrl Pts',(1.96319648628644,1.,3.55198990600886));
#38704=CARTESIAN_POINT('Ctrl Pts',(1.96227157573067,-1.,3.54436163300443));
#38705=CARTESIAN_POINT('Ctrl Pts',(1.96227157573067,1.,3.54436163300443));
#38706=CARTESIAN_POINT('Ctrl Pts',(1.96130926212689,-1.,3.53674730625813));
#38707=CARTESIAN_POINT('Ctrl Pts',(1.96130926212689,1.,3.53674730625813));
#38708=CARTESIAN_POINT('Ctrl Pts',(1.96030879411566,-1.,3.52914648844351));
#38709=CARTESIAN_POINT('Ctrl Pts',(1.96030879411566,1.,3.52914648844351));
#38710=CARTESIAN_POINT('Ctrl Pts',(1.95926936324461,-1.,3.52155867431486));
#38711=CARTESIAN_POINT('Ctrl Pts',(1.95926936324461,1.,3.52155867431486));
#38712=CARTESIAN_POINT('Ctrl Pts',(1.95819025316779,-1.,3.51398354617794));
#38713=CARTESIAN_POINT('Ctrl Pts',(1.95819025316779,1.,3.51398354617794));
#38714=CARTESIAN_POINT('Ctrl Pts',(1.95707099606511,-1.,3.50642124159909));
#38715=CARTESIAN_POINT('Ctrl Pts',(1.95707099606511,1.,3.50642124159909));
#38716=CARTESIAN_POINT('Ctrl Pts',(1.95591153823661,-1.,3.49887263575583));
#38717=CARTESIAN_POINT('Ctrl Pts',(1.95591153823661,1.,3.49887263575583));
#38718=CARTESIAN_POINT('Ctrl Pts',(1.95471236969643,-1.,3.49133956289133));
#38719=CARTESIAN_POINT('Ctrl Pts',(1.95471236969643,1.,3.49133956289133));
#38720=CARTESIAN_POINT('Ctrl Pts',(1.95347412486308,-1.,3.48382414832634));
#38721=CARTESIAN_POINT('Ctrl Pts',(1.95347412486308,1.,3.48382414832634));
#38722=CARTESIAN_POINT('Ctrl Pts',(1.95219722189876,-1.,3.47632820495921));
#38723=CARTESIAN_POINT('Ctrl Pts',(1.95219722189876,1.,3.47632820495921));
#38724=CARTESIAN_POINT('Ctrl Pts',(1.95088147859876,-1.,3.46885258974191));
#38725=CARTESIAN_POINT('Ctrl Pts',(1.95088147859876,1.,3.46885258974191));
#38726=CARTESIAN_POINT('Ctrl Pts',(1.94952575850197,-1.,3.46139661060962));
#38727=CARTESIAN_POINT('Ctrl Pts',(1.94952575850197,1.,3.46139661060962));
#38728=CARTESIAN_POINT('Ctrl Pts',(1.94812754766524,-1.,3.45395731584051));
#38729=CARTESIAN_POINT('Ctrl Pts',(1.94812754766524,1.,3.45395731584051));
#38730=CARTESIAN_POINT('Ctrl Pts',(1.94668377715329,-1.,3.44653088665681));
#38731=CARTESIAN_POINT('Ctrl Pts',(1.94668377715329,1.,3.44653088665681));
#38732=CARTESIAN_POINT('Ctrl Pts',(1.94519168842879,-1.,3.43911410197687));
#38733=CARTESIAN_POINT('Ctrl Pts',(1.94519168842879,1.,3.43911410197687));
#38734=CARTESIAN_POINT('Ctrl Pts',(1.94364973660284,-1.,3.43170586602434));
#38735=CARTESIAN_POINT('Ctrl Pts',(1.94364973660284,1.,3.43170586602434));
#38736=CARTESIAN_POINT('Ctrl Pts',(1.94205835913696,-1.,3.42430850941503));
#38737=CARTESIAN_POINT('Ctrl Pts',(1.94205835913696,1.,3.42430850941503));
#38738=CARTESIAN_POINT('Ctrl Pts',(1.94042111965246,-1.,3.41692971994096));
#38739=CARTESIAN_POINT('Ctrl Pts',(1.94042111965246,1.,3.41692971994096));
#38740=CARTESIAN_POINT('Ctrl Pts',(1.93874306008143,-1.,3.40957978266642));
#38741=CARTESIAN_POINT('Ctrl Pts',(1.93874306008143,1.,3.40957978266642));
#38742=CARTESIAN_POINT('Ctrl Pts',(1.93702857723098,-1.,3.40226802104109));
#38743=CARTESIAN_POINT('Ctrl Pts',(1.93702857723098,1.,3.40226802104109));
#38744=CARTESIAN_POINT('Ctrl Pts',(1.93527929945985,-1.,3.39499923640795));
#38745=CARTESIAN_POINT('Ctrl Pts',(1.93527929945985,1.,3.39499923640795));
#38746=CARTESIAN_POINT('Ctrl Pts',(1.93349233176788,-1.,3.38777076883256));
#38747=CARTESIAN_POINT('Ctrl Pts',(1.93349233176788,1.,3.38777076883256));
#38748=CARTESIAN_POINT('Ctrl Pts',(1.93165739093276,-1.,3.3805676852555));
#38749=CARTESIAN_POINT('Ctrl Pts',(1.93165739093276,1.,3.3805676852555));
#38750=CARTESIAN_POINT('Ctrl Pts',(1.92975993109877,-1.,3.37336807068043));
#38751=CARTESIAN_POINT('Ctrl Pts',(1.92975993109877,1.,3.37336807068043));
#38752=CARTESIAN_POINT('Ctrl Pts',(1.92778626543786,-1.,3.36615168657567));
#38753=CARTESIAN_POINT('Ctrl Pts',(1.92778626543786,1.,3.36615168657567));
#38754=CARTESIAN_POINT('Ctrl Pts',(1.92572846125756,-1.,3.35890824422965));
#38755=CARTESIAN_POINT('Ctrl Pts',(1.92572846125756,1.,3.35890824422965));
#38756=CARTESIAN_POINT('Ctrl Pts',(1.92358838440528,-1.,3.35164424847223));
#38757=CARTESIAN_POINT('Ctrl Pts',(1.92358838440528,1.,3.35164424847223));
#38758=CARTESIAN_POINT('Ctrl Pts',(1.92138450828404,-1.,3.34439448941961));
#38759=CARTESIAN_POINT('Ctrl Pts',(1.92138450828404,1.,3.34439448941961));
#38760=CARTESIAN_POINT('Ctrl Pts',(1.9191460961021,-1.,3.33721230710012));
#38761=CARTESIAN_POINT('Ctrl Pts',(1.9191460961021,1.,3.33721230710012));
#38762=CARTESIAN_POINT('Ctrl Pts',(1.91690081930331,-1.,3.33014884257873));
#38763=CARTESIAN_POINT('Ctrl Pts',(1.91690081930331,1.,3.33014884257873));
#38764=CARTESIAN_POINT('Ctrl Pts',(1.91466343916627,-1.,3.32323403454535));
#38765=CARTESIAN_POINT('Ctrl Pts',(1.91466343916627,1.,3.32323403454535));
#38766=CARTESIAN_POINT('Ctrl Pts',(1.91242616234442,-1.,3.31646052426364));
#38767=CARTESIAN_POINT('Ctrl Pts',(1.91242616234442,1.,3.31646052426364));
#38768=CARTESIAN_POINT('Ctrl Pts',(1.91014297830446,-1.,3.30975721158596));
#38769=CARTESIAN_POINT('Ctrl Pts',(1.91014297830446,1.,3.30975721158596));
#38770=CARTESIAN_POINT('Ctrl Pts',(1.90773912171341,-1.,3.30300595568195));
#38771=CARTESIAN_POINT('Ctrl Pts',(1.90773912171341,1.,3.30300595568195));
#38772=CARTESIAN_POINT('Ctrl Pts',(1.90513891864087,-1.,3.29608978722113));
#38773=CARTESIAN_POINT('Ctrl Pts',(1.90513891864087,1.,3.29608978722113));
#38774=CARTESIAN_POINT('Ctrl Pts',(1.90228971247527,-1.,3.2889344860029));
#38775=CARTESIAN_POINT('Ctrl Pts',(1.90228971247527,1.,3.2889344860029));
#38776=CARTESIAN_POINT('Ctrl Pts',(1.89918429230462,-1.,3.28154737912352));
#38777=CARTESIAN_POINT('Ctrl Pts',(1.89918429230462,1.,3.28154737912352));
#38778=CARTESIAN_POINT('Ctrl Pts',(1.89589172903793,-1.,3.27407108933139));
#38779=CARTESIAN_POINT('Ctrl Pts',(1.89589172903793,1.,3.27407108933139));
#38780=CARTESIAN_POINT('Ctrl Pts',(1.89255393500965,-1.,3.26677653888676));
#38781=CARTESIAN_POINT('Ctrl Pts',(1.89255393500965,1.,3.26677653888676));
#38782=CARTESIAN_POINT('Ctrl Pts',(1.88934996203698,-1.,3.25999885193947));
#38783=CARTESIAN_POINT('Ctrl Pts',(1.88934996203698,1.,3.25999885193947));
#38784=CARTESIAN_POINT('Ctrl Pts',(1.88646802523466,-1.,3.25408686339463));
#38785=CARTESIAN_POINT('Ctrl Pts',(1.88646802523466,1.,3.25408686339463));
#38786=CARTESIAN_POINT('Ctrl Pts',(1.88407708646357,-1.,3.24935200511918));
#38787=CARTESIAN_POINT('Ctrl Pts',(1.88407708646357,1.,3.24935200511918));
#38788=CARTESIAN_POINT('Ctrl Pts',(1.88229202582941,-1.,3.24600543790443));
#38789=CARTESIAN_POINT('Ctrl Pts',(1.88229202582941,1.,3.24600543790443));
#38790=CARTESIAN_POINT('Ctrl Pts',(1.88139187908074,-1.,3.24451807186481));
#38791=CARTESIAN_POINT('Ctrl Pts',(1.88139187908074,1.,3.24451807186481));
#38792=CARTESIAN_POINT('Ctrl Pts',(1.88102201872555,-1.,3.24408699284121));
#38793=CARTESIAN_POINT('Ctrl Pts',(1.88102201872555,1.,3.24408699284121));
#38794=CARTESIAN_POINT('Ctrl Pts',(1.88091100680349,-1.,3.24410359189609));
#38795=CARTESIAN_POINT('Ctrl Pts',(1.88091100680349,1.,3.24410359189609));
#38796=CARTESIAN_POINT('Ctrl Pts',(1.8808893942881,-1.,3.24418789321065));
#38797=CARTESIAN_POINT('Ctrl Pts',(1.8808893942881,1.,3.24418789321065));
#38798=CARTESIAN_POINT('',(1.97421938526992,1.,3.70708211654725));
#38799=CARTESIAN_POINT('Ctrl Pts',(1.97421938526992,1.,3.70708211654725));
#38800=CARTESIAN_POINT('Ctrl Pts',(1.97417727645308,1.,3.70551008132332));
#38801=CARTESIAN_POINT('Ctrl Pts',(1.97408973726715,1.,3.70236698912904));
#38802=CARTESIAN_POINT('Ctrl Pts',(1.97394846383216,1.,3.6976552856004));
#38803=CARTESIAN_POINT('Ctrl Pts',(1.97374016225483,1.,3.69137888599902));
#38804=CARTESIAN_POINT('Ctrl Pts',(1.97344650304519,1.,3.68354319915092));
#38805=CARTESIAN_POINT('Ctrl Pts',(1.97311947678516,1.,3.67571738107084));
#38806=CARTESIAN_POINT('Ctrl Pts',(1.97275897198678,1.,3.66790152752075));
#38807=CARTESIAN_POINT('Ctrl Pts',(1.9723648543905,1.,3.6600957816636));
#38808=CARTESIAN_POINT('Ctrl Pts',(1.97193697240239,1.,3.652300347166));
#38809=CARTESIAN_POINT('Ctrl Pts',(1.97147515441164,1.,3.64451546723514));
#38810=CARTESIAN_POINT('Ctrl Pts',(1.97097920454464,1.,3.63674139590412));
#38811=CARTESIAN_POINT('Ctrl Pts',(1.97044889850463,1.,3.62897836973293));
#38812=CARTESIAN_POINT('Ctrl Pts',(1.96988398129978,1.,3.62122658401893));
#38813=CARTESIAN_POINT('Ctrl Pts',(1.96928416040877,1.,3.61348615496704));
#38814=CARTESIAN_POINT('Ctrl Pts',(1.9686491188594,1.,3.60575714017989));
#38815=CARTESIAN_POINT('Ctrl Pts',(1.96797854118369,1.,3.59803959819938));
#38816=CARTESIAN_POINT('Ctrl Pts',(1.96727213799544,1.,3.59033364022801));
#38817=CARTESIAN_POINT('Ctrl Pts',(1.96652966688911,1.,3.58263947663829));
#38818=CARTESIAN_POINT('Ctrl Pts',(1.96575096652789,1.,3.57495748600959));
#38819=CARTESIAN_POINT('Ctrl Pts',(1.96493594634567,1.,3.56728820357791));
#38820=CARTESIAN_POINT('Ctrl Pts',(1.96408450906812,1.,3.55963218706096));
#38821=CARTESIAN_POINT('Ctrl Pts',(1.96319648628644,1.,3.55198990600886));
#38822=CARTESIAN_POINT('Ctrl Pts',(1.96227157573067,1.,3.54436163300443));
#38823=CARTESIAN_POINT('Ctrl Pts',(1.96130926212689,1.,3.53674730625813));
#38824=CARTESIAN_POINT('Ctrl Pts',(1.96030879411566,1.,3.52914648844351));
#38825=CARTESIAN_POINT('Ctrl Pts',(1.95926936324461,1.,3.52155867431486));
#38826=CARTESIAN_POINT('Ctrl Pts',(1.95819025316779,1.,3.51398354617794));
#38827=CARTESIAN_POINT('Ctrl Pts',(1.95707099606511,1.,3.50642124159909));
#38828=CARTESIAN_POINT('Ctrl Pts',(1.95591153823661,1.,3.49887263575583));
#38829=CARTESIAN_POINT('Ctrl Pts',(1.95471236969643,1.,3.49133956289133));
#38830=CARTESIAN_POINT('Ctrl Pts',(1.95347412486308,1.,3.48382414832634));
#38831=CARTESIAN_POINT('Ctrl Pts',(1.95219722189876,1.,3.47632820495921));
#38832=CARTESIAN_POINT('Ctrl Pts',(1.95088147859876,1.,3.46885258974191));
#38833=CARTESIAN_POINT('Ctrl Pts',(1.94952575850197,1.,3.46139661060962));
#38834=CARTESIAN_POINT('Ctrl Pts',(1.94812754766524,1.,3.45395731584051));
#38835=CARTESIAN_POINT('Ctrl Pts',(1.94668377715329,1.,3.44653088665681));
#38836=CARTESIAN_POINT('Ctrl Pts',(1.94519168842879,1.,3.43911410197687));
#38837=CARTESIAN_POINT('Ctrl Pts',(1.94364973660284,1.,3.43170586602434));
#38838=CARTESIAN_POINT('Ctrl Pts',(1.94205835913696,1.,3.42430850941503));
#38839=CARTESIAN_POINT('Ctrl Pts',(1.94042111965246,1.,3.41692971994096));
#38840=CARTESIAN_POINT('Ctrl Pts',(1.93874306008143,1.,3.40957978266642));
#38841=CARTESIAN_POINT('Ctrl Pts',(1.93702857723098,1.,3.40226802104109));
#38842=CARTESIAN_POINT('Ctrl Pts',(1.93527929945985,1.,3.39499923640795));
#38843=CARTESIAN_POINT('Ctrl Pts',(1.93349233176788,1.,3.38777076883256));
#38844=CARTESIAN_POINT('Ctrl Pts',(1.93165739093276,1.,3.3805676852555));
#38845=CARTESIAN_POINT('Ctrl Pts',(1.92975993109877,1.,3.37336807068043));
#38846=CARTESIAN_POINT('Ctrl Pts',(1.92778626543786,1.,3.36615168657567));
#38847=CARTESIAN_POINT('Ctrl Pts',(1.92572846125756,1.,3.35890824422965));
#38848=CARTESIAN_POINT('Ctrl Pts',(1.92358838440528,1.,3.35164424847223));
#38849=CARTESIAN_POINT('Ctrl Pts',(1.92138450828404,1.,3.34439448941961));
#38850=CARTESIAN_POINT('Ctrl Pts',(1.9191460961021,1.,3.33721230710012));
#38851=CARTESIAN_POINT('Ctrl Pts',(1.91690081930331,1.,3.33014884257873));
#38852=CARTESIAN_POINT('Ctrl Pts',(1.91466343916627,1.,3.32323403454535));
#38853=CARTESIAN_POINT('Ctrl Pts',(1.91242616234442,1.,3.31646052426364));
#38854=CARTESIAN_POINT('Ctrl Pts',(1.91014297830446,1.,3.30975721158596));
#38855=CARTESIAN_POINT('Ctrl Pts',(1.90773912171341,1.,3.30300595568195));
#38856=CARTESIAN_POINT('Ctrl Pts',(1.90513891864087,1.,3.29608978722113));
#38857=CARTESIAN_POINT('Ctrl Pts',(1.90228971247527,1.,3.2889344860029));
#38858=CARTESIAN_POINT('Ctrl Pts',(1.89918429230462,1.,3.28154737912352));
#38859=CARTESIAN_POINT('Ctrl Pts',(1.89589172903793,1.,3.27407108933139));
#38860=CARTESIAN_POINT('Ctrl Pts',(1.89255393500965,1.,3.26677653888676));
#38861=CARTESIAN_POINT('Ctrl Pts',(1.88934996203698,1.,3.25999885193947));
#38862=CARTESIAN_POINT('Ctrl Pts',(1.88646802523466,1.,3.25408686339463));
#38863=CARTESIAN_POINT('Ctrl Pts',(1.88407708646357,1.,3.24935200511918));
#38864=CARTESIAN_POINT('Ctrl Pts',(1.88242596600454,1.,3.2462565441079));
#38865=CARTESIAN_POINT('Ctrl Pts',(1.88156537699203,1.,3.24480754676064));
#38866=CARTESIAN_POINT('Ctrl Pts',(1.88117508446775,1.,3.24428080353022));
#38867=CARTESIAN_POINT('Ctrl Pts',(1.8810229239812,1.,3.24415531671284));
#38868=CARTESIAN_POINT('Ctrl Pts',(1.88097764062697,1.,3.24413672884812));
#38869=CARTESIAN_POINT('',(1.97421938526992,0.,3.70708211654725));
#38870=CARTESIAN_POINT('Ctrl Pts',(1.519044091397,-1.,3.42855728381368));
#38871=CARTESIAN_POINT('Ctrl Pts',(1.519044091397,1.,3.42855728381368));
#38872=CARTESIAN_POINT('Ctrl Pts',(1.51896318668366,-1.,3.42852521763778));
#38873=CARTESIAN_POINT('Ctrl Pts',(1.51896318668366,1.,3.42852521763778));
#38874=CARTESIAN_POINT('Ctrl Pts',(1.51888450659652,-1.,3.42860527149177));
#38875=CARTESIAN_POINT('Ctrl Pts',(1.51888450659652,1.,3.42860527149177));
#38876=CARTESIAN_POINT('Ctrl Pts',(1.51901585839109,-1.,3.42915787669893));
#38877=CARTESIAN_POINT('Ctrl Pts',(1.51901585839109,1.,3.42915787669893));
#38878=CARTESIAN_POINT('Ctrl Pts',(1.51969006980999,-1.,3.43076036253837));
#38879=CARTESIAN_POINT('Ctrl Pts',(1.51969006980999,1.,3.43076036253837));
#38880=CARTESIAN_POINT('Ctrl Pts',(1.52134826724292,-1.,3.43417156977893));
#38881=CARTESIAN_POINT('Ctrl Pts',(1.52134826724292,1.,3.43417156977893));
#38882=CARTESIAN_POINT('Ctrl Pts',(1.5237734895035,-1.,3.4388889597401));
#38883=CARTESIAN_POINT('Ctrl Pts',(1.5237734895035,1.,3.4388889597401));
#38884=CARTESIAN_POINT('Ctrl Pts',(1.52686242875556,-1.,3.44469547526647));
#38885=CARTESIAN_POINT('Ctrl Pts',(1.52686242875556,1.,3.44469547526647));
#38886=CARTESIAN_POINT('Ctrl Pts',(1.53046244461635,-1.,3.45127136828305));
#38887=CARTESIAN_POINT('Ctrl Pts',(1.53046244461635,1.,3.45127136828305));
#38888=CARTESIAN_POINT('Ctrl Pts',(1.53440195378792,-1.,3.45825932955032));
#38889=CARTESIAN_POINT('Ctrl Pts',(1.53440195378792,1.,3.45825932955032));
#38890=CARTESIAN_POINT('Ctrl Pts',(1.53851507915502,-1.,3.46531752207153));
#38891=CARTESIAN_POINT('Ctrl Pts',(1.53851507915502,1.,3.46531752207153));
#38892=CARTESIAN_POINT('Ctrl Pts',(1.54266605398187,-1.,3.47217189224653));
#38893=CARTESIAN_POINT('Ctrl Pts',(1.54266605398187,1.,3.47217189224653));
#38894=CARTESIAN_POINT('Ctrl Pts',(1.54678009290276,-1.,3.47868272898751));
#38895=CARTESIAN_POINT('Ctrl Pts',(1.54678009290276,1.,3.47868272898751));
#38896=CARTESIAN_POINT('Ctrl Pts',(1.55084702970452,-1.,3.48485155928567));
#38897=CARTESIAN_POINT('Ctrl Pts',(1.55084702970452,1.,3.48485155928567));
#38898=CARTESIAN_POINT('Ctrl Pts',(1.55489595901116,-1.,3.4907646087742));
#38899=CARTESIAN_POINT('Ctrl Pts',(1.55489595901116,1.,3.4907646087742));
#38900=CARTESIAN_POINT('Ctrl Pts',(1.55897703097874,-1.,3.49655185179655));
#38901=CARTESIAN_POINT('Ctrl Pts',(1.55897703097874,1.,3.49655185179655));
#38902=CARTESIAN_POINT('Ctrl Pts',(1.56314187758675,-1.,3.50234321621578));
#38903=CARTESIAN_POINT('Ctrl Pts',(1.56314187758675,1.,3.50234321621578));
#38904=CARTESIAN_POINT('Ctrl Pts',(1.56742097575012,-1.,3.50821771695363));
#38905=CARTESIAN_POINT('Ctrl Pts',(1.56742097575012,1.,3.50821771695363));
#38906=CARTESIAN_POINT('Ctrl Pts',(1.57181569799743,-1.,3.51418598431665));
#38907=CARTESIAN_POINT('Ctrl Pts',(1.57181569799743,1.,3.51418598431665));
#38908=CARTESIAN_POINT('Ctrl Pts',(1.57631049988158,-1.,3.52021847865912));
#38909=CARTESIAN_POINT('Ctrl Pts',(1.57631049988158,1.,3.52021847865912));
#38910=CARTESIAN_POINT('Ctrl Pts',(1.58088027227848,-1.,3.52626275334881));
#38911=CARTESIAN_POINT('Ctrl Pts',(1.58088027227848,1.,3.52626275334881));
#38912=CARTESIAN_POINT('Ctrl Pts',(1.58549906268088,-1.,3.5322637814708));
#38913=CARTESIAN_POINT('Ctrl Pts',(1.58549906268088,1.,3.5322637814708));
#38914=CARTESIAN_POINT('Ctrl Pts',(1.59014958368739,-1.,3.53818616861077));
#38915=CARTESIAN_POINT('Ctrl Pts',(1.59014958368739,1.,3.53818616861077));
#38916=CARTESIAN_POINT('Ctrl Pts',(1.59482766949766,-1.,3.54402458182337));
#38917=CARTESIAN_POINT('Ctrl Pts',(1.59482766949766,1.,3.54402458182337));
#38918=CARTESIAN_POINT('Ctrl Pts',(1.59953698113457,-1.,3.54979148634454));
#38919=CARTESIAN_POINT('Ctrl Pts',(1.59953698113457,1.,3.54979148634454));
#38920=CARTESIAN_POINT('Ctrl Pts',(1.60428584699853,-1.,3.55550985096129));
#38921=CARTESIAN_POINT('Ctrl Pts',(1.60428584699853,1.,3.55550985096129));
#38922=CARTESIAN_POINT('Ctrl Pts',(1.60908344685457,-1.,3.5612043248298));
#38923=CARTESIAN_POINT('Ctrl Pts',(1.60908344685457,1.,3.5612043248298));
#38924=CARTESIAN_POINT('Ctrl Pts',(1.61393581747514,-1.,3.56689200468387));
#38925=CARTESIAN_POINT('Ctrl Pts',(1.61393581747514,1.,3.56689200468387));
#38926=CARTESIAN_POINT('Ctrl Pts',(1.61884340915404,-1.,3.57257679609806));
#38927=CARTESIAN_POINT('Ctrl Pts',(1.61884340915404,1.,3.57257679609806));
#38928=CARTESIAN_POINT('Ctrl Pts',(1.62380329464844,-1.,3.5782545595439));
#38929=CARTESIAN_POINT('Ctrl Pts',(1.62380329464844,1.,3.5782545595439));
#38930=CARTESIAN_POINT('Ctrl Pts',(1.62881051550745,-1.,3.58391625774343));
#38931=CARTESIAN_POINT('Ctrl Pts',(1.62881051550745,1.,3.58391625774343));
#38932=CARTESIAN_POINT('Ctrl Pts',(1.6338597145126,-1.,3.58955176627879));
#38933=CARTESIAN_POINT('Ctrl Pts',(1.6338597145126,1.,3.58955176627879));
#38934=CARTESIAN_POINT('Ctrl Pts',(1.63894676675352,-1.,3.59515368334893));
#38935=CARTESIAN_POINT('Ctrl Pts',(1.63894676675352,1.,3.59515368334893));
#38936=CARTESIAN_POINT('Ctrl Pts',(1.64407004385582,-1.,3.60072028513845));
#38937=CARTESIAN_POINT('Ctrl Pts',(1.64407004385582,1.,3.60072028513845));
#38938=CARTESIAN_POINT('Ctrl Pts',(1.64922952425832,-1.,3.60625346556992));
#38939=CARTESIAN_POINT('Ctrl Pts',(1.64922952425832,1.,3.60625346556992));
#38940=CARTESIAN_POINT('Ctrl Pts',(1.65442619244325,-1.,3.61175734965127));
#38941=CARTESIAN_POINT('Ctrl Pts',(1.65442619244325,1.,3.61175734965127));
#38942=CARTESIAN_POINT('Ctrl Pts',(1.65966133399186,-1.,3.61723666482456));
#38943=CARTESIAN_POINT('Ctrl Pts',(1.65966133399186,1.,3.61723666482456));
#38944=CARTESIAN_POINT('Ctrl Pts',(1.66493585923855,-1.,3.62269517989109));
#38945=CARTESIAN_POINT('Ctrl Pts',(1.66493585923855,1.,3.62269517989109));
#38946=CARTESIAN_POINT('Ctrl Pts',(1.67024966008044,-1.,3.62813422105271));
#38947=CARTESIAN_POINT('Ctrl Pts',(1.67024966008044,1.,3.62813422105271));
#38948=CARTESIAN_POINT('Ctrl Pts',(1.67560193613156,-1.,3.63355343201232));
#38949=CARTESIAN_POINT('Ctrl Pts',(1.67560193613156,1.,3.63355343201232));
#38950=CARTESIAN_POINT('Ctrl Pts',(1.68099146651586,-1.,3.63895140887462));
#38951=CARTESIAN_POINT('Ctrl Pts',(1.68099146651586,1.,3.63895140887462));
#38952=CARTESIAN_POINT('Ctrl Pts',(1.68641690471457,-1.,3.64432638915203));
#38953=CARTESIAN_POINT('Ctrl Pts',(1.68641690471457,1.,3.64432638915203));
#38954=CARTESIAN_POINT('Ctrl Pts',(1.69187705481689,-1.,3.64967689827371));
#38955=CARTESIAN_POINT('Ctrl Pts',(1.69187705481689,1.,3.64967689827371));
#38956=CARTESIAN_POINT('Ctrl Pts',(1.69737117722534,-1.,3.65500246526749));
#38957=CARTESIAN_POINT('Ctrl Pts',(1.69737117722534,1.,3.65500246526749));
#38958=CARTESIAN_POINT('Ctrl Pts',(1.70289888566873,-1.,3.66030338774847));
#38959=CARTESIAN_POINT('Ctrl Pts',(1.70289888566873,1.,3.66030338774847));
#38960=CARTESIAN_POINT('Ctrl Pts',(1.70846001610956,-1.,3.66558043198876));
#38961=CARTESIAN_POINT('Ctrl Pts',(1.70846001610956,1.,3.66558043198876));
#38962=CARTESIAN_POINT('Ctrl Pts',(1.71405450210383,-1.,3.67083454901611));
#38963=CARTESIAN_POINT('Ctrl Pts',(1.71405450210383,1.,3.67083454901611));
#38964=CARTESIAN_POINT('Ctrl Pts',(1.71968225581808,-1.,3.67606660374709));
#38965=CARTESIAN_POINT('Ctrl Pts',(1.71968225581808,1.,3.67606660374709));
#38966=CARTESIAN_POINT('Ctrl Pts',(1.72534302437056,-1.,3.68127704936579));
#38967=CARTESIAN_POINT('Ctrl Pts',(1.72534302437056,1.,3.68127704936579));
#38968=CARTESIAN_POINT('Ctrl Pts',(1.73103640956717,-1.,3.68646597019332));
#38969=CARTESIAN_POINT('Ctrl Pts',(1.73103640956717,1.,3.68646597019332));
#38970=CARTESIAN_POINT('Ctrl Pts',(1.73676193254557,-1.,3.69163322648036));
#38971=CARTESIAN_POINT('Ctrl Pts',(1.73676193254557,1.,3.69163322648036));
#38972=CARTESIAN_POINT('Ctrl Pts',(1.74251908492617,-1.,3.69677856910517));
#38973=CARTESIAN_POINT('Ctrl Pts',(1.74251908492617,1.,3.69677856910517));
#38974=CARTESIAN_POINT('Ctrl Pts',(1.74830738046057,-1.,3.7019017567335));
#38975=CARTESIAN_POINT('Ctrl Pts',(1.74830738046057,1.,3.7019017567335));
#38976=CARTESIAN_POINT('Ctrl Pts',(1.75412641804042,-1.,3.70700269736659));
#38977=CARTESIAN_POINT('Ctrl Pts',(1.75412641804042,1.,3.70700269736659));
#38978=CARTESIAN_POINT('Ctrl Pts',(1.75997588498865,-1.,3.71208146346136));
#38979=CARTESIAN_POINT('Ctrl Pts',(1.75997588498865,1.,3.71208146346136));
#38980=CARTESIAN_POINT('Ctrl Pts',(1.76585552124394,-1.,3.71713822377359));
#38981=CARTESIAN_POINT('Ctrl Pts',(1.76585552124394,1.,3.71713822377359));
#38982=CARTESIAN_POINT('Ctrl Pts',(1.77176509401761,-1.,3.72217319911254));
#38983=CARTESIAN_POINT('Ctrl Pts',(1.77176509401761,1.,3.72217319911254));
#38984=CARTESIAN_POINT('Ctrl Pts',(1.77770437039658,-1.,3.72718661205609));
#38985=CARTESIAN_POINT('Ctrl Pts',(1.77770437039658,1.,3.72718661205609));
#38986=CARTESIAN_POINT('Ctrl Pts',(1.78367308442901,-1.,3.7321786309547));
#38987=CARTESIAN_POINT('Ctrl Pts',(1.78367308442901,1.,3.7321786309547));
#38988=CARTESIAN_POINT('Ctrl Pts',(1.78967092823491,-1.,3.73714934730681));
#38989=CARTESIAN_POINT('Ctrl Pts',(1.78967092823491,1.,3.73714934730681));
#38990=CARTESIAN_POINT('Ctrl Pts',(1.79569757859422,-1.,3.74209880352445));
#38991=CARTESIAN_POINT('Ctrl Pts',(1.79569757859422,1.,3.74209880352445));
#38992=CARTESIAN_POINT('Ctrl Pts',(1.8017527148577,-1.,3.74702700875467));
#38993=CARTESIAN_POINT('Ctrl Pts',(1.8017527148577,1.,3.74702700875467));
#38994=CARTESIAN_POINT('Ctrl Pts',(1.80783603939617,-1.,3.75193395887977));
#38995=CARTESIAN_POINT('Ctrl Pts',(1.80783603939617,1.,3.75193395887977));
#38996=CARTESIAN_POINT('Ctrl Pts',(1.8139472983358,-1.,3.75681965683071));
#38997=CARTESIAN_POINT('Ctrl Pts',(1.8139472983358,1.,3.75681965683071));
#38998=CARTESIAN_POINT('Ctrl Pts',(1.82008629694091,-1.,3.76168412707948));
#38999=CARTESIAN_POINT('Ctrl Pts',(1.82008629694091,1.,3.76168412707948));
#39000=CARTESIAN_POINT('Ctrl Pts',(1.82625289220915,-1.,3.76652740353775));
#39001=CARTESIAN_POINT('Ctrl Pts',(1.82625289220915,1.,3.76652740353775));
#39002=CARTESIAN_POINT('Ctrl Pts',(1.83120816955645,-1.,3.77038509817999));
#39003=CARTESIAN_POINT('Ctrl Pts',(1.83120816955645,1.,3.77038509817999));
#39004=CARTESIAN_POINT('Ctrl Pts',(1.83493697934534,-1.,3.77326886064398));
#39005=CARTESIAN_POINT('Ctrl Pts',(1.83493697934534,1.,3.77326886064398));
#39006=CARTESIAN_POINT('Ctrl Pts',(1.83742834010626,-1.,3.77518714457833));
#39007=CARTESIAN_POINT('Ctrl Pts',(1.83742834010626,1.,3.77518714457833));
#39008=CARTESIAN_POINT('Ctrl Pts',(1.8386753923786,-1.,3.77614523045147));
#39009=CARTESIAN_POINT('Ctrl Pts',(1.8386753923786,1.,3.77614523045147));
#39010=CARTESIAN_POINT('',(1.5189508286633,1.,3.42859860294306));
#39011=CARTESIAN_POINT('Ctrl Pts',(1.5189508286633,-1.,3.42859860294306));
#39012=CARTESIAN_POINT('Ctrl Pts',(1.5189508286633,-0.666666666666667,3.42859860294306));
#39013=CARTESIAN_POINT('Ctrl Pts',(1.5189508286633,-0.333333333333333,3.42859860294306));
#39014=CARTESIAN_POINT('Ctrl Pts',(1.5189508286633,0.333333333333333,3.42859860294306));
#39015=CARTESIAN_POINT('Ctrl Pts',(1.5189508286633,0.666666666666667,3.42859860294306));
#39016=CARTESIAN_POINT('Ctrl Pts',(1.5189508286633,1.,3.42859860294306));
#39017=CARTESIAN_POINT('',(1.8386753923786,1.,3.77614523045147));
#39018=CARTESIAN_POINT('',(1.8386753923786,0.,3.77614523045147));
#39019=CARTESIAN_POINT('Ctrl Pts',(1.5189508286633,1.,3.42859860294306));
#39020=CARTESIAN_POINT('Ctrl Pts',(1.51893924967331,1.,3.42864616361875));
#39021=CARTESIAN_POINT('Ctrl Pts',(1.5189513329503,1.,3.42884302333841));
#39022=CARTESIAN_POINT('Ctrl Pts',(1.51914806898491,1.,3.42946838852587));
#39023=CARTESIAN_POINT('Ctrl Pts',(1.5198144909338,1.,3.43101631893414));
#39024=CARTESIAN_POINT('Ctrl Pts',(1.52134826724292,1.,3.43417156977893));
#39025=CARTESIAN_POINT('Ctrl Pts',(1.5237734895035,1.,3.4388889597401));
#39026=CARTESIAN_POINT('Ctrl Pts',(1.52686242875556,1.,3.44469547526647));
#39027=CARTESIAN_POINT('Ctrl Pts',(1.53046244461635,1.,3.45127136828305));
#39028=CARTESIAN_POINT('Ctrl Pts',(1.53440195378792,1.,3.45825932955032));
#39029=CARTESIAN_POINT('Ctrl Pts',(1.53851507915502,1.,3.46531752207153));
#39030=CARTESIAN_POINT('Ctrl Pts',(1.54266605398187,1.,3.47217189224653));
#39031=CARTESIAN_POINT('Ctrl Pts',(1.54678009290276,1.,3.47868272898751));
#39032=CARTESIAN_POINT('Ctrl Pts',(1.55084702970452,1.,3.48485155928567));
#39033=CARTESIAN_POINT('Ctrl Pts',(1.55489595901116,1.,3.4907646087742));
#39034=CARTESIAN_POINT('Ctrl Pts',(1.55897703097874,1.,3.49655185179655));
#39035=CARTESIAN_POINT('Ctrl Pts',(1.56314187758675,1.,3.50234321621578));
#39036=CARTESIAN_POINT('Ctrl Pts',(1.56742097575012,1.,3.50821771695363));
#39037=CARTESIAN_POINT('Ctrl Pts',(1.57181569799743,1.,3.51418598431665));
#39038=CARTESIAN_POINT('Ctrl Pts',(1.57631049988158,1.,3.52021847865912));
#39039=CARTESIAN_POINT('Ctrl Pts',(1.58088027227848,1.,3.52626275334881));
#39040=CARTESIAN_POINT('Ctrl Pts',(1.58549906268088,1.,3.5322637814708));
#39041=CARTESIAN_POINT('Ctrl Pts',(1.59014958368739,1.,3.53818616861077));
#39042=CARTESIAN_POINT('Ctrl Pts',(1.59482766949766,1.,3.54402458182337));
#39043=CARTESIAN_POINT('Ctrl Pts',(1.59953698113457,1.,3.54979148634454));
#39044=CARTESIAN_POINT('Ctrl Pts',(1.60428584699853,1.,3.55550985096129));
#39045=CARTESIAN_POINT('Ctrl Pts',(1.60908344685457,1.,3.5612043248298));
#39046=CARTESIAN_POINT('Ctrl Pts',(1.61393581747514,1.,3.56689200468387));
#39047=CARTESIAN_POINT('Ctrl Pts',(1.61884340915404,1.,3.57257679609806));
#39048=CARTESIAN_POINT('Ctrl Pts',(1.62380329464844,1.,3.5782545595439));
#39049=CARTESIAN_POINT('Ctrl Pts',(1.62881051550745,1.,3.58391625774343));
#39050=CARTESIAN_POINT('Ctrl Pts',(1.6338597145126,1.,3.58955176627879));
#39051=CARTESIAN_POINT('Ctrl Pts',(1.63894676675352,1.,3.59515368334893));
#39052=CARTESIAN_POINT('Ctrl Pts',(1.64407004385582,1.,3.60072028513845));
#39053=CARTESIAN_POINT('Ctrl Pts',(1.64922952425832,1.,3.60625346556992));
#39054=CARTESIAN_POINT('Ctrl Pts',(1.65442619244325,1.,3.61175734965127));
#39055=CARTESIAN_POINT('Ctrl Pts',(1.65966133399186,1.,3.61723666482456));
#39056=CARTESIAN_POINT('Ctrl Pts',(1.66493585923855,1.,3.62269517989109));
#39057=CARTESIAN_POINT('Ctrl Pts',(1.67024966008044,1.,3.62813422105271));
#39058=CARTESIAN_POINT('Ctrl Pts',(1.67560193613156,1.,3.63355343201232));
#39059=CARTESIAN_POINT('Ctrl Pts',(1.68099146651586,1.,3.63895140887462));
#39060=CARTESIAN_POINT('Ctrl Pts',(1.68641690471457,1.,3.64432638915203));
#39061=CARTESIAN_POINT('Ctrl Pts',(1.69187705481689,1.,3.64967689827371));
#39062=CARTESIAN_POINT('Ctrl Pts',(1.69737117722534,1.,3.65500246526749));
#39063=CARTESIAN_POINT('Ctrl Pts',(1.70289888566873,1.,3.66030338774847));
#39064=CARTESIAN_POINT('Ctrl Pts',(1.70846001610956,1.,3.66558043198876));
#39065=CARTESIAN_POINT('Ctrl Pts',(1.71405450210383,1.,3.67083454901611));
#39066=CARTESIAN_POINT('Ctrl Pts',(1.71968225581808,1.,3.67606660374709));
#39067=CARTESIAN_POINT('Ctrl Pts',(1.72534302437056,1.,3.68127704936579));
#39068=CARTESIAN_POINT('Ctrl Pts',(1.73103640956717,1.,3.68646597019332));
#39069=CARTESIAN_POINT('Ctrl Pts',(1.73676193254557,1.,3.69163322648036));
#39070=CARTESIAN_POINT('Ctrl Pts',(1.74251908492617,1.,3.69677856910517));
#39071=CARTESIAN_POINT('Ctrl Pts',(1.74830738046057,1.,3.7019017567335));
#39072=CARTESIAN_POINT('Ctrl Pts',(1.75412641804042,1.,3.70700269736659));
#39073=CARTESIAN_POINT('Ctrl Pts',(1.75997588498865,1.,3.71208146346136));
#39074=CARTESIAN_POINT('Ctrl Pts',(1.76585552124394,1.,3.71713822377359));
#39075=CARTESIAN_POINT('Ctrl Pts',(1.77176509401761,1.,3.72217319911254));
#39076=CARTESIAN_POINT('Ctrl Pts',(1.77770437039658,1.,3.72718661205609));
#39077=CARTESIAN_POINT('Ctrl Pts',(1.78367308442901,1.,3.7321786309547));
#39078=CARTESIAN_POINT('Ctrl Pts',(1.78967092823491,1.,3.73714934730681));
#39079=CARTESIAN_POINT('Ctrl Pts',(1.79569757859422,1.,3.74209880352445));
#39080=CARTESIAN_POINT('Ctrl Pts',(1.8017527148577,1.,3.74702700875467));
#39081=CARTESIAN_POINT('Ctrl Pts',(1.80783603939617,1.,3.75193395887977));
#39082=CARTESIAN_POINT('Ctrl Pts',(1.8139472983358,1.,3.75681965683071));
#39083=CARTESIAN_POINT('Ctrl Pts',(1.82008629694091,1.,3.76168412707948));
#39084=CARTESIAN_POINT('Ctrl Pts',(1.82625289220915,1.,3.76652740353775));
#39085=CARTESIAN_POINT('Ctrl Pts',(1.83120816955645,1.,3.77038509817999));
#39086=CARTESIAN_POINT('Ctrl Pts',(1.83493697934534,1.,3.77326886064398));
#39087=CARTESIAN_POINT('Ctrl Pts',(1.83742834010626,1.,3.77518714457833));
#39088=CARTESIAN_POINT('Ctrl Pts',(1.8386753923786,1.,3.77614523045147));
#39089=CARTESIAN_POINT('Origin',(1.8386753923786,0.,3.77614523045147));
#39090=CARTESIAN_POINT('',(1.97421938526992,1.,3.70708211654725));
#39091=CARTESIAN_POINT('Origin',(0.,0.,0.));
#39092=CARTESIAN_POINT('',(1.35032489087269,1.,3.49844575334386));
#39093=CARTESIAN_POINT('Origin',(0.,1.,0.));
#39094=CARTESIAN_POINT('Ctrl Pts',(1.35032489087269,1.,3.49844575334386));
#39095=CARTESIAN_POINT('Ctrl Pts',(1.35032489087269,0.666666666666667,3.49844575334386));
#39096=CARTESIAN_POINT('Ctrl Pts',(1.35032489087269,0.333333333333333,3.49844575334386));
#39097=CARTESIAN_POINT('Ctrl Pts',(1.35032489087269,-0.333333333333333,
3.49844575334386));
#39098=CARTESIAN_POINT('Ctrl Pts',(1.35032489087269,-0.666666666666667,
3.49844575334386));
#39099=CARTESIAN_POINT('Ctrl Pts',(1.35032489087269,-1.,3.49844575334386));
#39100=CARTESIAN_POINT('Ctrl Pts',(1.36999806084572,-1.,3.97027773754922));
#39101=CARTESIAN_POINT('Ctrl Pts',(1.36999806084572,1.,3.97027773754922));
#39102=CARTESIAN_POINT('Ctrl Pts',(1.37020239094758,-1.,3.9687184694173));
#39103=CARTESIAN_POINT('Ctrl Pts',(1.37020239094758,1.,3.9687184694173));
#39104=CARTESIAN_POINT('Ctrl Pts',(1.37060761746027,-1.,3.96560037975788));
#39105=CARTESIAN_POINT('Ctrl Pts',(1.37060761746027,1.,3.96560037975788));
#39106=CARTESIAN_POINT('Ctrl Pts',(1.37120515615663,-1.,3.96092458508407));
#39107=CARTESIAN_POINT('Ctrl Pts',(1.37120515615663,1.,3.96092458508407));
#39108=CARTESIAN_POINT('Ctrl Pts',(1.37198126433139,-1.,3.95469287283105));
#39109=CARTESIAN_POINT('Ctrl Pts',(1.37198126433139,1.,3.95469287283105));
#39110=CARTESIAN_POINT('Ctrl Pts',(1.37291699203423,-1.,3.94690771786926));
#39111=CARTESIAN_POINT('Ctrl Pts',(1.37291699203423,1.,3.94690771786926));
#39112=CARTESIAN_POINT('Ctrl Pts',(1.37381821967499,-1.,3.93912709041791));
#39113=CARTESIAN_POINT('Ctrl Pts',(1.37381821967499,1.,3.93912709041791));
#39114=CARTESIAN_POINT('Ctrl Pts',(1.37468482215784,-1.,3.93135106761941));
#39115=CARTESIAN_POINT('Ctrl Pts',(1.37468482215784,1.,3.93135106761941));
#39116=CARTESIAN_POINT('Ctrl Pts',(1.37551664448057,-1.,3.92357976987132));
#39117=CARTESIAN_POINT('Ctrl Pts',(1.37551664448057,1.,3.92357976987132));
#39118=CARTESIAN_POINT('Ctrl Pts',(1.37631350505516,-1.,3.91581337461825));
#39119=CARTESIAN_POINT('Ctrl Pts',(1.37631350505516,1.,3.91581337461825));
#39120=CARTESIAN_POINT('Ctrl Pts',(1.3770751963376,-1.,3.90805209522729));
#39121=CARTESIAN_POINT('Ctrl Pts',(1.3770751963376,1.,3.90805209522729));
#39122=CARTESIAN_POINT('Ctrl Pts',(1.3778014851263,-1.,3.90029615196255));
#39123=CARTESIAN_POINT('Ctrl Pts',(1.3778014851263,1.,3.90029615196255));
#39124=CARTESIAN_POINT('Ctrl Pts',(1.37849211287981,-1.,3.89254574338385));
#39125=CARTESIAN_POINT('Ctrl Pts',(1.37849211287981,1.,3.89254574338385));
#39126=CARTESIAN_POINT('Ctrl Pts',(1.37914679719446,-1.,3.88480102249461));
#39127=CARTESIAN_POINT('Ctrl Pts',(1.37914679719446,1.,3.88480102249461));
#39128=CARTESIAN_POINT('Ctrl Pts',(1.37976523097187,-1.,3.87706205830865));
#39129=CARTESIAN_POINT('Ctrl Pts',(1.37976523097187,1.,3.87706205830865));
#39130=CARTESIAN_POINT('Ctrl Pts',(1.38034709213129,-1.,3.86932885813403));
#39131=CARTESIAN_POINT('Ctrl Pts',(1.38034709213129,1.,3.86932885813403));
#39132=CARTESIAN_POINT('Ctrl Pts',(1.38089205993067,-1.,3.86160143044187));
#39133=CARTESIAN_POINT('Ctrl Pts',(1.38089205993067,1.,3.86160143044187));
#39134=CARTESIAN_POINT('Ctrl Pts',(1.38139983115075,-1.,3.85387983979557));
#39135=CARTESIAN_POINT('Ctrl Pts',(1.38139983115075,1.,3.85387983979557));
#39136=CARTESIAN_POINT('Ctrl Pts',(1.38187013346089,-1.,3.84616425605705));
#39137=CARTESIAN_POINT('Ctrl Pts',(1.38187013346089,1.,3.84616425605705));
#39138=CARTESIAN_POINT('Ctrl Pts',(1.38230274828774,-1.,3.83845502790609));
#39139=CARTESIAN_POINT('Ctrl Pts',(1.38230274828774,1.,3.83845502790609));
#39140=CARTESIAN_POINT('Ctrl Pts',(1.38269750245086,-1.,3.83075266982138));
#39141=CARTESIAN_POINT('Ctrl Pts',(1.38269750245086,1.,3.83075266982138));
#39142=CARTESIAN_POINT('Ctrl Pts',(1.38305421262724,-1.,3.82305771743715));
#39143=CARTESIAN_POINT('Ctrl Pts',(1.38305421262724,1.,3.82305771743715));
#39144=CARTESIAN_POINT('Ctrl Pts',(1.38337263902766,-1.,3.81537060817765));
#39145=CARTESIAN_POINT('Ctrl Pts',(1.38337263902766,1.,3.81537060817765));
#39146=CARTESIAN_POINT('Ctrl Pts',(1.38365244046226,-1.,3.80769156398429));
#39147=CARTESIAN_POINT('Ctrl Pts',(1.38365244046226,1.,3.80769156398429));
#39148=CARTESIAN_POINT('Ctrl Pts',(1.38389311766701,-1.,3.80002044322169));
#39149=CARTESIAN_POINT('Ctrl Pts',(1.38389311766701,1.,3.80002044322169));
#39150=CARTESIAN_POINT('Ctrl Pts',(1.38409399694588,-1.,3.79235669640907));
#39151=CARTESIAN_POINT('Ctrl Pts',(1.38409399694588,1.,3.79235669640907));
#39152=CARTESIAN_POINT('Ctrl Pts',(1.38425435883773,-1.,3.78469969805134));
#39153=CARTESIAN_POINT('Ctrl Pts',(1.38425435883773,1.,3.78469969805134));
#39154=CARTESIAN_POINT('Ctrl Pts',(1.38437354551435,-1.,3.77704902230441));
#39155=CARTESIAN_POINT('Ctrl Pts',(1.38437354551435,1.,3.77704902230441));
#39156=CARTESIAN_POINT('Ctrl Pts',(1.38445107339517,-1.,3.76940473185775));
#39157=CARTESIAN_POINT('Ctrl Pts',(1.38445107339517,1.,3.76940473185775));
#39158=CARTESIAN_POINT('Ctrl Pts',(1.38448675253343,-1.,3.76176768271347));
#39159=CARTESIAN_POINT('Ctrl Pts',(1.38448675253343,1.,3.76176768271347));
#39160=CARTESIAN_POINT('Ctrl Pts',(1.38448077997155,-1.,3.75413976318727));
#39161=CARTESIAN_POINT('Ctrl Pts',(1.38448077997155,1.,3.75413976318727));
#39162=CARTESIAN_POINT('Ctrl Pts',(1.38443344984389,-1.,3.7465231716786));
#39163=CARTESIAN_POINT('Ctrl Pts',(1.38443344984389,1.,3.7465231716786));
#39164=CARTESIAN_POINT('Ctrl Pts',(1.38434489156456,-1.,3.73891976418099));
#39165=CARTESIAN_POINT('Ctrl Pts',(1.38434489156456,1.,3.73891976418099));
#39166=CARTESIAN_POINT('Ctrl Pts',(1.38421479111531,-1.,3.73133035859283));
#39167=CARTESIAN_POINT('Ctrl Pts',(1.38421479111531,1.,3.73133035859283));
#39168=CARTESIAN_POINT('Ctrl Pts',(1.3840421342895,-1.,3.72375409358805));
#39169=CARTESIAN_POINT('Ctrl Pts',(1.3840421342895,1.,3.72375409358805));
#39170=CARTESIAN_POINT('Ctrl Pts',(1.38382489984585,-1.,3.7161876605181));
#39171=CARTESIAN_POINT('Ctrl Pts',(1.38382489984585,1.,3.7161876605181));
#39172=CARTESIAN_POINT('Ctrl Pts',(1.38356065402122,-1.,3.70862680753343));
#39173=CARTESIAN_POINT('Ctrl Pts',(1.38356065402122,1.,3.70862680753343));
#39174=CARTESIAN_POINT('Ctrl Pts',(1.38324717612862,-1.,3.70106792167894));
#39175=CARTESIAN_POINT('Ctrl Pts',(1.38324717612862,1.,3.70106792167894));
#39176=CARTESIAN_POINT('Ctrl Pts',(1.38288311171649,-1.,3.69350967899523));
#39177=CARTESIAN_POINT('Ctrl Pts',(1.38288311171649,1.,3.69350967899523));
#39178=CARTESIAN_POINT('Ctrl Pts',(1.38246852827185,-1.,3.68595444983844));
#39179=CARTESIAN_POINT('Ctrl Pts',(1.38246852827185,1.,3.68595444983844));
#39180=CARTESIAN_POINT('Ctrl Pts',(1.38200574290626,-1.,3.6784103848243));
#39181=CARTESIAN_POINT('Ctrl Pts',(1.38200574290626,1.,3.6784103848243));
#39182=CARTESIAN_POINT('Ctrl Pts',(1.38149812653876,-1.,3.67088843112282));
#39183=CARTESIAN_POINT('Ctrl Pts',(1.38149812653876,1.,3.67088843112282));
#39184=CARTESIAN_POINT('Ctrl Pts',(1.38094856333558,-1.,3.66339848520874));
#39185=CARTESIAN_POINT('Ctrl Pts',(1.38094856333558,1.,3.66339848520874));
#39186=CARTESIAN_POINT('Ctrl Pts',(1.38035791051215,-1.,3.65594554404396));
#39187=CARTESIAN_POINT('Ctrl Pts',(1.38035791051215,1.,3.65594554404396));
#39188=CARTESIAN_POINT('Ctrl Pts',(1.37972372481598,-1.,3.64852652756444));
#39189=CARTESIAN_POINT('Ctrl Pts',(1.37972372481598,1.,3.64852652756444));
#39190=CARTESIAN_POINT('Ctrl Pts',(1.37903818567347,-1.,3.64112507791112));
#39191=CARTESIAN_POINT('Ctrl Pts',(1.37903818567347,1.,3.64112507791112));
#39192=CARTESIAN_POINT('Ctrl Pts',(1.37829035457324,-1.,3.63371727442448));
#39193=CARTESIAN_POINT('Ctrl Pts',(1.37829035457324,1.,3.63371727442448));
#39194=CARTESIAN_POINT('Ctrl Pts',(1.37746987919868,-1.,3.62628098665112));
#39195=CARTESIAN_POINT('Ctrl Pts',(1.37746987919868,1.,3.62628098665112));
#39196=CARTESIAN_POINT('Ctrl Pts',(1.37657053403102,-1.,3.61880481160408));
#39197=CARTESIAN_POINT('Ctrl Pts',(1.37657053403102,1.,3.61880481160408));
#39198=CARTESIAN_POINT('Ctrl Pts',(1.37559314436641,-1.,3.61129546591082));
#39199=CARTESIAN_POINT('Ctrl Pts',(1.37559314436641,1.,3.61129546591082));
#39200=CARTESIAN_POINT('Ctrl Pts',(1.37455051379642,-1.,3.60379020124038));
#39201=CARTESIAN_POINT('Ctrl Pts',(1.37455051379642,1.,3.60379020124038));
#39202=CARTESIAN_POINT('Ctrl Pts',(1.37346320103184,-1.,3.59634627869117));
#39203=CARTESIAN_POINT('Ctrl Pts',(1.37346320103184,1.,3.59634627869117));
#39204=CARTESIAN_POINT('Ctrl Pts',(1.37235053661,-1.,3.5890185384643));
#39205=CARTESIAN_POINT('Ctrl Pts',(1.37235053661,1.,3.5890185384643));
#39206=CARTESIAN_POINT('Ctrl Pts',(1.37122241663073,-1.,3.58183885982745));
#39207=CARTESIAN_POINT('Ctrl Pts',(1.37122241663073,1.,3.58183885982745));
#39208=CARTESIAN_POINT('Ctrl Pts',(1.37007229485646,-1.,3.57479875549453));
#39209=CARTESIAN_POINT('Ctrl Pts',(1.37007229485646,1.,3.57479875549453));
#39210=CARTESIAN_POINT('Ctrl Pts',(1.36886584973349,-1.,3.56782080304554));
#39211=CARTESIAN_POINT('Ctrl Pts',(1.36886584973349,1.,3.56782080304554));
#39212=CARTESIAN_POINT('Ctrl Pts',(1.36754771771174,-1.,3.56077662028492));
#39213=CARTESIAN_POINT('Ctrl Pts',(1.36754771771174,1.,3.56077662028492));
#39214=CARTESIAN_POINT('Ctrl Pts',(1.36606145456711,-1.,3.55353883995793));
#39215=CARTESIAN_POINT('Ctrl Pts',(1.36606145456711,1.,3.55353883995793));
#39216=CARTESIAN_POINT('Ctrl Pts',(1.36436666257567,-1.,3.54602591832893));
#39217=CARTESIAN_POINT('Ctrl Pts',(1.36436666257567,1.,3.54602591832893));
#39218=CARTESIAN_POINT('Ctrl Pts',(1.36245507339334,-1.,3.53824396425032));
#39219=CARTESIAN_POINT('Ctrl Pts',(1.36245507339334,1.,3.53824396425032));
#39220=CARTESIAN_POINT('Ctrl Pts',(1.36037259643827,-1.,3.53034464961849));
#39221=CARTESIAN_POINT('Ctrl Pts',(1.36037259643827,1.,3.53034464961849));
#39222=CARTESIAN_POINT('Ctrl Pts',(1.35821701528975,-1.,3.52261776117121));
#39223=CARTESIAN_POINT('Ctrl Pts',(1.35821701528975,1.,3.52261776117121));
#39224=CARTESIAN_POINT('Ctrl Pts',(1.35611275237288,-1.,3.51542230699919));
#39225=CARTESIAN_POINT('Ctrl Pts',(1.35611275237288,1.,3.51542230699919));
#39226=CARTESIAN_POINT('Ctrl Pts',(1.35419113576022,-1.,3.50913227060177));
#39227=CARTESIAN_POINT('Ctrl Pts',(1.35419113576022,1.,3.50913227060177));
#39228=CARTESIAN_POINT('Ctrl Pts',(1.3525703284343,-1.,3.50408168106113));
#39229=CARTESIAN_POINT('Ctrl Pts',(1.3525703284343,1.,3.50408168106113));
#39230=CARTESIAN_POINT('Ctrl Pts',(1.35133076331065,-1.,3.50049707063673));
#39231=CARTESIAN_POINT('Ctrl Pts',(1.35133076331065,1.,3.50049707063673));
#39232=CARTESIAN_POINT('Ctrl Pts',(1.35067437417289,-1.,3.49888720256612));
#39233=CARTESIAN_POINT('Ctrl Pts',(1.35067437417289,1.,3.49888720256612));
#39234=CARTESIAN_POINT('Ctrl Pts',(1.35037650302887,-1.,3.49840357193384));
#39235=CARTESIAN_POINT('Ctrl Pts',(1.35037650302887,1.,3.49840357193384));
#39236=CARTESIAN_POINT('Ctrl Pts',(1.35026426118351,-1.,3.49840260053616));
#39237=CARTESIAN_POINT('Ctrl Pts',(1.35026426118351,1.,3.49840260053616));
#39238=CARTESIAN_POINT('Ctrl Pts',(1.35022972712301,-1.,3.49848248301936));
#39239=CARTESIAN_POINT('Ctrl Pts',(1.35022972712301,1.,3.49848248301936));
#39240=CARTESIAN_POINT('',(1.36999806084572,1.,3.97027773754922));
#39241=CARTESIAN_POINT('Ctrl Pts',(1.36999806084572,1.,3.97027773754922));
#39242=CARTESIAN_POINT('Ctrl Pts',(1.37020239094758,1.,3.9687184694173));
#39243=CARTESIAN_POINT('Ctrl Pts',(1.37060761746027,1.,3.96560037975788));
#39244=CARTESIAN_POINT('Ctrl Pts',(1.37120515615663,1.,3.96092458508407));
#39245=CARTESIAN_POINT('Ctrl Pts',(1.37198126433139,1.,3.95469287283105));
#39246=CARTESIAN_POINT('Ctrl Pts',(1.37291699203423,1.,3.94690771786926));
#39247=CARTESIAN_POINT('Ctrl Pts',(1.37381821967499,1.,3.93912709041791));
#39248=CARTESIAN_POINT('Ctrl Pts',(1.37468482215784,1.,3.93135106761941));
#39249=CARTESIAN_POINT('Ctrl Pts',(1.37551664448057,1.,3.92357976987132));
#39250=CARTESIAN_POINT('Ctrl Pts',(1.37631350505516,1.,3.91581337461825));
#39251=CARTESIAN_POINT('Ctrl Pts',(1.3770751963376,1.,3.90805209522729));
#39252=CARTESIAN_POINT('Ctrl Pts',(1.3778014851263,1.,3.90029615196255));
#39253=CARTESIAN_POINT('Ctrl Pts',(1.37849211287981,1.,3.89254574338385));
#39254=CARTESIAN_POINT('Ctrl Pts',(1.37914679719446,1.,3.88480102249461));
#39255=CARTESIAN_POINT('Ctrl Pts',(1.37976523097187,1.,3.87706205830865));
#39256=CARTESIAN_POINT('Ctrl Pts',(1.38034709213129,1.,3.86932885813403));
#39257=CARTESIAN_POINT('Ctrl Pts',(1.38089205993067,1.,3.86160143044187));
#39258=CARTESIAN_POINT('Ctrl Pts',(1.38139983115075,1.,3.85387983979557));
#39259=CARTESIAN_POINT('Ctrl Pts',(1.38187013346089,1.,3.84616425605705));
#39260=CARTESIAN_POINT('Ctrl Pts',(1.38230274828774,1.,3.83845502790609));
#39261=CARTESIAN_POINT('Ctrl Pts',(1.38269750245086,1.,3.83075266982138));
#39262=CARTESIAN_POINT('Ctrl Pts',(1.38305421262724,1.,3.82305771743715));
#39263=CARTESIAN_POINT('Ctrl Pts',(1.38337263902766,1.,3.81537060817765));
#39264=CARTESIAN_POINT('Ctrl Pts',(1.38365244046226,1.,3.80769156398429));
#39265=CARTESIAN_POINT('Ctrl Pts',(1.38389311766701,1.,3.80002044322169));
#39266=CARTESIAN_POINT('Ctrl Pts',(1.38409399694588,1.,3.79235669640907));
#39267=CARTESIAN_POINT('Ctrl Pts',(1.38425435883773,1.,3.78469969805134));
#39268=CARTESIAN_POINT('Ctrl Pts',(1.38437354551435,1.,3.77704902230441));
#39269=CARTESIAN_POINT('Ctrl Pts',(1.38445107339517,1.,3.76940473185775));
#39270=CARTESIAN_POINT('Ctrl Pts',(1.38448675253343,1.,3.76176768271347));
#39271=CARTESIAN_POINT('Ctrl Pts',(1.38448077997155,1.,3.75413976318727));
#39272=CARTESIAN_POINT('Ctrl Pts',(1.38443344984389,1.,3.7465231716786));
#39273=CARTESIAN_POINT('Ctrl Pts',(1.38434489156456,1.,3.73891976418099));
#39274=CARTESIAN_POINT('Ctrl Pts',(1.38421479111531,1.,3.73133035859283));
#39275=CARTESIAN_POINT('Ctrl Pts',(1.3840421342895,1.,3.72375409358805));
#39276=CARTESIAN_POINT('Ctrl Pts',(1.38382489984585,1.,3.7161876605181));
#39277=CARTESIAN_POINT('Ctrl Pts',(1.38356065402122,1.,3.70862680753343));
#39278=CARTESIAN_POINT('Ctrl Pts',(1.38324717612862,1.,3.70106792167894));
#39279=CARTESIAN_POINT('Ctrl Pts',(1.38288311171649,1.,3.69350967899523));
#39280=CARTESIAN_POINT('Ctrl Pts',(1.38246852827185,1.,3.68595444983844));
#39281=CARTESIAN_POINT('Ctrl Pts',(1.38200574290626,1.,3.6784103848243));
#39282=CARTESIAN_POINT('Ctrl Pts',(1.38149812653876,1.,3.67088843112282));
#39283=CARTESIAN_POINT('Ctrl Pts',(1.38094856333558,1.,3.66339848520874));
#39284=CARTESIAN_POINT('Ctrl Pts',(1.38035791051215,1.,3.65594554404396));
#39285=CARTESIAN_POINT('Ctrl Pts',(1.37972372481598,1.,3.64852652756444));
#39286=CARTESIAN_POINT('Ctrl Pts',(1.37903818567347,1.,3.64112507791112));
#39287=CARTESIAN_POINT('Ctrl Pts',(1.37829035457324,1.,3.63371727442448));
#39288=CARTESIAN_POINT('Ctrl Pts',(1.37746987919868,1.,3.62628098665112));
#39289=CARTESIAN_POINT('Ctrl Pts',(1.37657053403102,1.,3.61880481160408));
#39290=CARTESIAN_POINT('Ctrl Pts',(1.37559314436641,1.,3.61129546591082));
#39291=CARTESIAN_POINT('Ctrl Pts',(1.37455051379642,1.,3.60379020124038));
#39292=CARTESIAN_POINT('Ctrl Pts',(1.37346320103184,1.,3.59634627869117));
#39293=CARTESIAN_POINT('Ctrl Pts',(1.37235053661,1.,3.5890185384643));
#39294=CARTESIAN_POINT('Ctrl Pts',(1.37122241663073,1.,3.58183885982745));
#39295=CARTESIAN_POINT('Ctrl Pts',(1.37007229485646,1.,3.57479875549453));
#39296=CARTESIAN_POINT('Ctrl Pts',(1.36886584973349,1.,3.56782080304554));
#39297=CARTESIAN_POINT('Ctrl Pts',(1.36754771771174,1.,3.56077662028492));
#39298=CARTESIAN_POINT('Ctrl Pts',(1.36606145456711,1.,3.55353883995793));
#39299=CARTESIAN_POINT('Ctrl Pts',(1.36436666257567,1.,3.54602591832893));
#39300=CARTESIAN_POINT('Ctrl Pts',(1.36245507339334,1.,3.53824396425032));
#39301=CARTESIAN_POINT('Ctrl Pts',(1.36037259643827,1.,3.53034464961849));
#39302=CARTESIAN_POINT('Ctrl Pts',(1.35821701528975,1.,3.52261776117121));
#39303=CARTESIAN_POINT('Ctrl Pts',(1.35611275237288,1.,3.51542230699919));
#39304=CARTESIAN_POINT('Ctrl Pts',(1.35419113576022,1.,3.50913227060177));
#39305=CARTESIAN_POINT('Ctrl Pts',(1.3525703284343,1.,3.50408168106113));
#39306=CARTESIAN_POINT('Ctrl Pts',(1.35142377279535,1.,3.5007660381658));
#39307=CARTESIAN_POINT('Ctrl Pts',(1.35080045218652,1.,3.49920025459856));
#39308=CARTESIAN_POINT('Ctrl Pts',(1.35049736560633,1.,3.49861894124915));
#39309=CARTESIAN_POINT('Ctrl Pts',(1.35036670893102,1.,3.49847119623841));
#39310=CARTESIAN_POINT('Ctrl Pts',(1.35032489087269,1.,3.49844575334386));
#39311=CARTESIAN_POINT('',(1.36999806084572,0.,3.97027773754922));
#39312=CARTESIAN_POINT('Ctrl Pts',(0.96399761336957,-1.,3.62397690409552));
#39313=CARTESIAN_POINT('Ctrl Pts',(0.96399761336957,1.,3.62397690409552));
#39314=CARTESIAN_POINT('Ctrl Pts',(0.963922720982576,-1.,3.62393257642191));
#39315=CARTESIAN_POINT('Ctrl Pts',(0.963922720982576,1.,3.62393257642191));
#39316=CARTESIAN_POINT('Ctrl Pts',(0.963832486396055,-1.,3.62399933640277));
#39317=CARTESIAN_POINT('Ctrl Pts',(0.963832486396055,1.,3.62399933640277));
#39318=CARTESIAN_POINT('Ctrl Pts',(0.963875774532102,-1.,3.62456568607055));
#39319=CARTESIAN_POINT('Ctrl Pts',(0.963875774532102,1.,3.62456568607055));
#39320=CARTESIAN_POINT('Ctrl Pts',(0.964291001274618,-1.,3.62625391255277));
#39321=CARTESIAN_POINT('Ctrl Pts',(0.964291001274618,1.,3.62625391255277));
#39322=CARTESIAN_POINT('Ctrl Pts',(0.965395153165715,-1.,3.62988252139998));
#39323=CARTESIAN_POINT('Ctrl Pts',(0.965395153165715,1.,3.62988252139998));
#39324=CARTESIAN_POINT('Ctrl Pts',(0.967052554540877,-1.,3.6349212208096));
#39325=CARTESIAN_POINT('Ctrl Pts',(0.967052554540877,1.,3.6349212208096));
#39326=CARTESIAN_POINT('Ctrl Pts',(0.969195124674828,-1.,3.64113946505393));
#39327=CARTESIAN_POINT('Ctrl Pts',(0.969195124674828,1.,3.64113946505393));
#39328=CARTESIAN_POINT('Ctrl Pts',(0.971722122060277,-1.,3.64819756447072));
#39329=CARTESIAN_POINT('Ctrl Pts',(0.971722122060277,1.,3.64819756447072));
#39330=CARTESIAN_POINT('Ctrl Pts',(0.974519971354138,-1.,3.6557157673487));
#39331=CARTESIAN_POINT('Ctrl Pts',(0.974519971354138,1.,3.6557157673487));
#39332=CARTESIAN_POINT('Ctrl Pts',(0.977478312751416,-1.,3.66333049637403));
#39333=CARTESIAN_POINT('Ctrl Pts',(0.977478312751416,1.,3.66333049637403));
#39334=CARTESIAN_POINT('Ctrl Pts',(0.980505922458494,-1.,3.67074983340444));
#39335=CARTESIAN_POINT('Ctrl Pts',(0.980505922458494,1.,3.67074983340444));
#39336=CARTESIAN_POINT('Ctrl Pts',(0.983550791470864,-1.,3.67782408841876));
#39337=CARTESIAN_POINT('Ctrl Pts',(0.983550791470864,1.,3.67782408841876));
#39338=CARTESIAN_POINT('Ctrl Pts',(0.986602639864285,-1.,3.6845531792623));
#39339=CARTESIAN_POINT('Ctrl Pts',(0.986602639864285,1.,3.6845531792623));
#39340=CARTESIAN_POINT('Ctrl Pts',(0.989676715398858,-1.,3.69102682138955));
#39341=CARTESIAN_POINT('Ctrl Pts',(0.989676715398858,1.,3.69102682138955));
#39342=CARTESIAN_POINT('Ctrl Pts',(0.992802218332103,-1.,3.69738123415696));
#39343=CARTESIAN_POINT('Ctrl Pts',(0.992802218332103,1.,3.69738123415696));
#39344=CARTESIAN_POINT('Ctrl Pts',(0.996009819772431,-1.,3.70375282282107));
#39345=CARTESIAN_POINT('Ctrl Pts',(0.996009819772431,1.,3.70375282282107));
#39346=CARTESIAN_POINT('Ctrl Pts',(0.999317260756344,-1.,3.7102243971387));
#39347=CARTESIAN_POINT('Ctrl Pts',(0.999317260756344,1.,3.7102243971387));
#39348=CARTESIAN_POINT('Ctrl Pts',(1.00272423396802,-1.,3.71680667125047));
#39349=CARTESIAN_POINT('Ctrl Pts',(1.00272423396802,1.,3.71680667125047));
#39350=CARTESIAN_POINT('Ctrl Pts',(1.00622000735696,-1.,3.72346803750544));
#39351=CARTESIAN_POINT('Ctrl Pts',(1.00622000735696,1.,3.72346803750544));
#39352=CARTESIAN_POINT('Ctrl Pts',(1.00978798539491,-1.,3.73015276704407));
#39353=CARTESIAN_POINT('Ctrl Pts',(1.00978798539491,1.,3.73015276704407));
#39354=CARTESIAN_POINT('Ctrl Pts',(1.01341114319906,-1.,3.73680245055747));
#39355=CARTESIAN_POINT('Ctrl Pts',(1.01341114319906,1.,3.73680245055747));
#39356=CARTESIAN_POINT('Ctrl Pts',(1.01707794311088,-1.,3.74337942504993));
#39357=CARTESIAN_POINT('Ctrl Pts',(1.01707794311088,1.,3.74337942504993));
#39358=CARTESIAN_POINT('Ctrl Pts',(1.02078510487439,-1.,3.74987777155873));
#39359=CARTESIAN_POINT('Ctrl Pts',(1.02078510487439,1.,3.74987777155873));
#39360=CARTESIAN_POINT('Ctrl Pts',(1.02453429444668,-1.,3.75631037456224));
#39361=CARTESIAN_POINT('Ctrl Pts',(1.02453429444668,1.,3.75631037456224));
#39362=CARTESIAN_POINT('Ctrl Pts',(1.02833014458184,-1.,3.76270122291245));
#39363=CARTESIAN_POINT('Ctrl Pts',(1.02833014458184,1.,3.76270122291245));
#39364=CARTESIAN_POINT('Ctrl Pts',(1.03217786604919,-1.,3.76907609832516));
#39365=CARTESIAN_POINT('Ctrl Pts',(1.03217786604919,1.,3.76907609832516));
#39366=CARTESIAN_POINT('Ctrl Pts',(1.03608074678008,-1.,3.77545283140427));
#39367=CARTESIAN_POINT('Ctrl Pts',(1.03608074678008,1.,3.77545283140427));
#39368=CARTESIAN_POINT('Ctrl Pts',(1.04003862055798,-1.,3.7818353500817));
#39369=CARTESIAN_POINT('Ctrl Pts',(1.04003862055798,1.,3.7818353500817));
#39370=CARTESIAN_POINT('Ctrl Pts',(1.04404924374422,-1.,3.78821910787179));
#39371=CARTESIAN_POINT('Ctrl Pts',(1.04404924374422,1.,3.78821910787179));
#39372=CARTESIAN_POINT('Ctrl Pts',(1.04810913267639,-1.,3.79459440308786));
#39373=CARTESIAN_POINT('Ctrl Pts',(1.04810913267639,1.,3.79459440308786));
#39374=CARTESIAN_POINT('Ctrl Pts',(1.05221457990016,-1.,3.80095039790681));
#39375=CARTESIAN_POINT('Ctrl Pts',(1.05221457990016,1.,3.80095039790681));
#39376=CARTESIAN_POINT('Ctrl Pts',(1.05636266918644,-1.,3.80727913637791));
#39377=CARTESIAN_POINT('Ctrl Pts',(1.05636266918644,1.,3.80727913637791));
#39378=CARTESIAN_POINT('Ctrl Pts',(1.06055206187299,-1.,3.8135786611749));
#39379=CARTESIAN_POINT('Ctrl Pts',(1.06055206187299,1.,3.8135786611749));
#39380=CARTESIAN_POINT('Ctrl Pts',(1.0647824403893,-1.,3.81985083953012));
#39381=CARTESIAN_POINT('Ctrl Pts',(1.0647824403893,1.,3.81985083953012));
#39382=CARTESIAN_POINT('Ctrl Pts',(1.06905413180359,-1.,3.82609989967276));
#39383=CARTESIAN_POINT('Ctrl Pts',(1.06905413180359,1.,3.82609989967276));
#39384=CARTESIAN_POINT('Ctrl Pts',(1.07336766633459,-1.,3.83233071195144));
#39385=CARTESIAN_POINT('Ctrl Pts',(1.07336766633459,1.,3.83233071195144));
#39386=CARTESIAN_POINT('Ctrl Pts',(1.07772335353858,-1.,3.83854714117491));
#39387=CARTESIAN_POINT('Ctrl Pts',(1.07772335353858,1.,3.83854714117491));
#39388=CARTESIAN_POINT('Ctrl Pts',(1.08212087917991,-1.,3.8447504803063));
#39389=CARTESIAN_POINT('Ctrl Pts',(1.08212087917991,1.,3.8447504803063));
#39390=CARTESIAN_POINT('Ctrl Pts',(1.08655950846384,-1.,3.85094025222713));
#39391=CARTESIAN_POINT('Ctrl Pts',(1.08655950846384,1.,3.85094025222713));
#39392=CARTESIAN_POINT('Ctrl Pts',(1.09103825516294,-1.,3.85711487933931));
#39393=CARTESIAN_POINT('Ctrl Pts',(1.09103825516294,1.,3.85711487933931));
#39394=CARTESIAN_POINT('Ctrl Pts',(1.09555606505013,-1.,3.86327241021247));
#39395=CARTESIAN_POINT('Ctrl Pts',(1.09555606505013,1.,3.86327241021247));
#39396=CARTESIAN_POINT('Ctrl Pts',(1.10011198761195,-1.,3.86941120134849));
#39397=CARTESIAN_POINT('Ctrl Pts',(1.10011198761195,1.,3.86941120134849));
#39398=CARTESIAN_POINT('Ctrl Pts',(1.10470536603287,-1.,3.87553067187514));
#39399=CARTESIAN_POINT('Ctrl Pts',(1.10470536603287,1.,3.87553067187514));
#39400=CARTESIAN_POINT('Ctrl Pts',(1.10933577224008,-1.,3.88163105531724));
#39401=CARTESIAN_POINT('Ctrl Pts',(1.10933577224008,1.,3.88163105531724));
#39402=CARTESIAN_POINT('Ctrl Pts',(1.11400292434429,-1.,3.88771308285171));
#39403=CARTESIAN_POINT('Ctrl Pts',(1.11400292434429,1.,3.88771308285171));
#39404=CARTESIAN_POINT('Ctrl Pts',(1.11870660794603,-1.,3.89377768340344));
#39405=CARTESIAN_POINT('Ctrl Pts',(1.11870660794603,1.,3.89377768340344));
#39406=CARTESIAN_POINT('Ctrl Pts',(1.12344660099043,-1.,3.89982569750025));
#39407=CARTESIAN_POINT('Ctrl Pts',(1.12344660099043,1.,3.89982569750025));
#39408=CARTESIAN_POINT('Ctrl Pts',(1.12822258281553,-1.,3.90585753318737));
#39409=CARTESIAN_POINT('Ctrl Pts',(1.12822258281553,1.,3.90585753318737));
#39410=CARTESIAN_POINT('Ctrl Pts',(1.13303414693896,-1.,3.91187321145649));
#39411=CARTESIAN_POINT('Ctrl Pts',(1.13303414693896,1.,3.91187321145649));
#39412=CARTESIAN_POINT('Ctrl Pts',(1.13788084225554,-1.,3.91787251936827));
#39413=CARTESIAN_POINT('Ctrl Pts',(1.13788084225554,1.,3.91787251936827));
#39414=CARTESIAN_POINT('Ctrl Pts',(1.14276220561593,-1.,3.92385513133997));
#39415=CARTESIAN_POINT('Ctrl Pts',(1.14276220561593,1.,3.92385513133997));
#39416=CARTESIAN_POINT('Ctrl Pts',(1.14767779451123,-1.,3.92982073294257));
#39417=CARTESIAN_POINT('Ctrl Pts',(1.14767779451123,1.,3.92982073294257));
#39418=CARTESIAN_POINT('Ctrl Pts',(1.1526272271632,-1.,3.9357691705628));
#39419=CARTESIAN_POINT('Ctrl Pts',(1.1526272271632,1.,3.9357691705628));
#39420=CARTESIAN_POINT('Ctrl Pts',(1.15761018340956,-1.,3.94170046685203));
#39421=CARTESIAN_POINT('Ctrl Pts',(1.15761018340956,1.,3.94170046685203));
#39422=CARTESIAN_POINT('Ctrl Pts',(1.16262637999157,-1.,3.94761474780583));
#39423=CARTESIAN_POINT('Ctrl Pts',(1.16262637999157,1.,3.94761474780583));
#39424=CARTESIAN_POINT('Ctrl Pts',(1.16767555244438,-1.,3.95351219509876));
#39425=CARTESIAN_POINT('Ctrl Pts',(1.16767555244438,1.,3.95351219509876));
#39426=CARTESIAN_POINT('Ctrl Pts',(1.17275743590361,-1.,3.95939299213276));
#39427=CARTESIAN_POINT('Ctrl Pts',(1.17275743590361,1.,3.95939299213276));
#39428=CARTESIAN_POINT('Ctrl Pts',(1.17787174135592,-1.,3.96525726358159));
#39429=CARTESIAN_POINT('Ctrl Pts',(1.17787174135592,1.,3.96525726358159));
#39430=CARTESIAN_POINT('Ctrl Pts',(1.18301815039831,-1.,3.97110505165415));
#39431=CARTESIAN_POINT('Ctrl Pts',(1.18301815039831,1.,3.97110505165415));
#39432=CARTESIAN_POINT('Ctrl Pts',(1.18819633715539,-1.,3.97693634767754));
#39433=CARTESIAN_POINT('Ctrl Pts',(1.18819633715539,1.,3.97693634767754));
#39434=CARTESIAN_POINT('Ctrl Pts',(1.19340598349475,-1.,3.98275111052561));
#39435=CARTESIAN_POINT('Ctrl Pts',(1.19340598349475,1.,3.98275111052561));
#39436=CARTESIAN_POINT('Ctrl Pts',(1.19864679609566,-1.,3.98854928957189));
#39437=CARTESIAN_POINT('Ctrl Pts',(1.19864679609566,1.,3.98854928957189));
#39438=CARTESIAN_POINT('Ctrl Pts',(1.20391852375138,-1.,3.99433084799666));
#39439=CARTESIAN_POINT('Ctrl Pts',(1.20391852375138,1.,3.99433084799666));
#39440=CARTESIAN_POINT('Ctrl Pts',(1.20922097029551,-1.,4.00009577950721));
#39441=CARTESIAN_POINT('Ctrl Pts',(1.20922097029551,1.,4.00009577950721));
#39442=CARTESIAN_POINT('Ctrl Pts',(1.21455398918133,-1.,4.00584409522722));
#39443=CARTESIAN_POINT('Ctrl Pts',(1.21455398918133,1.,4.00584409522722));
#39444=CARTESIAN_POINT('Ctrl Pts',(1.21884478244403,-1.,4.01042947140789));
#39445=CARTESIAN_POINT('Ctrl Pts',(1.21884478244403,1.,4.01042947140789));
#39446=CARTESIAN_POINT('Ctrl Pts',(1.22207656455845,-1.,4.01386104433519));
#39447=CARTESIAN_POINT('Ctrl Pts',(1.22207656455845,1.,4.01386104433519));
#39448=CARTESIAN_POINT('Ctrl Pts',(1.22423716681317,-1.,4.01614544569895));
#39449=CARTESIAN_POINT('Ctrl Pts',(1.22423716681317,1.,4.01614544569895));
#39450=CARTESIAN_POINT('Ctrl Pts',(1.22531898815164,-1.,4.01728681790024));
#39451=CARTESIAN_POINT('Ctrl Pts',(1.22531898815164,1.,4.01728681790024));
#39452=CARTESIAN_POINT('',(0.963899035118985,1.,3.62400312501199));
#39453=CARTESIAN_POINT('Ctrl Pts',(0.963899035118985,-1.,3.62400312501199));
#39454=CARTESIAN_POINT('Ctrl Pts',(0.963899035118985,-0.666666666666667,
3.62400312501199));
#39455=CARTESIAN_POINT('Ctrl Pts',(0.963899035118985,-0.333333333333333,
3.62400312501199));
#39456=CARTESIAN_POINT('Ctrl Pts',(0.963899035118985,0.333333333333333,
3.62400312501199));
#39457=CARTESIAN_POINT('Ctrl Pts',(0.963899035118985,0.666666666666667,
3.62400312501199));
#39458=CARTESIAN_POINT('Ctrl Pts',(0.963899035118985,1.,3.62400312501199));
#39459=CARTESIAN_POINT('',(1.22531898815164,1.,4.01728681790024));
#39460=CARTESIAN_POINT('',(1.22531898815164,0.,4.01728681790024));
#39461=CARTESIAN_POINT('Ctrl Pts',(0.963899035118985,1.,3.62400312501199));
#39462=CARTESIAN_POINT('Ctrl Pts',(0.963880158556712,1.,3.62404828878375));
#39463=CARTESIAN_POINT('Ctrl Pts',(0.963861297423578,1.,3.62424461507455));
#39464=CARTESIAN_POINT('Ctrl Pts',(0.963957782642589,1.,3.62489305727516));
#39465=CARTESIAN_POINT('Ctrl Pts',(0.964373850166081,1.,3.62652618145252));
#39466=CARTESIAN_POINT('Ctrl Pts',(0.965395153165715,1.,3.62988252139998));
#39467=CARTESIAN_POINT('Ctrl Pts',(0.967052554540877,1.,3.6349212208096));
#39468=CARTESIAN_POINT('Ctrl Pts',(0.969195124674828,1.,3.64113946505393));
#39469=CARTESIAN_POINT('Ctrl Pts',(0.971722122060277,1.,3.64819756447072));
#39470=CARTESIAN_POINT('Ctrl Pts',(0.974519971354138,1.,3.6557157673487));
#39471=CARTESIAN_POINT('Ctrl Pts',(0.977478312751416,1.,3.66333049637403));
#39472=CARTESIAN_POINT('Ctrl Pts',(0.980505922458494,1.,3.67074983340444));
#39473=CARTESIAN_POINT('Ctrl Pts',(0.983550791470864,1.,3.67782408841876));
#39474=CARTESIAN_POINT('Ctrl Pts',(0.986602639864285,1.,3.6845531792623));
#39475=CARTESIAN_POINT('Ctrl Pts',(0.989676715398858,1.,3.69102682138955));
#39476=CARTESIAN_POINT('Ctrl Pts',(0.992802218332103,1.,3.69738123415696));
#39477=CARTESIAN_POINT('Ctrl Pts',(0.996009819772431,1.,3.70375282282107));
#39478=CARTESIAN_POINT('Ctrl Pts',(0.999317260756344,1.,3.7102243971387));
#39479=CARTESIAN_POINT('Ctrl Pts',(1.00272423396802,1.,3.71680667125047));
#39480=CARTESIAN_POINT('Ctrl Pts',(1.00622000735696,1.,3.72346803750544));
#39481=CARTESIAN_POINT('Ctrl Pts',(1.00978798539491,1.,3.73015276704407));
#39482=CARTESIAN_POINT('Ctrl Pts',(1.01341114319906,1.,3.73680245055747));
#39483=CARTESIAN_POINT('Ctrl Pts',(1.01707794311088,1.,3.74337942504993));
#39484=CARTESIAN_POINT('Ctrl Pts',(1.02078510487439,1.,3.74987777155873));
#39485=CARTESIAN_POINT('Ctrl Pts',(1.02453429444668,1.,3.75631037456224));
#39486=CARTESIAN_POINT('Ctrl Pts',(1.02833014458184,1.,3.76270122291245));
#39487=CARTESIAN_POINT('Ctrl Pts',(1.03217786604919,1.,3.76907609832516));
#39488=CARTESIAN_POINT('Ctrl Pts',(1.03608074678008,1.,3.77545283140427));
#39489=CARTESIAN_POINT('Ctrl Pts',(1.04003862055798,1.,3.7818353500817));
#39490=CARTESIAN_POINT('Ctrl Pts',(1.04404924374422,1.,3.78821910787179));
#39491=CARTESIAN_POINT('Ctrl Pts',(1.04810913267639,1.,3.79459440308786));
#39492=CARTESIAN_POINT('Ctrl Pts',(1.05221457990016,1.,3.80095039790681));
#39493=CARTESIAN_POINT('Ctrl Pts',(1.05636266918644,1.,3.80727913637791));
#39494=CARTESIAN_POINT('Ctrl Pts',(1.06055206187299,1.,3.8135786611749));
#39495=CARTESIAN_POINT('Ctrl Pts',(1.0647824403893,1.,3.81985083953012));
#39496=CARTESIAN_POINT('Ctrl Pts',(1.06905413180359,1.,3.82609989967276));
#39497=CARTESIAN_POINT('Ctrl Pts',(1.07336766633459,1.,3.83233071195144));
#39498=CARTESIAN_POINT('Ctrl Pts',(1.07772335353858,1.,3.83854714117491));
#39499=CARTESIAN_POINT('Ctrl Pts',(1.08212087917991,1.,3.8447504803063));
#39500=CARTESIAN_POINT('Ctrl Pts',(1.08655950846384,1.,3.85094025222713));
#39501=CARTESIAN_POINT('Ctrl Pts',(1.09103825516294,1.,3.85711487933931));
#39502=CARTESIAN_POINT('Ctrl Pts',(1.09555606505013,1.,3.86327241021247));
#39503=CARTESIAN_POINT('Ctrl Pts',(1.10011198761195,1.,3.86941120134849));
#39504=CARTESIAN_POINT('Ctrl Pts',(1.10470536603287,1.,3.87553067187514));
#39505=CARTESIAN_POINT('Ctrl Pts',(1.10933577224008,1.,3.88163105531724));
#39506=CARTESIAN_POINT('Ctrl Pts',(1.11400292434429,1.,3.88771308285171));
#39507=CARTESIAN_POINT('Ctrl Pts',(1.11870660794603,1.,3.89377768340344));
#39508=CARTESIAN_POINT('Ctrl Pts',(1.12344660099043,1.,3.89982569750025));
#39509=CARTESIAN_POINT('Ctrl Pts',(1.12822258281553,1.,3.90585753318737));
#39510=CARTESIAN_POINT('Ctrl Pts',(1.13303414693896,1.,3.91187321145649));
#39511=CARTESIAN_POINT('Ctrl Pts',(1.13788084225554,1.,3.91787251936827));
#39512=CARTESIAN_POINT('Ctrl Pts',(1.14276220561593,1.,3.92385513133997));
#39513=CARTESIAN_POINT('Ctrl Pts',(1.14767779451123,1.,3.92982073294257));
#39514=CARTESIAN_POINT('Ctrl Pts',(1.1526272271632,1.,3.9357691705628));
#39515=CARTESIAN_POINT('Ctrl Pts',(1.15761018340956,1.,3.94170046685203));
#39516=CARTESIAN_POINT('Ctrl Pts',(1.16262637999157,1.,3.94761474780583));
#39517=CARTESIAN_POINT('Ctrl Pts',(1.16767555244438,1.,3.95351219509876));
#39518=CARTESIAN_POINT('Ctrl Pts',(1.17275743590361,1.,3.95939299213276));
#39519=CARTESIAN_POINT('Ctrl Pts',(1.17787174135592,1.,3.96525726358159));
#39520=CARTESIAN_POINT('Ctrl Pts',(1.18301815039831,1.,3.97110505165415));
#39521=CARTESIAN_POINT('Ctrl Pts',(1.18819633715539,1.,3.97693634767754));
#39522=CARTESIAN_POINT('Ctrl Pts',(1.19340598349475,1.,3.98275111052561));
#39523=CARTESIAN_POINT('Ctrl Pts',(1.19864679609566,1.,3.98854928957189));
#39524=CARTESIAN_POINT('Ctrl Pts',(1.20391852375138,1.,3.99433084799666));
#39525=CARTESIAN_POINT('Ctrl Pts',(1.20922097029551,1.,4.00009577950721));
#39526=CARTESIAN_POINT('Ctrl Pts',(1.21455398918133,1.,4.00584409522722));
#39527=CARTESIAN_POINT('Ctrl Pts',(1.21884478244403,1.,4.01042947140789));
#39528=CARTESIAN_POINT('Ctrl Pts',(1.22207656455845,1.,4.01386104433519));
#39529=CARTESIAN_POINT('Ctrl Pts',(1.22423716681317,1.,4.01614544569895));
#39530=CARTESIAN_POINT('Ctrl Pts',(1.22531898815164,1.,4.01728681790024));
#39531=CARTESIAN_POINT('Origin',(1.22531898815164,0.,4.01728681790024));
#39532=CARTESIAN_POINT('',(1.36999806084572,1.,3.97027773754922));
#39533=CARTESIAN_POINT('Origin',(0.,0.,0.));
#39534=CARTESIAN_POINT('',(0.786422660833742,1.,3.66661143271648));
#39535=CARTESIAN_POINT('Origin',(0.,1.,0.));
#39536=CARTESIAN_POINT('Ctrl Pts',(0.786422660833742,1.,3.66661143271648));
#39537=CARTESIAN_POINT('Ctrl Pts',(0.786422660833742,0.666666666666667,
3.66661143271648));
#39538=CARTESIAN_POINT('Ctrl Pts',(0.786422660833742,0.333333333333333,
3.66661143271648));
#39539=CARTESIAN_POINT('Ctrl Pts',(0.786422660833742,-0.333333333333333,
3.66661143271648));
#39540=CARTESIAN_POINT('Ctrl Pts',(0.786422660833742,-0.666666666666667,
3.66661143271648));
#39541=CARTESIAN_POINT('Ctrl Pts',(0.786422660833742,-1.,3.66661143271648));
#39542=CARTESIAN_POINT('Ctrl Pts',(0.732042837400619,-1.,4.13571194405636));
#39543=CARTESIAN_POINT('Ctrl Pts',(0.732042837400619,1.,4.13571194405636));
#39544=CARTESIAN_POINT('Ctrl Pts',(0.732488575135925,-1.,4.13420383737278));
#39545=CARTESIAN_POINT('Ctrl Pts',(0.732488575135925,1.,4.13420383737278));
#39546=CARTESIAN_POINT('Ctrl Pts',(0.733376589325634,-1.,4.13118752796397));
#39547=CARTESIAN_POINT('Ctrl Pts',(0.733376589325634,1.,4.13118752796397));
#39548=CARTESIAN_POINT('Ctrl Pts',(0.734698226767512,-1.,4.12666277572794));
#39549=CARTESIAN_POINT('Ctrl Pts',(0.734698226767512,1.,4.12666277572794));
#39550=CARTESIAN_POINT('Ctrl Pts',(0.736439634335347,-1.,4.12062919626082));
#39551=CARTESIAN_POINT('Ctrl Pts',(0.736439634335347,1.,4.12062919626082));
#39552=CARTESIAN_POINT('Ctrl Pts',(0.738581708229118,-1.,4.11308626953795));
#39553=CARTESIAN_POINT('Ctrl Pts',(0.738581708229118,1.,4.11308626953795));
#39554=CARTESIAN_POINT('Ctrl Pts',(0.740688998555151,-1.,4.1055424175856));
#39555=CARTESIAN_POINT('Ctrl Pts',(0.740688998555151,1.,4.1055424175856));
#39556=CARTESIAN_POINT('Ctrl Pts',(0.742761369690017,-1.,4.09799769702712));
#39557=CARTESIAN_POINT('Ctrl Pts',(0.742761369690017,1.,4.09799769702712));
#39558=CARTESIAN_POINT('Ctrl Pts',(0.744798649705513,-1.,4.09045220253011));
#39559=CARTESIAN_POINT('Ctrl Pts',(0.744798649705513,1.,4.09045220253011));
#39560=CARTESIAN_POINT('Ctrl Pts',(0.746800631490821,-1.,4.08290608094789));
#39561=CARTESIAN_POINT('Ctrl Pts',(0.746800631490821,1.,4.08290608094789));
#39562=CARTESIAN_POINT('Ctrl Pts',(0.748767076679176,-1.,4.07535951055363));
#39563=CARTESIAN_POINT('Ctrl Pts',(0.748767076679176,1.,4.07535951055363));
#39564=CARTESIAN_POINT('Ctrl Pts',(0.750697720483175,-1.,4.06781267241886));
#39565=CARTESIAN_POINT('Ctrl Pts',(0.750697720483175,1.,4.06781267241886));
#39566=CARTESIAN_POINT('Ctrl Pts',(0.752592276482868,-1.,4.06026572221399));
#39567=CARTESIAN_POINT('Ctrl Pts',(0.752592276482868,1.,4.06026572221399));
#39568=CARTESIAN_POINT('Ctrl Pts',(0.754450441816411,-1.,4.05271876688106));
#39569=CARTESIAN_POINT('Ctrl Pts',(0.754450441816411,1.,4.05271876688106));
#39570=CARTESIAN_POINT('Ctrl Pts',(0.756271902370186,-1.,4.04517182654344));
#39571=CARTESIAN_POINT('Ctrl Pts',(0.756271902370186,1.,4.04517182654344));
#39572=CARTESIAN_POINT('Ctrl Pts',(0.758056338885553,-1.,4.03762485803468));
#39573=CARTESIAN_POINT('Ctrl Pts',(0.758056338885553,1.,4.03762485803468));
#39574=CARTESIAN_POINT('Ctrl Pts',(0.759803433244165,-1.,4.0300778195465));
#39575=CARTESIAN_POINT('Ctrl Pts',(0.759803433244165,1.,4.0300778195465));
#39576=CARTESIAN_POINT('Ctrl Pts',(0.761512875859941,-1.,4.02253072741347));
#39577=CARTESIAN_POINT('Ctrl Pts',(0.761512875859941,1.,4.02253072741347));
#39578=CARTESIAN_POINT('Ctrl Pts',(0.763184371182826,-1.,4.01498370680434));
#39579=CARTESIAN_POINT('Ctrl Pts',(0.763184371182826,1.,4.01498370680434));
#39580=CARTESIAN_POINT('Ctrl Pts',(0.764817648784946,-1.,4.00743706791366));
#39581=CARTESIAN_POINT('Ctrl Pts',(0.764817648784946,1.,4.00743706791366));
#39582=CARTESIAN_POINT('Ctrl Pts',(0.766412457135785,-1.,3.99989129179464));
#39583=CARTESIAN_POINT('Ctrl Pts',(0.766412457135785,1.,3.99989129179464));
#39584=CARTESIAN_POINT('Ctrl Pts',(0.767968531377707,-1.,3.99234687880892));
#39585=CARTESIAN_POINT('Ctrl Pts',(0.767968531377707,1.,3.99234687880892));
#39586=CARTESIAN_POINT('Ctrl Pts',(0.769485566245459,-1.,3.98480422348403));
#39587=CARTESIAN_POINT('Ctrl Pts',(0.769485566245459,1.,3.98480422348403));
#39588=CARTESIAN_POINT('Ctrl Pts',(0.770963190030503,-1.,3.97726349165507));
#39589=CARTESIAN_POINT('Ctrl Pts',(0.770963190030503,1.,3.97726349165507));
#39590=CARTESIAN_POINT('Ctrl Pts',(0.772400931772238,-1.,3.96972446532832));
#39591=CARTESIAN_POINT('Ctrl Pts',(0.772400931772238,1.,3.96972446532832));
#39592=CARTESIAN_POINT('Ctrl Pts',(0.773798212026682,-1.,3.96218649639876));
#39593=CARTESIAN_POINT('Ctrl Pts',(0.773798212026682,1.,3.96218649639876));
#39594=CARTESIAN_POINT('Ctrl Pts',(0.775154418039441,-1.,3.95464885452364));
#39595=CARTESIAN_POINT('Ctrl Pts',(0.775154418039441,1.,3.95464885452364));
#39596=CARTESIAN_POINT('Ctrl Pts',(0.776468966697959,-1.,3.94711101619471));
#39597=CARTESIAN_POINT('Ctrl Pts',(0.776468966697959,1.,3.94711101619471));
#39598=CARTESIAN_POINT('Ctrl Pts',(0.777741370568549,-1.,3.93957296768098));
#39599=CARTESIAN_POINT('Ctrl Pts',(0.777741370568549,1.,3.93957296768098));
#39600=CARTESIAN_POINT('Ctrl Pts',(0.778971308134786,-1.,3.93203552473153));
#39601=CARTESIAN_POINT('Ctrl Pts',(0.778971308134786,1.,3.93203552473153));
#39602=CARTESIAN_POINT('Ctrl Pts',(0.780158678615506,-1.,3.92450058323799));
#39603=CARTESIAN_POINT('Ctrl Pts',(0.780158678615506,1.,3.92450058323799));
#39604=CARTESIAN_POINT('Ctrl Pts',(0.781303428618343,-1.,3.9169703605466));
#39605=CARTESIAN_POINT('Ctrl Pts',(0.781303428618343,1.,3.9169703605466));
#39606=CARTESIAN_POINT('Ctrl Pts',(0.782405395622758,-1.,3.90944671004536));
#39607=CARTESIAN_POINT('Ctrl Pts',(0.782405395622758,1.,3.90944671004536));
#39608=CARTESIAN_POINT('Ctrl Pts',(0.783464141529082,-1.,3.90193039043971));
#39609=CARTESIAN_POINT('Ctrl Pts',(0.783464141529082,1.,3.90193039043971));
#39610=CARTESIAN_POINT('Ctrl Pts',(0.784478799358335,-1.,3.89442039235105));
#39611=CARTESIAN_POINT('Ctrl Pts',(0.784478799358335,1.,3.89442039235105));
#39612=CARTESIAN_POINT('Ctrl Pts',(0.785447890340723,-1.,3.88691313167399));
#39613=CARTESIAN_POINT('Ctrl Pts',(0.785447890340723,1.,3.88691313167399));
#39614=CARTESIAN_POINT('Ctrl Pts',(0.786369675812591,-1.,3.87940402818186));
#39615=CARTESIAN_POINT('Ctrl Pts',(0.786369675812591,1.,3.87940402818186));
#39616=CARTESIAN_POINT('Ctrl Pts',(0.78724252761798,-1.,3.87188916600905));
#39617=CARTESIAN_POINT('Ctrl Pts',(0.78724252761798,1.,3.87188916600905));
#39618=CARTESIAN_POINT('Ctrl Pts',(0.78806531509377,-1.,3.86436702561342));
#39619=CARTESIAN_POINT('Ctrl Pts',(0.78806531509377,1.,3.86436702561342));
#39620=CARTESIAN_POINT('Ctrl Pts',(0.788837734090688,-1.,3.85683995872536));
#39621=CARTESIAN_POINT('Ctrl Pts',(0.788837734090688,1.,3.85683995872536));
#39622=CARTESIAN_POINT('Ctrl Pts',(0.789560798155618,-1.,3.8493163780891));
#39623=CARTESIAN_POINT('Ctrl Pts',(0.789560798155618,1.,3.8493163780891));
#39624=CARTESIAN_POINT('Ctrl Pts',(0.790236124191289,-1.,3.84180762342476));
#39625=CARTESIAN_POINT('Ctrl Pts',(0.790236124191289,1.,3.84180762342476));
#39626=CARTESIAN_POINT('Ctrl Pts',(0.790865012705339,-1.,3.83432392054804));
#39627=CARTESIAN_POINT('Ctrl Pts',(0.790865012705339,1.,3.83432392054804));
#39628=CARTESIAN_POINT('Ctrl Pts',(0.791447528662381,-1.,3.82687033899799));
#39629=CARTESIAN_POINT('Ctrl Pts',(0.791447528662381,1.,3.82687033899799));
#39630=CARTESIAN_POINT('Ctrl Pts',(0.791981740718606,-1.,3.81944345442237));
#39631=CARTESIAN_POINT('Ctrl Pts',(0.791981740718606,1.,3.81944345442237));
#39632=CARTESIAN_POINT('Ctrl Pts',(0.792462483517568,-1.,3.81202588694726));
#39633=CARTESIAN_POINT('Ctrl Pts',(0.792462483517568,1.,3.81202588694726));
#39634=CARTESIAN_POINT('Ctrl Pts',(0.792882695234692,-1.,3.80459229925598));
#39635=CARTESIAN_POINT('Ctrl Pts',(0.792882695234692,1.,3.80459229925598));
#39636=CARTESIAN_POINT('Ctrl Pts',(0.7932356129732,-1.,3.79711921389862));
#39637=CARTESIAN_POINT('Ctrl Pts',(0.7932356129732,1.,3.79711921389862));
#39638=CARTESIAN_POINT('Ctrl Pts',(0.793516871680965,-1.,3.78959439439222));
#39639=CARTESIAN_POINT('Ctrl Pts',(0.793516871680965,1.,3.78959439439222));
#39640=CARTESIAN_POINT('Ctrl Pts',(0.793726235781339,-1.,3.78202460377617));
#39641=CARTESIAN_POINT('Ctrl Pts',(0.793726235781339,1.,3.78202460377617));
#39642=CARTESIAN_POINT('Ctrl Pts',(0.793870523787515,-1.,3.77444863801264));
#39643=CARTESIAN_POINT('Ctrl Pts',(0.793870523787515,1.,3.77444863801264));
#39644=CARTESIAN_POINT('Ctrl Pts',(0.793961083689141,-1.,3.76692626931184));
#39645=CARTESIAN_POINT('Ctrl Pts',(0.793961083689141,1.,3.76692626931184));
#39646=CARTESIAN_POINT('Ctrl Pts',(0.794008429135046,-1.,3.75951468666325));
#39647=CARTESIAN_POINT('Ctrl Pts',(0.794008429135046,1.,3.75951468666325));
#39648=CARTESIAN_POINT('Ctrl Pts',(0.79401734737144,-1.,3.75224692493895));
#39649=CARTESIAN_POINT('Ctrl Pts',(0.79401734737144,1.,3.75224692493895));
#39650=CARTESIAN_POINT('Ctrl Pts',(0.79398270045988,-1.,3.74511357728827));
#39651=CARTESIAN_POINT('Ctrl Pts',(0.79398270045988,1.,3.74511357728827));
#39652=CARTESIAN_POINT('Ctrl Pts',(0.79388270093679,-1.,3.73803280541576));
#39653=CARTESIAN_POINT('Ctrl Pts',(0.79388270093679,1.,3.73803280541576));
#39654=CARTESIAN_POINT('Ctrl Pts',(0.793682750269347,-1.,3.7308691469564));
#39655=CARTESIAN_POINT('Ctrl Pts',(0.793682750269347,1.,3.7308691469564));
#39656=CARTESIAN_POINT('Ctrl Pts',(0.79334702378387,-1.,3.7234879729357));
#39657=CARTESIAN_POINT('Ctrl Pts',(0.79334702378387,1.,3.7234879729357));
#39658=CARTESIAN_POINT('Ctrl Pts',(0.792848377370115,-1.,3.7158024239604));
#39659=CARTESIAN_POINT('Ctrl Pts',(0.792848377370115,1.,3.7158024239604));
#39660=CARTESIAN_POINT('Ctrl Pts',(0.792177688845967,-1.,3.70781724021879));
#39661=CARTESIAN_POINT('Ctrl Pts',(0.792177688845967,1.,3.70781724021879));
#39662=CARTESIAN_POINT('Ctrl Pts',(0.791356575696508,-1.,3.69968940808982));
#39663=CARTESIAN_POINT('Ctrl Pts',(0.791356575696508,1.,3.69968940808982));
#39664=CARTESIAN_POINT('Ctrl Pts',(0.790436284989579,-1.,3.69172044327754));
#39665=CARTESIAN_POINT('Ctrl Pts',(0.790436284989579,1.,3.69172044327754));
#39666=CARTESIAN_POINT('Ctrl Pts',(0.789483546065158,-1.,3.68428439784285));
#39667=CARTESIAN_POINT('Ctrl Pts',(0.789483546065158,1.,3.68428439784285));
#39668=CARTESIAN_POINT('Ctrl Pts',(0.788569566220662,-1.,3.67777119516438));
#39669=CARTESIAN_POINT('Ctrl Pts',(0.788569566220662,1.,3.67777119516438));
#39670=CARTESIAN_POINT('Ctrl Pts',(0.787758799995426,-1.,3.672529236635));
#39671=CARTESIAN_POINT('Ctrl Pts',(0.787758799995426,1.,3.672529236635));
#39672=CARTESIAN_POINT('Ctrl Pts',(0.787095252589507,-1.,3.66879484800625));
#39673=CARTESIAN_POINT('Ctrl Pts',(0.787095252589507,1.,3.66879484800625));
#39674=CARTESIAN_POINT('Ctrl Pts',(0.786698783541657,-1.,3.66710211819938));
#39675=CARTESIAN_POINT('Ctrl Pts',(0.786698783541657,1.,3.66710211819938));
#39676=CARTESIAN_POINT('Ctrl Pts',(0.786480236184947,-1.,3.66657784454965));
#39677=CARTESIAN_POINT('Ctrl Pts',(0.786480236184947,1.,3.66657784454965));
#39678=CARTESIAN_POINT('Ctrl Pts',(0.786369528183039,-1.,3.66655932661846));
#39679=CARTESIAN_POINT('Ctrl Pts',(0.786369528183039,1.,3.66655932661846));
#39680=CARTESIAN_POINT('Ctrl Pts',(0.786322922920599,-1.,3.66663282329846));
#39681=CARTESIAN_POINT('Ctrl Pts',(0.786322922920599,1.,3.66663282329846));
#39682=CARTESIAN_POINT('',(0.732042837400619,1.,4.13571194405636));
#39683=CARTESIAN_POINT('Ctrl Pts',(0.732042837400619,1.,4.13571194405636));
#39684=CARTESIAN_POINT('Ctrl Pts',(0.732488575135925,1.,4.13420383737278));
#39685=CARTESIAN_POINT('Ctrl Pts',(0.733376589325634,1.,4.13118752796397));
#39686=CARTESIAN_POINT('Ctrl Pts',(0.734698226767512,1.,4.12666277572794));
#39687=CARTESIAN_POINT('Ctrl Pts',(0.736439634335347,1.,4.12062919626082));
#39688=CARTESIAN_POINT('Ctrl Pts',(0.738581708229118,1.,4.11308626953795));
#39689=CARTESIAN_POINT('Ctrl Pts',(0.740688998555151,1.,4.1055424175856));
#39690=CARTESIAN_POINT('Ctrl Pts',(0.742761369690017,1.,4.09799769702712));
#39691=CARTESIAN_POINT('Ctrl Pts',(0.744798649705513,1.,4.09045220253011));
#39692=CARTESIAN_POINT('Ctrl Pts',(0.746800631490821,1.,4.08290608094789));
#39693=CARTESIAN_POINT('Ctrl Pts',(0.748767076679176,1.,4.07535951055363));
#39694=CARTESIAN_POINT('Ctrl Pts',(0.750697720483175,1.,4.06781267241886));
#39695=CARTESIAN_POINT('Ctrl Pts',(0.752592276482868,1.,4.06026572221399));
#39696=CARTESIAN_POINT('Ctrl Pts',(0.754450441816411,1.,4.05271876688106));
#39697=CARTESIAN_POINT('Ctrl Pts',(0.756271902370186,1.,4.04517182654344));
#39698=CARTESIAN_POINT('Ctrl Pts',(0.758056338885553,1.,4.03762485803468));
#39699=CARTESIAN_POINT('Ctrl Pts',(0.759803433244165,1.,4.0300778195465));
#39700=CARTESIAN_POINT('Ctrl Pts',(0.761512875859941,1.,4.02253072741347));
#39701=CARTESIAN_POINT('Ctrl Pts',(0.763184371182826,1.,4.01498370680434));
#39702=CARTESIAN_POINT('Ctrl Pts',(0.764817648784946,1.,4.00743706791366));
#39703=CARTESIAN_POINT('Ctrl Pts',(0.766412457135785,1.,3.99989129179464));
#39704=CARTESIAN_POINT('Ctrl Pts',(0.767968531377707,1.,3.99234687880892));
#39705=CARTESIAN_POINT('Ctrl Pts',(0.769485566245459,1.,3.98480422348403));
#39706=CARTESIAN_POINT('Ctrl Pts',(0.770963190030503,1.,3.97726349165507));
#39707=CARTESIAN_POINT('Ctrl Pts',(0.772400931772238,1.,3.96972446532832));
#39708=CARTESIAN_POINT('Ctrl Pts',(0.773798212026682,1.,3.96218649639876));
#39709=CARTESIAN_POINT('Ctrl Pts',(0.775154418039441,1.,3.95464885452364));
#39710=CARTESIAN_POINT('Ctrl Pts',(0.776468966697959,1.,3.94711101619471));
#39711=CARTESIAN_POINT('Ctrl Pts',(0.777741370568549,1.,3.93957296768098));
#39712=CARTESIAN_POINT('Ctrl Pts',(0.778971308134786,1.,3.93203552473153));
#39713=CARTESIAN_POINT('Ctrl Pts',(0.780158678615506,1.,3.92450058323799));
#39714=CARTESIAN_POINT('Ctrl Pts',(0.781303428618343,1.,3.9169703605466));
#39715=CARTESIAN_POINT('Ctrl Pts',(0.782405395622758,1.,3.90944671004536));
#39716=CARTESIAN_POINT('Ctrl Pts',(0.783464141529082,1.,3.90193039043971));
#39717=CARTESIAN_POINT('Ctrl Pts',(0.784478799358335,1.,3.89442039235105));
#39718=CARTESIAN_POINT('Ctrl Pts',(0.785447890340723,1.,3.88691313167399));
#39719=CARTESIAN_POINT('Ctrl Pts',(0.786369675812591,1.,3.87940402818186));
#39720=CARTESIAN_POINT('Ctrl Pts',(0.78724252761798,1.,3.87188916600905));
#39721=CARTESIAN_POINT('Ctrl Pts',(0.78806531509377,1.,3.86436702561342));
#39722=CARTESIAN_POINT('Ctrl Pts',(0.788837734090688,1.,3.85683995872536));
#39723=CARTESIAN_POINT('Ctrl Pts',(0.789560798155618,1.,3.8493163780891));
#39724=CARTESIAN_POINT('Ctrl Pts',(0.790236124191289,1.,3.84180762342476));
#39725=CARTESIAN_POINT('Ctrl Pts',(0.790865012705339,1.,3.83432392054804));
#39726=CARTESIAN_POINT('Ctrl Pts',(0.791447528662381,1.,3.82687033899799));
#39727=CARTESIAN_POINT('Ctrl Pts',(0.791981740718606,1.,3.81944345442237));
#39728=CARTESIAN_POINT('Ctrl Pts',(0.792462483517568,1.,3.81202588694726));
#39729=CARTESIAN_POINT('Ctrl Pts',(0.792882695234692,1.,3.80459229925598));
#39730=CARTESIAN_POINT('Ctrl Pts',(0.7932356129732,1.,3.79711921389862));
#39731=CARTESIAN_POINT('Ctrl Pts',(0.793516871680965,1.,3.78959439439222));
#39732=CARTESIAN_POINT('Ctrl Pts',(0.793726235781339,1.,3.78202460377617));
#39733=CARTESIAN_POINT('Ctrl Pts',(0.793870523787515,1.,3.77444863801264));
#39734=CARTESIAN_POINT('Ctrl Pts',(0.793961083689141,1.,3.76692626931184));
#39735=CARTESIAN_POINT('Ctrl Pts',(0.794008429135046,1.,3.75951468666325));
#39736=CARTESIAN_POINT('Ctrl Pts',(0.79401734737144,1.,3.75224692493895));
#39737=CARTESIAN_POINT('Ctrl Pts',(0.79398270045988,1.,3.74511357728827));
#39738=CARTESIAN_POINT('Ctrl Pts',(0.79388270093679,1.,3.73803280541576));
#39739=CARTESIAN_POINT('Ctrl Pts',(0.793682750269347,1.,3.7308691469564));
#39740=CARTESIAN_POINT('Ctrl Pts',(0.79334702378387,1.,3.7234879729357));
#39741=CARTESIAN_POINT('Ctrl Pts',(0.792848377370115,1.,3.7158024239604));
#39742=CARTESIAN_POINT('Ctrl Pts',(0.792177688845967,1.,3.70781724021879));
#39743=CARTESIAN_POINT('Ctrl Pts',(0.791356575696508,1.,3.69968940808982));
#39744=CARTESIAN_POINT('Ctrl Pts',(0.790436284989579,1.,3.69172044327754));
#39745=CARTESIAN_POINT('Ctrl Pts',(0.789483546065158,1.,3.68428439784285));
#39746=CARTESIAN_POINT('Ctrl Pts',(0.788569566220662,1.,3.67777119516438));
#39747=CARTESIAN_POINT('Ctrl Pts',(0.787758799995426,1.,3.672529236635));
#39748=CARTESIAN_POINT('Ctrl Pts',(0.787145041181588,1.,3.66907505398769));
#39749=CARTESIAN_POINT('Ctrl Pts',(0.786774337198499,1.,3.66743103898844));
#39750=CARTESIAN_POINT('Ctrl Pts',(0.786565919559889,1.,3.66680946938396));
#39751=CARTESIAN_POINT('Ctrl Pts',(0.786459983896781,1.,3.66664310415236));
#39752=CARTESIAN_POINT('Ctrl Pts',(0.786422660833743,1.,3.66661143271648));
#39753=CARTESIAN_POINT('',(0.732042837400619,0.,4.13571194405636));
#39754=CARTESIAN_POINT('Ctrl Pts',(0.385214314776328,-1.,3.73016218570874));
#39755=CARTESIAN_POINT('Ctrl Pts',(0.385214314776328,1.,3.73016218570874));
#39756=CARTESIAN_POINT('Ctrl Pts',(0.385147278814803,-1.,3.73010668803185));
#39757=CARTESIAN_POINT('Ctrl Pts',(0.385147278814803,1.,3.73010668803185));
#39758=CARTESIAN_POINT('Ctrl Pts',(0.385047711603887,-1.,3.73015851028729));
#39759=CARTESIAN_POINT('Ctrl Pts',(0.385047711603887,1.,3.73015851028729));
#39760=CARTESIAN_POINT('Ctrl Pts',(0.385001870183841,-1.,3.73072465900727));
#39761=CARTESIAN_POINT('Ctrl Pts',(0.385001870183841,1.,3.73072465900727));
#39762=CARTESIAN_POINT('Ctrl Pts',(0.385147887989514,-1.,3.73245705639337));
#39763=CARTESIAN_POINT('Ctrl Pts',(0.385147887989514,1.,3.73245705639337));
#39764=CARTESIAN_POINT('Ctrl Pts',(0.385670806454744,-1.,3.73621371845475));
#39765=CARTESIAN_POINT('Ctrl Pts',(0.385670806454744,1.,3.73621371845475));
#39766=CARTESIAN_POINT('Ctrl Pts',(0.386519576222035,-1.,3.74144965781088));
#39767=CARTESIAN_POINT('Ctrl Pts',(0.386519576222035,1.,3.74144965781088));
#39768=CARTESIAN_POINT('Ctrl Pts',(0.387663020050396,-1.,3.74792651696269));
#39769=CARTESIAN_POINT('Ctrl Pts',(0.387663020050396,1.,3.74792651696269));
#39770=CARTESIAN_POINT('Ctrl Pts',(0.38905477589825,-1.,3.75529302894757));
#39771=CARTESIAN_POINT('Ctrl Pts',(0.38905477589825,1.,3.75529302894757));
#39772=CARTESIAN_POINT('Ctrl Pts',(0.390642072979258,-1.,3.76315635032993));
#39773=CARTESIAN_POINT('Ctrl Pts',(0.390642072979258,1.,3.76315635032993));
#39774=CARTESIAN_POINT('Ctrl Pts',(0.392372786223346,-1.,3.77114011595892));
#39775=CARTESIAN_POINT('Ctrl Pts',(0.392372786223346,1.,3.77114011595892));
#39776=CARTESIAN_POINT('Ctrl Pts',(0.394202481011595,-1.,3.77894173114368));
#39777=CARTESIAN_POINT('Ctrl Pts',(0.394202481011595,1.,3.77894173114368));
#39778=CARTESIAN_POINT('Ctrl Pts',(0.396103205335028,-1.,3.78640521279479));
#39779=CARTESIAN_POINT('Ctrl Pts',(0.396103205335028,1.,3.78640521279479));
#39780=CARTESIAN_POINT('Ctrl Pts',(0.398064818684158,-1.,3.79352887163457));
#39781=CARTESIAN_POINT('Ctrl Pts',(0.398064818684158,1.,3.79352887163457));
#39782=CARTESIAN_POINT('Ctrl Pts',(0.400088346504726,-1.,3.80040370384659));
#39783=CARTESIAN_POINT('Ctrl Pts',(0.400088346504726,1.,3.80040370384659));
#39784=CARTESIAN_POINT('Ctrl Pts',(0.402181320148474,-1.,3.80716881962763));
#39785=CARTESIAN_POINT('Ctrl Pts',(0.402181320148474,1.,3.80716881962763));
#39786=CARTESIAN_POINT('Ctrl Pts',(0.404352694628236,-1.,3.81396374287762));
#39787=CARTESIAN_POINT('Ctrl Pts',(0.404352694628236,1.,3.81396374287762));
#39788=CARTESIAN_POINT('Ctrl Pts',(0.406607038258906,-1.,3.82087303913741));
#39789=CARTESIAN_POINT('Ctrl Pts',(0.406607038258906,1.,3.82087303913741));
#39790=CARTESIAN_POINT('Ctrl Pts',(0.408942371447376,-1.,3.82790724256397));
#39791=CARTESIAN_POINT('Ctrl Pts',(0.408942371447376,1.,3.82790724256397));
#39792=CARTESIAN_POINT('Ctrl Pts',(0.411353038798459,-1.,3.83503345578645));
#39793=CARTESIAN_POINT('Ctrl Pts',(0.411353038798459,1.,3.83503345578645));
#39794=CARTESIAN_POINT('Ctrl Pts',(0.413831367016726,-1.,3.84219403994742));
#39795=CARTESIAN_POINT('Ctrl Pts',(0.413831367016726,1.,3.84219403994742));
#39796=CARTESIAN_POINT('Ctrl Pts',(0.41636967805292,-1.,3.8493286415751));
#39797=CARTESIAN_POINT('Ctrl Pts',(0.41636967805292,1.,3.8493286415751));
#39798=CARTESIAN_POINT('Ctrl Pts',(0.418962468086809,-1.,3.85639825648031));
#39799=CARTESIAN_POINT('Ctrl Pts',(0.418962468086809,1.,3.85639825648031));
#39800=CARTESIAN_POINT('Ctrl Pts',(0.421607423177575,-1.,3.86339652542749));
#39801=CARTESIAN_POINT('Ctrl Pts',(0.421607423177575,1.,3.86339652542749));
#39802=CARTESIAN_POINT('Ctrl Pts',(0.424304173195142,-1.,3.87033643487882));
#39803=CARTESIAN_POINT('Ctrl Pts',(0.424304173195142,1.,3.87033643487882));
#39804=CARTESIAN_POINT('Ctrl Pts',(0.427053541173469,-1.,3.87724240306609));
#39805=CARTESIAN_POINT('Ctrl Pts',(0.427053541173469,1.,3.87724240306609));
#39806=CARTESIAN_POINT('Ctrl Pts',(0.429856640579733,-1.,3.88414070943334));
#39807=CARTESIAN_POINT('Ctrl Pts',(0.429856640579733,1.,3.88414070943334));
#39808=CARTESIAN_POINT('Ctrl Pts',(0.432713929544439,-1.,3.89104947940592));
#39809=CARTESIAN_POINT('Ctrl Pts',(0.432713929544439,1.,3.89104947940592));
#39810=CARTESIAN_POINT('Ctrl Pts',(0.435624629433505,-1.,3.8979725665544));
#39811=CARTESIAN_POINT('Ctrl Pts',(0.435624629433505,1.,3.8979725665544));
#39812=CARTESIAN_POINT('Ctrl Pts',(0.438587235458233,-1.,3.90490512938546));
#39813=CARTESIAN_POINT('Ctrl Pts',(0.438587235458233,1.,3.90490512938546));
#39814=CARTESIAN_POINT('Ctrl Pts',(0.441599824524047,-1.,3.91183704069146));
#39815=CARTESIAN_POINT('Ctrl Pts',(0.441599824524047,1.,3.91183704069146));
#39816=CARTESIAN_POINT('Ctrl Pts',(0.444660430230592,-1.,3.91875701610721));
#39817=CARTESIAN_POINT('Ctrl Pts',(0.444660430230592,1.,3.91875701610721));
#39818=CARTESIAN_POINT('Ctrl Pts',(0.447767416837296,-1.,3.92565674143424));
#39819=CARTESIAN_POINT('Ctrl Pts',(0.447767416837296,1.,3.92565674143424));
#39820=CARTESIAN_POINT('Ctrl Pts',(0.450919768356346,-1.,3.93253407403128));
#39821=CARTESIAN_POINT('Ctrl Pts',(0.450919768356346,1.,3.93253407403128));
#39822=CARTESIAN_POINT('Ctrl Pts',(0.454116879027575,-1.,3.93939080846298));
#39823=CARTESIAN_POINT('Ctrl Pts',(0.454116879027575,1.,3.93939080846298));
#39824=CARTESIAN_POINT('Ctrl Pts',(0.457358410451673,-1.,3.94623117206675));
#39825=CARTESIAN_POINT('Ctrl Pts',(0.457358410451673,1.,3.94623117206675));
#39826=CARTESIAN_POINT('Ctrl Pts',(0.460644124429119,-1.,3.95306005817363));
#39827=CARTESIAN_POINT('Ctrl Pts',(0.460644124429119,1.,3.95306005817363));
#39828=CARTESIAN_POINT('Ctrl Pts',(0.463973722115744,-1.,3.95988133243543));
#39829=CARTESIAN_POINT('Ctrl Pts',(0.463973722115744,1.,3.95988133243543));
#39830=CARTESIAN_POINT('Ctrl Pts',(0.467346690880671,-1.,3.96669622273946));
#39831=CARTESIAN_POINT('Ctrl Pts',(0.467346690880671,1.,3.96669622273946));
#39832=CARTESIAN_POINT('Ctrl Pts',(0.470762379613477,-1.,3.97350414289415));
#39833=CARTESIAN_POINT('Ctrl Pts',(0.470762379613477,1.,3.97350414289415));
#39834=CARTESIAN_POINT('Ctrl Pts',(0.474220061019542,-1.,3.9803033804443));
#39835=CARTESIAN_POINT('Ctrl Pts',(0.474220061019542,1.,3.9803033804443));
#39836=CARTESIAN_POINT('Ctrl Pts',(0.477718999122033,-1.,3.98709184306743));
#39837=CARTESIAN_POINT('Ctrl Pts',(0.477718999122033,1.,3.98709184306743));
#39838=CARTESIAN_POINT('Ctrl Pts',(0.481258512209637,-1.,3.99386775880655));
#39839=CARTESIAN_POINT('Ctrl Pts',(0.481258512209637,1.,3.99386775880655));
#39840=CARTESIAN_POINT('Ctrl Pts',(0.484838042421754,-1.,4.00063045119234));
#39841=CARTESIAN_POINT('Ctrl Pts',(0.484838042421754,1.,4.00063045119234));
#39842=CARTESIAN_POINT('Ctrl Pts',(0.48845713042453,-1.,4.0073800839092));
#39843=CARTESIAN_POINT('Ctrl Pts',(0.48845713042453,1.,4.0073800839092));
#39844=CARTESIAN_POINT('Ctrl Pts',(0.49211538341793,-1.,4.01411733503486));
#39845=CARTESIAN_POINT('Ctrl Pts',(0.49211538341793,1.,4.01411733503486));
#39846=CARTESIAN_POINT('Ctrl Pts',(0.495812444326222,-1.,4.02084308851813));
#39847=CARTESIAN_POINT('Ctrl Pts',(0.495812444326222,1.,4.02084308851813));
#39848=CARTESIAN_POINT('Ctrl Pts',(0.499547962340889,-1.,4.0275581398015));
#39849=CARTESIAN_POINT('Ctrl Pts',(0.499547962340889,1.,4.0275581398015));
#39850=CARTESIAN_POINT('Ctrl Pts',(0.503321556915513,-1.,4.0342628417439));
#39851=CARTESIAN_POINT('Ctrl Pts',(0.503321556915513,1.,4.0342628417439));
#39852=CARTESIAN_POINT('Ctrl Pts',(0.507132823288361,-1.,4.04095715149074));
#39853=CARTESIAN_POINT('Ctrl Pts',(0.507132823288361,1.,4.04095715149074));
#39854=CARTESIAN_POINT('Ctrl Pts',(0.510981349219173,-1.,4.04764078815591));
#39855=CARTESIAN_POINT('Ctrl Pts',(0.510981349219173,1.,4.04764078815591));
#39856=CARTESIAN_POINT('Ctrl Pts',(0.514866728193103,-1.,4.05431335771261));
#39857=CARTESIAN_POINT('Ctrl Pts',(0.514866728193103,1.,4.05431335771261));
#39858=CARTESIAN_POINT('Ctrl Pts',(0.518788572336809,-1.,4.06097448037934));
#39859=CARTESIAN_POINT('Ctrl Pts',(0.518788572336809,1.,4.06097448037934));
#39860=CARTESIAN_POINT('Ctrl Pts',(0.522746528602767,-1.,4.06762394471075));
#39861=CARTESIAN_POINT('Ctrl Pts',(0.522746528602767,1.,4.06762394471075));
#39862=CARTESIAN_POINT('Ctrl Pts',(0.526740277226999,-1.,4.07426172299496));
#39863=CARTESIAN_POINT('Ctrl Pts',(0.526740277226999,1.,4.07426172299496));
#39864=CARTESIAN_POINT('Ctrl Pts',(0.530769518728075,-1.,4.08088789536488));
#39865=CARTESIAN_POINT('Ctrl Pts',(0.530769518728075,1.,4.08088789536488));
#39866=CARTESIAN_POINT('Ctrl Pts',(0.534833963476999,-1.,4.08750259988693));
#39867=CARTESIAN_POINT('Ctrl Pts',(0.534833963476999,1.,4.08750259988693));
#39868=CARTESIAN_POINT('Ctrl Pts',(0.53893332117992,-1.,4.09410597627116));
#39869=CARTESIAN_POINT('Ctrl Pts',(0.53893332117992,1.,4.09410597627116));
#39870=CARTESIAN_POINT('Ctrl Pts',(0.543067286878457,-1.,4.10069810244473));
#39871=CARTESIAN_POINT('Ctrl Pts',(0.543067286878457,1.,4.10069810244473));
#39872=CARTESIAN_POINT('Ctrl Pts',(0.547235539486759,-1.,4.1072789702877));
#39873=CARTESIAN_POINT('Ctrl Pts',(0.547235539486759,1.,4.1072789702877));
#39874=CARTESIAN_POINT('Ctrl Pts',(0.551437758498246,-1.,4.11384852025578));
#39875=CARTESIAN_POINT('Ctrl Pts',(0.551437758498246,1.,4.11384852025578));
#39876=CARTESIAN_POINT('Ctrl Pts',(0.555673636130778,-1.,4.1204066619623));
#39877=CARTESIAN_POINT('Ctrl Pts',(0.555673636130778,1.,4.1204066619623));
#39878=CARTESIAN_POINT('Ctrl Pts',(0.559942890594628,-1.,4.12695329951859));
#39879=CARTESIAN_POINT('Ctrl Pts',(0.559942890594628,1.,4.12695329951859));
#39880=CARTESIAN_POINT('Ctrl Pts',(0.564245279535705,-1.,4.13348835726086));
#39881=CARTESIAN_POINT('Ctrl Pts',(0.564245279535705,1.,4.13348835726086));
#39882=CARTESIAN_POINT('Ctrl Pts',(0.568580610187115,-1.,4.14001179828669));
#39883=CARTESIAN_POINT('Ctrl Pts',(0.568580610187115,1.,4.14001179828669));
#39884=CARTESIAN_POINT('Ctrl Pts',(0.572948736066276,-1.,4.14652361065787));
#39885=CARTESIAN_POINT('Ctrl Pts',(0.572948736066276,1.,4.14652361065787));
#39886=CARTESIAN_POINT('Ctrl Pts',(0.576469391673916,-1.,4.1517237611974));
#39887=CARTESIAN_POINT('Ctrl Pts',(0.576469391673916,1.,4.1517237611974));
#39888=CARTESIAN_POINT('Ctrl Pts',(0.579124568912543,-1.,4.15561864787379));
#39889=CARTESIAN_POINT('Ctrl Pts',(0.579124568912543,1.,4.15561864787379));
#39890=CARTESIAN_POINT('Ctrl Pts',(0.580901211462913,-1.,4.15821291712391));
#39891=CARTESIAN_POINT('Ctrl Pts',(0.580901211462913,1.,4.15821291712391));
#39892=CARTESIAN_POINT('Ctrl Pts',(0.581791163835814,-1.,4.15950947128175));
#39893=CARTESIAN_POINT('Ctrl Pts',(0.581791163835814,1.,4.15950947128175));
#39894=CARTESIAN_POINT('',(0.385112848332548,1.,3.73017266276632));
#39895=CARTESIAN_POINT('Ctrl Pts',(0.385112848332548,-1.,3.73017266276632));
#39896=CARTESIAN_POINT('Ctrl Pts',(0.385112848332548,-0.666666666666667,
3.73017266276632));
#39897=CARTESIAN_POINT('Ctrl Pts',(0.385112848332548,-0.333333333333333,
3.73017266276632));
#39898=CARTESIAN_POINT('Ctrl Pts',(0.385112848332548,0.333333333333333,
3.73017266276632));
#39899=CARTESIAN_POINT('Ctrl Pts',(0.385112848332548,0.666666666666667,
3.73017266276632));
#39900=CARTESIAN_POINT('Ctrl Pts',(0.385112848332548,1.,3.73017266276632));
#39901=CARTESIAN_POINT('',(0.581791163835814,1.,4.15950947128175));
#39902=CARTESIAN_POINT('',(0.581791163835814,0.,4.15950947128175));
#39903=CARTESIAN_POINT('Ctrl Pts',(0.385112848332549,1.,3.73017266276632));
#39904=CARTESIAN_POINT('Ctrl Pts',(0.385087139001608,1.,3.73021431755218));
#39905=CARTESIAN_POINT('Ctrl Pts',(0.385037797882046,1.,3.73040527620929));
#39906=CARTESIAN_POINT('Ctrl Pts',(0.385031656499141,1.,3.731060828624));
#39907=CARTESIAN_POINT('Ctrl Pts',(0.385187124633964,1.,3.73273893363318));
#39908=CARTESIAN_POINT('Ctrl Pts',(0.385670806454744,1.,3.73621371845475));
#39909=CARTESIAN_POINT('Ctrl Pts',(0.386519576222035,1.,3.74144965781088));
#39910=CARTESIAN_POINT('Ctrl Pts',(0.387663020050396,1.,3.74792651696269));
#39911=CARTESIAN_POINT('Ctrl Pts',(0.38905477589825,1.,3.75529302894757));
#39912=CARTESIAN_POINT('Ctrl Pts',(0.390642072979258,1.,3.76315635032993));
#39913=CARTESIAN_POINT('Ctrl Pts',(0.392372786223346,1.,3.77114011595892));
#39914=CARTESIAN_POINT('Ctrl Pts',(0.394202481011595,1.,3.77894173114368));
#39915=CARTESIAN_POINT('Ctrl Pts',(0.396103205335028,1.,3.78640521279479));
#39916=CARTESIAN_POINT('Ctrl Pts',(0.398064818684158,1.,3.79352887163457));
#39917=CARTESIAN_POINT('Ctrl Pts',(0.400088346504726,1.,3.80040370384659));
#39918=CARTESIAN_POINT('Ctrl Pts',(0.402181320148474,1.,3.80716881962763));
#39919=CARTESIAN_POINT('Ctrl Pts',(0.404352694628236,1.,3.81396374287762));
#39920=CARTESIAN_POINT('Ctrl Pts',(0.406607038258906,1.,3.82087303913741));
#39921=CARTESIAN_POINT('Ctrl Pts',(0.408942371447376,1.,3.82790724256397));
#39922=CARTESIAN_POINT('Ctrl Pts',(0.411353038798459,1.,3.83503345578645));
#39923=CARTESIAN_POINT('Ctrl Pts',(0.413831367016726,1.,3.84219403994742));
#39924=CARTESIAN_POINT('Ctrl Pts',(0.41636967805292,1.,3.8493286415751));
#39925=CARTESIAN_POINT('Ctrl Pts',(0.418962468086809,1.,3.85639825648031));
#39926=CARTESIAN_POINT('Ctrl Pts',(0.421607423177575,1.,3.86339652542749));
#39927=CARTESIAN_POINT('Ctrl Pts',(0.424304173195142,1.,3.87033643487882));
#39928=CARTESIAN_POINT('Ctrl Pts',(0.427053541173469,1.,3.87724240306609));
#39929=CARTESIAN_POINT('Ctrl Pts',(0.429856640579733,1.,3.88414070943334));
#39930=CARTESIAN_POINT('Ctrl Pts',(0.432713929544439,1.,3.89104947940592));
#39931=CARTESIAN_POINT('Ctrl Pts',(0.435624629433505,1.,3.8979725665544));
#39932=CARTESIAN_POINT('Ctrl Pts',(0.438587235458233,1.,3.90490512938546));
#39933=CARTESIAN_POINT('Ctrl Pts',(0.441599824524047,1.,3.91183704069146));
#39934=CARTESIAN_POINT('Ctrl Pts',(0.444660430230592,1.,3.91875701610721));
#39935=CARTESIAN_POINT('Ctrl Pts',(0.447767416837296,1.,3.92565674143424));
#39936=CARTESIAN_POINT('Ctrl Pts',(0.450919768356346,1.,3.93253407403128));
#39937=CARTESIAN_POINT('Ctrl Pts',(0.454116879027575,1.,3.93939080846298));
#39938=CARTESIAN_POINT('Ctrl Pts',(0.457358410451673,1.,3.94623117206675));
#39939=CARTESIAN_POINT('Ctrl Pts',(0.460644124429119,1.,3.95306005817363));
#39940=CARTESIAN_POINT('Ctrl Pts',(0.463973722115744,1.,3.95988133243543));
#39941=CARTESIAN_POINT('Ctrl Pts',(0.467346690880671,1.,3.96669622273946));
#39942=CARTESIAN_POINT('Ctrl Pts',(0.470762379613477,1.,3.97350414289415));
#39943=CARTESIAN_POINT('Ctrl Pts',(0.474220061019542,1.,3.9803033804443));
#39944=CARTESIAN_POINT('Ctrl Pts',(0.477718999122033,1.,3.98709184306743));
#39945=CARTESIAN_POINT('Ctrl Pts',(0.481258512209637,1.,3.99386775880655));
#39946=CARTESIAN_POINT('Ctrl Pts',(0.484838042421754,1.,4.00063045119234));
#39947=CARTESIAN_POINT('Ctrl Pts',(0.48845713042453,1.,4.0073800839092));
#39948=CARTESIAN_POINT('Ctrl Pts',(0.49211538341793,1.,4.01411733503486));
#39949=CARTESIAN_POINT('Ctrl Pts',(0.495812444326222,1.,4.02084308851813));
#39950=CARTESIAN_POINT('Ctrl Pts',(0.499547962340889,1.,4.0275581398015));
#39951=CARTESIAN_POINT('Ctrl Pts',(0.503321556915513,1.,4.0342628417439));
#39952=CARTESIAN_POINT('Ctrl Pts',(0.507132823288361,1.,4.04095715149074));
#39953=CARTESIAN_POINT('Ctrl Pts',(0.510981349219173,1.,4.04764078815591));
#39954=CARTESIAN_POINT('Ctrl Pts',(0.514866728193103,1.,4.05431335771261));
#39955=CARTESIAN_POINT('Ctrl Pts',(0.518788572336809,1.,4.06097448037934));
#39956=CARTESIAN_POINT('Ctrl Pts',(0.522746528602767,1.,4.06762394471075));
#39957=CARTESIAN_POINT('Ctrl Pts',(0.526740277226999,1.,4.07426172299496));
#39958=CARTESIAN_POINT('Ctrl Pts',(0.530769518728075,1.,4.08088789536488));
#39959=CARTESIAN_POINT('Ctrl Pts',(0.534833963476999,1.,4.08750259988693));
#39960=CARTESIAN_POINT('Ctrl Pts',(0.53893332117992,1.,4.09410597627116));
#39961=CARTESIAN_POINT('Ctrl Pts',(0.543067286878457,1.,4.10069810244473));
#39962=CARTESIAN_POINT('Ctrl Pts',(0.547235539486759,1.,4.1072789702877));
#39963=CARTESIAN_POINT('Ctrl Pts',(0.551437758498246,1.,4.11384852025578));
#39964=CARTESIAN_POINT('Ctrl Pts',(0.555673636130778,1.,4.1204066619623));
#39965=CARTESIAN_POINT('Ctrl Pts',(0.559942890594628,1.,4.12695329951859));
#39966=CARTESIAN_POINT('Ctrl Pts',(0.564245279535705,1.,4.13348835726086));
#39967=CARTESIAN_POINT('Ctrl Pts',(0.568580610187115,1.,4.14001179828669));
#39968=CARTESIAN_POINT('Ctrl Pts',(0.572948736066276,1.,4.14652361065787));
#39969=CARTESIAN_POINT('Ctrl Pts',(0.576469391673916,1.,4.1517237611974));
#39970=CARTESIAN_POINT('Ctrl Pts',(0.579124568912543,1.,4.15561864787379));
#39971=CARTESIAN_POINT('Ctrl Pts',(0.580901211462913,1.,4.15821291712391));
#39972=CARTESIAN_POINT('Ctrl Pts',(0.581791163835814,1.,4.15950947128175));
#39973=CARTESIAN_POINT('Origin',(0.581791163835814,0.,4.15950947128175));
#39974=CARTESIAN_POINT('',(0.732042837400619,1.,4.13571194405636));
#39975=CARTESIAN_POINT('Origin',(0.,0.,0.));
#39976=CARTESIAN_POINT('',(0.203156094897895,1.,3.74449296982994));
#39977=CARTESIAN_POINT('Origin',(0.,1.,0.));
#39978=CARTESIAN_POINT('Ctrl Pts',(0.203156094897895,1.,3.74449296982994));
#39979=CARTESIAN_POINT('Ctrl Pts',(0.203156094897895,0.666666666666667,
3.74449296982994));
#39980=CARTESIAN_POINT('Ctrl Pts',(0.203156094897895,0.333333333333333,
3.74449296982994));
#39981=CARTESIAN_POINT('Ctrl Pts',(0.203156094897895,-0.333333333333333,
3.74449296982994));
#39982=CARTESIAN_POINT('Ctrl Pts',(0.203156094897895,-0.666666666666667,
3.74449296982994));
#39983=CARTESIAN_POINT('Ctrl Pts',(0.203156094897895,-1.,3.74449296982994));
#39984=CARTESIAN_POINT('Ctrl Pts',(0.0760622897878233,-1.,4.19931119685982));
#39985=CARTESIAN_POINT('Ctrl Pts',(0.0760622897878233,1.,4.19931119685982));
#39986=CARTESIAN_POINT('Ctrl Pts',(0.0767384596142192,-1.,4.19789138621624));
#39987=CARTESIAN_POINT('Ctrl Pts',(0.0767384596142192,1.,4.19789138621624));
#39988=CARTESIAN_POINT('Ctrl Pts',(0.0780873956244399,-1.,4.19505112860624));
#39989=CARTESIAN_POINT('Ctrl Pts',(0.0780873956244399,1.,4.19505112860624));
#39990=CARTESIAN_POINT('Ctrl Pts',(0.08010058871176,-1.,4.19078883322483));
#39991=CARTESIAN_POINT('Ctrl Pts',(0.08010058871176,1.,4.19078883322483));
#39992=CARTESIAN_POINT('Ctrl Pts',(0.0827644164389507,-1.,4.1851019532944));
#39993=CARTESIAN_POINT('Ctrl Pts',(0.0827644164389507,1.,4.1851019532944));
#39994=CARTESIAN_POINT('Ctrl Pts',(0.0860600915552512,-1.,4.17798698669991));
#39995=CARTESIAN_POINT('Ctrl Pts',(0.0860600915552512,1.,4.17798698669991));
#39996=CARTESIAN_POINT('Ctrl Pts',(0.0893215560850325,-1.,4.17086566491823));
#39997=CARTESIAN_POINT('Ctrl Pts',(0.0893215560850325,1.,4.17086566491823));
#39998=CARTESIAN_POINT('Ctrl Pts',(0.0925486672167687,-1.,4.16373802265942));
#39999=CARTESIAN_POINT('Ctrl Pts',(0.0925486672167687,1.,4.16373802265942));
#40000=CARTESIAN_POINT('Ctrl Pts',(0.0957412403297065,-1.,4.15660412653006));
#40001=CARTESIAN_POINT('Ctrl Pts',(0.0957412403297065,1.,4.15660412653006));
#40002=CARTESIAN_POINT('Ctrl Pts',(0.0988990478899809,-1.,4.1494640891762));
#40003=CARTESIAN_POINT('Ctrl Pts',(0.0988990478899809,1.,4.1494640891762));
#40004=CARTESIAN_POINT('Ctrl Pts',(0.102021826577453,-1.,4.14231804938737));
#40005=CARTESIAN_POINT('Ctrl Pts',(0.102021826577453,1.,4.14231804938737));
#40006=CARTESIAN_POINT('Ctrl Pts',(0.105109286538864,-1.,4.13516614458396));
#40007=CARTESIAN_POINT('Ctrl Pts',(0.105109286538864,1.,4.13516614458396));
#40008=CARTESIAN_POINT('Ctrl Pts',(0.10816112052835,-1.,4.12800848371386));
#40009=CARTESIAN_POINT('Ctrl Pts',(0.10816112052835,1.,4.12800848371386));
#40010=CARTESIAN_POINT('Ctrl Pts',(0.111177012683377,-1.,4.12084512502444));
#40011=CARTESIAN_POINT('Ctrl Pts',(0.111177012683377,1.,4.12084512502444));
#40012=CARTESIAN_POINT('Ctrl Pts',(0.114156649609601,-1.,4.11367603925313));
#40013=CARTESIAN_POINT('Ctrl Pts',(0.114156649609601,1.,4.11367603925313));
#40014=CARTESIAN_POINT('Ctrl Pts',(0.117099722731704,-1.,4.10650113382187));
#40015=CARTESIAN_POINT('Ctrl Pts',(0.117099722731704,1.,4.10650113382187));
#40016=CARTESIAN_POINT('Ctrl Pts',(0.120005924388162,-1.,4.09932031767243));
#40017=CARTESIAN_POINT('Ctrl Pts',(0.120005924388162,1.,4.09932031767243));
#40018=CARTESIAN_POINT('Ctrl Pts',(0.122874946249119,-1.,4.09213355850836));
#40019=CARTESIAN_POINT('Ctrl Pts',(0.122874946249119,1.,4.09213355850836));
#40020=CARTESIAN_POINT('Ctrl Pts',(0.125706476822529,-1.,4.08494093372315));
#40021=CARTESIAN_POINT('Ctrl Pts',(0.125706476822529,1.,4.08494093372315));
#40022=CARTESIAN_POINT('Ctrl Pts',(0.128500200484813,-1.,4.07774270738809));
#40023=CARTESIAN_POINT('Ctrl Pts',(0.128500200484813,1.,4.07774270738809));
#40024=CARTESIAN_POINT('Ctrl Pts',(0.131255793548914,-1.,4.07053931528579));
#40025=CARTESIAN_POINT('Ctrl Pts',(0.131255793548914,1.,4.07053931528579));
#40026=CARTESIAN_POINT('Ctrl Pts',(0.133972916144225,-1.,4.06333121018476));
#40027=CARTESIAN_POINT('Ctrl Pts',(0.133972916144225,1.,4.06333121018476));
#40028=CARTESIAN_POINT('Ctrl Pts',(0.136651205046111,-1.,4.05611873400122));
#40029=CARTESIAN_POINT('Ctrl Pts',(0.136651205046111,1.,4.05611873400122));
#40030=CARTESIAN_POINT('Ctrl Pts',(0.139290267180059,-1.,4.04890199238056));
#40031=CARTESIAN_POINT('Ctrl Pts',(0.139290267180059,1.,4.04890199238056));
#40032=CARTESIAN_POINT('Ctrl Pts',(0.141889671485507,-1.,4.04168069633842));
#40033=CARTESIAN_POINT('Ctrl Pts',(0.141889671485507,1.,4.04168069633842));
#40034=CARTESIAN_POINT('Ctrl Pts',(0.144448947038352,-1.,4.03445411510403));
#40035=CARTESIAN_POINT('Ctrl Pts',(0.144448947038352,1.,4.03445411510403));
#40036=CARTESIAN_POINT('Ctrl Pts',(0.146967602878998,-1.,4.02722143147048));
#40037=CARTESIAN_POINT('Ctrl Pts',(0.146967602878998,1.,4.02722143147048));
#40038=CARTESIAN_POINT('Ctrl Pts',(0.149445144968707,-1.,4.01998203715588));
#40039=CARTESIAN_POINT('Ctrl Pts',(0.149445144968707,1.,4.01998203715588));
#40040=CARTESIAN_POINT('Ctrl Pts',(0.151881094022909,-1.,4.01273584234684));
#40041=CARTESIAN_POINT('Ctrl Pts',(0.151881094022909,1.,4.01273584234684));
#40042=CARTESIAN_POINT('Ctrl Pts',(0.154275004872309,-1.,4.00548360245297));
#40043=CARTESIAN_POINT('Ctrl Pts',(0.154275004872309,1.,4.00548360245297));
#40044=CARTESIAN_POINT('Ctrl Pts',(0.156626481393735,-1.,3.99822717425869));
#40045=CARTESIAN_POINT('Ctrl Pts',(0.156626481393735,1.,3.99822717425869));
#40046=CARTESIAN_POINT('Ctrl Pts',(0.158935123982796,-1.,3.99096873945862));
#40047=CARTESIAN_POINT('Ctrl Pts',(0.158935123982796,1.,3.99096873945862));
#40048=CARTESIAN_POINT('Ctrl Pts',(0.161200482186087,-1.,3.98371010319866));
#40049=CARTESIAN_POINT('Ctrl Pts',(0.161200482186087,1.,3.98371010319866));
#40050=CARTESIAN_POINT('Ctrl Pts',(0.163422004609998,-1.,3.97645194630944));
#40051=CARTESIAN_POINT('Ctrl Pts',(0.163422004609998,1.,3.97645194630944));
#40052=CARTESIAN_POINT('Ctrl Pts',(0.165598992851097,-1.,3.9691931362141));
#40053=CARTESIAN_POINT('Ctrl Pts',(0.165598992851097,1.,3.9691931362141));
#40054=CARTESIAN_POINT('Ctrl Pts',(0.167730547023312,-1.,3.96192990160296));
#40055=CARTESIAN_POINT('Ctrl Pts',(0.167730547023312,1.,3.96192990160296));
#40056=CARTESIAN_POINT('Ctrl Pts',(0.16981566637413,-1.,3.95465744665263));
#40057=CARTESIAN_POINT('Ctrl Pts',(0.16981566637413,1.,3.95465744665263));
#40058=CARTESIAN_POINT('Ctrl Pts',(0.171853355369232,-1.,3.94737164900861));
#40059=CARTESIAN_POINT('Ctrl Pts',(0.171853355369232,1.,3.94737164900861));
#40060=CARTESIAN_POINT('Ctrl Pts',(0.173842734974607,-1.,3.94007083096214));
#40061=CARTESIAN_POINT('Ctrl Pts',(0.173842734974607,1.,3.94007083096214));
#40062=CARTESIAN_POINT('Ctrl Pts',(0.175783136893872,-1.,3.93275726771049));
#40063=CARTESIAN_POINT('Ctrl Pts',(0.175783136893872,1.,3.93275726771049));
#40064=CARTESIAN_POINT('Ctrl Pts',(0.177674246152328,-1.,3.92543942697672));
#40065=CARTESIAN_POINT('Ctrl Pts',(0.177674246152328,1.,3.92543942697672));
#40066=CARTESIAN_POINT('Ctrl Pts',(0.179515885822894,-1.,3.91812876180948));
#40067=CARTESIAN_POINT('Ctrl Pts',(0.179515885822894,1.,3.91812876180948));
#40068=CARTESIAN_POINT('Ctrl Pts',(0.181307740731795,-1.,3.91083557557193));
#40069=CARTESIAN_POINT('Ctrl Pts',(0.181307740731795,1.,3.91083557557193));
#40070=CARTESIAN_POINT('Ctrl Pts',(0.183049081993193,-1.,3.90356488555138));
#40071=CARTESIAN_POINT('Ctrl Pts',(0.183049081993193,1.,3.90356488555138));
#40072=CARTESIAN_POINT('Ctrl Pts',(0.184738537728034,-1.,3.89631300742633));
#40073=CARTESIAN_POINT('Ctrl Pts',(0.184738537728034,1.,3.89631300742633));
#40074=CARTESIAN_POINT('Ctrl Pts',(0.186373724985263,-1.,3.88906196725817));
#40075=CARTESIAN_POINT('Ctrl Pts',(0.186373724985263,1.,3.88906196725817));
#40076=CARTESIAN_POINT('Ctrl Pts',(0.187951632512663,-1.,3.88178563496187));
#40077=CARTESIAN_POINT('Ctrl Pts',(0.187951632512663,1.,3.88178563496187));
#40078=CARTESIAN_POINT('Ctrl Pts',(0.189469253358254,-1.,3.87445976418377));
#40079=CARTESIAN_POINT('Ctrl Pts',(0.189469253358254,1.,3.87445976418377));
#40080=CARTESIAN_POINT('Ctrl Pts',(0.190924190418612,-1.,3.8670715862477));
#40081=CARTESIAN_POINT('Ctrl Pts',(0.190924190418612,1.,3.8670715862477));
#40082=CARTESIAN_POINT('Ctrl Pts',(0.192315153044979,-1.,3.85962774407652));
#40083=CARTESIAN_POINT('Ctrl Pts',(0.192315153044979,1.,3.85962774407652));
#40084=CARTESIAN_POINT('Ctrl Pts',(0.193642806777747,-1.,3.85216762264019));
#40085=CARTESIAN_POINT('Ctrl Pts',(0.193642806777747,1.,3.85216762264019));
#40086=CARTESIAN_POINT('Ctrl Pts',(0.194909009460254,-1.,3.84475203347052));
#40087=CARTESIAN_POINT('Ctrl Pts',(0.194909009460254,1.,3.84475203347052));
#40088=CARTESIAN_POINT('Ctrl Pts',(0.196115198971889,-1.,3.83743910616265));
#40089=CARTESIAN_POINT('Ctrl Pts',(0.196115198971889,1.,3.83743910616265));
#40090=CARTESIAN_POINT('Ctrl Pts',(0.197260935827375,-1.,3.83026221776488));
#40091=CARTESIAN_POINT('Ctrl Pts',(0.197260935827375,1.,3.83026221776488));
#40092=CARTESIAN_POINT('Ctrl Pts',(0.198342616900469,-1.,3.82321127348981));
#40093=CARTESIAN_POINT('Ctrl Pts',(0.198342616900469,1.,3.82321127348981));
#40094=CARTESIAN_POINT('Ctrl Pts',(0.199351525297396,-1.,3.81620203429702));
#40095=CARTESIAN_POINT('Ctrl Pts',(0.199351525297396,1.,3.81620203429702));
#40096=CARTESIAN_POINT('Ctrl Pts',(0.200274679433289,-1.,3.80909529318501));
#40097=CARTESIAN_POINT('Ctrl Pts',(0.200274679433289,1.,3.80909529318501));
#40098=CARTESIAN_POINT('Ctrl Pts',(0.201097756307251,-1.,3.80175247447171));
#40099=CARTESIAN_POINT('Ctrl Pts',(0.201097756307251,1.,3.80175247447171));
#40100=CARTESIAN_POINT('Ctrl Pts',(0.201807533800798,-1.,3.79408354187274));
#40101=CARTESIAN_POINT('Ctrl Pts',(0.201807533800798,1.,3.79408354187274));
#40102=CARTESIAN_POINT('Ctrl Pts',(0.202394260512192,-1.,3.78609175019317));
#40103=CARTESIAN_POINT('Ctrl Pts',(0.202394260512192,1.,3.78609175019317));
#40104=CARTESIAN_POINT('Ctrl Pts',(0.202854729699196,-1.,3.77793553476879));
#40105=CARTESIAN_POINT('Ctrl Pts',(0.202854729699196,1.,3.77793553476879));
#40106=CARTESIAN_POINT('Ctrl Pts',(0.203192390045337,-1.,3.76992071595267));
#40107=CARTESIAN_POINT('Ctrl Pts',(0.203192390045337,1.,3.76992071595267));
#40108=CARTESIAN_POINT('Ctrl Pts',(0.203414634707646,-1.,3.76242717937273));
#40109=CARTESIAN_POINT('Ctrl Pts',(0.203414634707646,1.,3.76242717937273));
#40110=CARTESIAN_POINT('Ctrl Pts',(0.203530796848403,-1.,3.75585118707924));
#40111=CARTESIAN_POINT('Ctrl Pts',(0.203530796848403,1.,3.75585118707924));
#40112=CARTESIAN_POINT('Ctrl Pts',(0.203550035479096,-1.,3.75054693397716));
#40113=CARTESIAN_POINT('Ctrl Pts',(0.203550035479096,1.,3.75054693397716));
#40114=CARTESIAN_POINT('Ctrl Pts',(0.203478844530229,-1.,3.74675472018582));
#40115=CARTESIAN_POINT('Ctrl Pts',(0.203478844530229,1.,3.74675472018582));
#40116=CARTESIAN_POINT('Ctrl Pts',(0.203352057956055,-1.,3.7450208092684));
#40117=CARTESIAN_POINT('Ctrl Pts',(0.203352057956055,1.,3.7450208092684));
#40118=CARTESIAN_POINT('Ctrl Pts',(0.203218215747894,-1.,3.74446880195845));
#40119=CARTESIAN_POINT('Ctrl Pts',(0.203218215747894,1.,3.74446880195845));
#40120=CARTESIAN_POINT('Ctrl Pts',(0.20311176758786,-1.,3.74443319346666));
#40121=CARTESIAN_POINT('Ctrl Pts',(0.20311176758786,1.,3.74443319346666));
#40122=CARTESIAN_POINT('Ctrl Pts',(0.203054238699719,-1.,3.74449849461127));
#40123=CARTESIAN_POINT('Ctrl Pts',(0.203054238699719,1.,3.74449849461127));
#40124=CARTESIAN_POINT('',(0.0760622897878233,1.,4.19931119685982));
#40125=CARTESIAN_POINT('Ctrl Pts',(0.0760622897878233,1.,4.19931119685982));
#40126=CARTESIAN_POINT('Ctrl Pts',(0.0767384596142192,1.,4.19789138621624));
#40127=CARTESIAN_POINT('Ctrl Pts',(0.0780873956244399,1.,4.19505112860624));
#40128=CARTESIAN_POINT('Ctrl Pts',(0.08010058871176,1.,4.19078883322483));
#40129=CARTESIAN_POINT('Ctrl Pts',(0.0827644164389507,1.,4.1851019532944));
#40130=CARTESIAN_POINT('Ctrl Pts',(0.0860600915552512,1.,4.17798698669991));
#40131=CARTESIAN_POINT('Ctrl Pts',(0.0893215560850325,1.,4.17086566491823));
#40132=CARTESIAN_POINT('Ctrl Pts',(0.0925486672167687,1.,4.16373802265942));
#40133=CARTESIAN_POINT('Ctrl Pts',(0.0957412403297065,1.,4.15660412653006));
#40134=CARTESIAN_POINT('Ctrl Pts',(0.0988990478899809,1.,4.1494640891762));
#40135=CARTESIAN_POINT('Ctrl Pts',(0.102021826577453,1.,4.14231804938737));
#40136=CARTESIAN_POINT('Ctrl Pts',(0.105109286538864,1.,4.13516614458396));
#40137=CARTESIAN_POINT('Ctrl Pts',(0.10816112052835,1.,4.12800848371386));
#40138=CARTESIAN_POINT('Ctrl Pts',(0.111177012683377,1.,4.12084512502444));
#40139=CARTESIAN_POINT('Ctrl Pts',(0.114156649609601,1.,4.11367603925313));
#40140=CARTESIAN_POINT('Ctrl Pts',(0.117099722731704,1.,4.10650113382187));
#40141=CARTESIAN_POINT('Ctrl Pts',(0.120005924388162,1.,4.09932031767243));
#40142=CARTESIAN_POINT('Ctrl Pts',(0.122874946249119,1.,4.09213355850836));
#40143=CARTESIAN_POINT('Ctrl Pts',(0.125706476822529,1.,4.08494093372315));
#40144=CARTESIAN_POINT('Ctrl Pts',(0.128500200484813,1.,4.07774270738809));
#40145=CARTESIAN_POINT('Ctrl Pts',(0.131255793548914,1.,4.07053931528579));
#40146=CARTESIAN_POINT('Ctrl Pts',(0.133972916144225,1.,4.06333121018476));
#40147=CARTESIAN_POINT('Ctrl Pts',(0.136651205046111,1.,4.05611873400122));
#40148=CARTESIAN_POINT('Ctrl Pts',(0.139290267180059,1.,4.04890199238056));
#40149=CARTESIAN_POINT('Ctrl Pts',(0.141889671485507,1.,4.04168069633842));
#40150=CARTESIAN_POINT('Ctrl Pts',(0.144448947038352,1.,4.03445411510403));
#40151=CARTESIAN_POINT('Ctrl Pts',(0.146967602878998,1.,4.02722143147048));
#40152=CARTESIAN_POINT('Ctrl Pts',(0.149445144968707,1.,4.01998203715588));
#40153=CARTESIAN_POINT('Ctrl Pts',(0.151881094022909,1.,4.01273584234684));
#40154=CARTESIAN_POINT('Ctrl Pts',(0.154275004872309,1.,4.00548360245297));
#40155=CARTESIAN_POINT('Ctrl Pts',(0.156626481393735,1.,3.99822717425869));
#40156=CARTESIAN_POINT('Ctrl Pts',(0.158935123982796,1.,3.99096873945862));
#40157=CARTESIAN_POINT('Ctrl Pts',(0.161200482186087,1.,3.98371010319866));
#40158=CARTESIAN_POINT('Ctrl Pts',(0.163422004609998,1.,3.97645194630944));
#40159=CARTESIAN_POINT('Ctrl Pts',(0.165598992851097,1.,3.9691931362141));
#40160=CARTESIAN_POINT('Ctrl Pts',(0.167730547023312,1.,3.96192990160296));
#40161=CARTESIAN_POINT('Ctrl Pts',(0.16981566637413,1.,3.95465744665263));
#40162=CARTESIAN_POINT('Ctrl Pts',(0.171853355369232,1.,3.94737164900861));
#40163=CARTESIAN_POINT('Ctrl Pts',(0.173842734974607,1.,3.94007083096214));
#40164=CARTESIAN_POINT('Ctrl Pts',(0.175783136893872,1.,3.93275726771049));
#40165=CARTESIAN_POINT('Ctrl Pts',(0.177674246152328,1.,3.92543942697672));
#40166=CARTESIAN_POINT('Ctrl Pts',(0.179515885822894,1.,3.91812876180948));
#40167=CARTESIAN_POINT('Ctrl Pts',(0.181307740731795,1.,3.91083557557193));
#40168=CARTESIAN_POINT('Ctrl Pts',(0.183049081993193,1.,3.90356488555138));
#40169=CARTESIAN_POINT('Ctrl Pts',(0.184738537728034,1.,3.89631300742633));
#40170=CARTESIAN_POINT('Ctrl Pts',(0.186373724985263,1.,3.88906196725817));
#40171=CARTESIAN_POINT('Ctrl Pts',(0.187951632512663,1.,3.88178563496187));
#40172=CARTESIAN_POINT('Ctrl Pts',(0.189469253358254,1.,3.87445976418377));
#40173=CARTESIAN_POINT('Ctrl Pts',(0.190924190418612,1.,3.8670715862477));
#40174=CARTESIAN_POINT('Ctrl Pts',(0.192315153044979,1.,3.85962774407652));
#40175=CARTESIAN_POINT('Ctrl Pts',(0.193642806777747,1.,3.85216762264019));
#40176=CARTESIAN_POINT('Ctrl Pts',(0.194909009460254,1.,3.84475203347052));
#40177=CARTESIAN_POINT('Ctrl Pts',(0.196115198971889,1.,3.83743910616265));
#40178=CARTESIAN_POINT('Ctrl Pts',(0.197260935827375,1.,3.83026221776488));
#40179=CARTESIAN_POINT('Ctrl Pts',(0.198342616900469,1.,3.82321127348981));
#40180=CARTESIAN_POINT('Ctrl Pts',(0.199351525297396,1.,3.81620203429702));
#40181=CARTESIAN_POINT('Ctrl Pts',(0.200274679433289,1.,3.80909529318501));
#40182=CARTESIAN_POINT('Ctrl Pts',(0.201097756307251,1.,3.80175247447171));
#40183=CARTESIAN_POINT('Ctrl Pts',(0.201807533800798,1.,3.79408354187274));
#40184=CARTESIAN_POINT('Ctrl Pts',(0.202394260512192,1.,3.78609175019317));
#40185=CARTESIAN_POINT('Ctrl Pts',(0.202854729699196,1.,3.77793553476879));
#40186=CARTESIAN_POINT('Ctrl Pts',(0.203192390045337,1.,3.76992071595267));
#40187=CARTESIAN_POINT('Ctrl Pts',(0.203414634707646,1.,3.76242717937273));
#40188=CARTESIAN_POINT('Ctrl Pts',(0.203530796848403,1.,3.75585118707924));
#40189=CARTESIAN_POINT('Ctrl Pts',(0.203550035479096,1.,3.75054693397716));
#40190=CARTESIAN_POINT('Ctrl Pts',(0.203484186269314,1.,3.74703926501843));
#40191=CARTESIAN_POINT('Ctrl Pts',(0.203375226874331,1.,3.74535749969262));
#40192=CARTESIAN_POINT('Ctrl Pts',(0.203266610111263,1.,3.74471097893961));
#40193=CARTESIAN_POINT('Ctrl Pts',(0.203188003947964,1.,3.74453008995129));
#40194=CARTESIAN_POINT('Ctrl Pts',(0.203156094897895,1.,3.74449296982994));
#40195=CARTESIAN_POINT('',(0.0760622897878233,0.,4.19931119685982));
#40196=CARTESIAN_POINT('Ctrl Pts',(-0.20305423869972,-1.,3.74449849461127));
#40197=CARTESIAN_POINT('Ctrl Pts',(-0.20305423869972,1.,3.74449849461127));
#40198=CARTESIAN_POINT('Ctrl Pts',(-0.203111767587923,-1.,3.7444331934681));
#40199=CARTESIAN_POINT('Ctrl Pts',(-0.203111767587923,1.,3.7444331934681));
#40200=CARTESIAN_POINT('Ctrl Pts',(-0.203218215748059,-1.,3.7444688019622));
#40201=CARTESIAN_POINT('Ctrl Pts',(-0.203218215748059,1.,3.7444688019622));
#40202=CARTESIAN_POINT('Ctrl Pts',(-0.203352057956297,-1.,3.74502080927395));
#40203=CARTESIAN_POINT('Ctrl Pts',(-0.203352057956297,1.,3.74502080927395));
#40204=CARTESIAN_POINT('Ctrl Pts',(-0.203478844530447,-1.,3.7467547201908));
#40205=CARTESIAN_POINT('Ctrl Pts',(-0.203478844530447,1.,3.7467547201908));
#40206=CARTESIAN_POINT('Ctrl Pts',(-0.203550035479166,-1.,3.75054693397875));
#40207=CARTESIAN_POINT('Ctrl Pts',(-0.203550035479166,1.,3.75054693397875));
#40208=CARTESIAN_POINT('Ctrl Pts',(-0.203530796848322,-1.,3.75585118707734));
#40209=CARTESIAN_POINT('Ctrl Pts',(-0.203530796848322,1.,3.75585118707734));
#40210=CARTESIAN_POINT('Ctrl Pts',(-0.203414634707479,-1.,3.76242717936885));
#40211=CARTESIAN_POINT('Ctrl Pts',(-0.203414634707479,1.,3.76242717936885));
#40212=CARTESIAN_POINT('Ctrl Pts',(-0.203192390045165,-1.,3.7699207159487));
#40213=CARTESIAN_POINT('Ctrl Pts',(-0.203192390045165,1.,3.7699207159487));
#40214=CARTESIAN_POINT('Ctrl Pts',(-0.202854729699081,-1.,3.77793553476614));
#40215=CARTESIAN_POINT('Ctrl Pts',(-0.202854729699081,1.,3.77793553476614));
#40216=CARTESIAN_POINT('Ctrl Pts',(-0.20239426051216,-1.,3.78609175019242));
#40217=CARTESIAN_POINT('Ctrl Pts',(-0.20239426051216,1.,3.78609175019242));
#40218=CARTESIAN_POINT('Ctrl Pts',(-0.201807533800837,-1.,3.7940835418736));
#40219=CARTESIAN_POINT('Ctrl Pts',(-0.201807533800837,1.,3.7940835418736));
#40220=CARTESIAN_POINT('Ctrl Pts',(-0.201097756307326,-1.,3.80175247447337));
#40221=CARTESIAN_POINT('Ctrl Pts',(-0.201097756307326,1.,3.80175247447337));
#40222=CARTESIAN_POINT('Ctrl Pts',(-0.200274679433365,-1.,3.80909529318669));
#40223=CARTESIAN_POINT('Ctrl Pts',(-0.200274679433365,1.,3.80909529318669));
#40224=CARTESIAN_POINT('Ctrl Pts',(-0.199351525297447,-1.,3.81620203429815));
#40225=CARTESIAN_POINT('Ctrl Pts',(-0.199351525297447,1.,3.81620203429815));
#40226=CARTESIAN_POINT('Ctrl Pts',(-0.198342616900487,-1.,3.82321127349016));
#40227=CARTESIAN_POINT('Ctrl Pts',(-0.198342616900487,1.,3.82321127349016));
#40228=CARTESIAN_POINT('Ctrl Pts',(-0.197260935827362,-1.,3.83026221776456));
#40229=CARTESIAN_POINT('Ctrl Pts',(-0.197260935827362,1.,3.83026221776456));
#40230=CARTESIAN_POINT('Ctrl Pts',(-0.196115198971859,-1.,3.83743910616195));
#40231=CARTESIAN_POINT('Ctrl Pts',(-0.196115198971859,1.,3.83743910616195));
#40232=CARTESIAN_POINT('Ctrl Pts',(-0.194909009460221,-1.,3.84475203346977));
#40233=CARTESIAN_POINT('Ctrl Pts',(-0.194909009460221,1.,3.84475203346977));
#40234=CARTESIAN_POINT('Ctrl Pts',(-0.193642806777723,-1.,3.85216762263966));
#40235=CARTESIAN_POINT('Ctrl Pts',(-0.193642806777723,1.,3.85216762263966));
#40236=CARTESIAN_POINT('Ctrl Pts',(-0.192315153044971,-1.,3.85962774407633));
#40237=CARTESIAN_POINT('Ctrl Pts',(-0.192315153044971,1.,3.85962774407633));
#40238=CARTESIAN_POINT('Ctrl Pts',(-0.19092419041862,-1.,3.86707158624783));
#40239=CARTESIAN_POINT('Ctrl Pts',(-0.19092419041862,1.,3.86707158624783));
#40240=CARTESIAN_POINT('Ctrl Pts',(-0.189469253358273,-1.,3.87445976418412));
#40241=CARTESIAN_POINT('Ctrl Pts',(-0.189469253358273,1.,3.87445976418412));
#40242=CARTESIAN_POINT('Ctrl Pts',(-0.187951632512685,-1.,3.88178563496228));
#40243=CARTESIAN_POINT('Ctrl Pts',(-0.187951632512685,1.,3.88178563496228));
#40244=CARTESIAN_POINT('Ctrl Pts',(-0.186373724985281,-1.,3.88906196725848));
#40245=CARTESIAN_POINT('Ctrl Pts',(-0.186373724985281,1.,3.88906196725848));
#40246=CARTESIAN_POINT('Ctrl Pts',(-0.184738537728043,-1.,3.89631300742646));
#40247=CARTESIAN_POINT('Ctrl Pts',(-0.184738537728043,1.,3.89631300742646));
#40248=CARTESIAN_POINT('Ctrl Pts',(-0.183049081993191,-1.,3.90356488555132));
#40249=CARTESIAN_POINT('Ctrl Pts',(-0.183049081993191,1.,3.90356488555132));
#40250=CARTESIAN_POINT('Ctrl Pts',(-0.181307740731786,-1.,3.91083557557175));
#40251=CARTESIAN_POINT('Ctrl Pts',(-0.181307740731786,1.,3.91083557557175));
#40252=CARTESIAN_POINT('Ctrl Pts',(-0.179515885822882,-1.,3.91812876180926));
#40253=CARTESIAN_POINT('Ctrl Pts',(-0.179515885822882,1.,3.91812876180926));
#40254=CARTESIAN_POINT('Ctrl Pts',(-0.177674246152318,-1.,3.92543942697655));
#40255=CARTESIAN_POINT('Ctrl Pts',(-0.177674246152318,1.,3.92543942697655));
#40256=CARTESIAN_POINT('Ctrl Pts',(-0.175783136893868,-1.,3.93275726771042));
#40257=CARTESIAN_POINT('Ctrl Pts',(-0.175783136893868,1.,3.93275726771042));
#40258=CARTESIAN_POINT('Ctrl Pts',(-0.17384273497461,-1.,3.94007083096217));
#40259=CARTESIAN_POINT('Ctrl Pts',(-0.17384273497461,1.,3.94007083096217));
#40260=CARTESIAN_POINT('Ctrl Pts',(-0.17185335536924,-1.,3.94737164900868));
#40261=CARTESIAN_POINT('Ctrl Pts',(-0.17185335536924,1.,3.94737164900868));
#40262=CARTESIAN_POINT('Ctrl Pts',(-0.169815666374139,-1.,3.95465744665268));
#40263=CARTESIAN_POINT('Ctrl Pts',(-0.169815666374139,1.,3.95465744665268));
#40264=CARTESIAN_POINT('Ctrl Pts',(-0.16773054702332,-1.,3.96192990160296));
#40265=CARTESIAN_POINT('Ctrl Pts',(-0.16773054702332,1.,3.96192990160296));
#40266=CARTESIAN_POINT('Ctrl Pts',(-0.165598992851102,-1.,3.96919313621407));
#40267=CARTESIAN_POINT('Ctrl Pts',(-0.165598992851102,1.,3.96919313621407));
#40268=CARTESIAN_POINT('Ctrl Pts',(-0.163422004609999,-1.,3.97645194630943));
#40269=CARTESIAN_POINT('Ctrl Pts',(-0.163422004609999,1.,3.97645194630943));
#40270=CARTESIAN_POINT('Ctrl Pts',(-0.161200482186085,-1.,3.98371010319872));
#40271=CARTESIAN_POINT('Ctrl Pts',(-0.161200482186085,1.,3.98371010319872));
#40272=CARTESIAN_POINT('Ctrl Pts',(-0.158935123982793,-1.,3.99096873945878));
#40273=CARTESIAN_POINT('Ctrl Pts',(-0.158935123982793,1.,3.99096873945878));
#40274=CARTESIAN_POINT('Ctrl Pts',(-0.156626481393734,-1.,3.99822717425893));
#40275=CARTESIAN_POINT('Ctrl Pts',(-0.156626481393734,1.,3.99822717425893));
#40276=CARTESIAN_POINT('Ctrl Pts',(-0.154275004872311,-1.,4.00548360245319));
#40277=CARTESIAN_POINT('Ctrl Pts',(-0.154275004872311,1.,4.00548360245319));
#40278=CARTESIAN_POINT('Ctrl Pts',(-0.151881094022911,-1.,4.01273584234689));
#40279=CARTESIAN_POINT('Ctrl Pts',(-0.151881094022911,1.,4.01273584234689));
#40280=CARTESIAN_POINT('Ctrl Pts',(-0.149445144968707,-1.,4.01998203715564));
#40281=CARTESIAN_POINT('Ctrl Pts',(-0.149445144968707,1.,4.01998203715564));
#40282=CARTESIAN_POINT('Ctrl Pts',(-0.146967602878994,-1.,4.02722143146994));
#40283=CARTESIAN_POINT('Ctrl Pts',(-0.146967602878994,1.,4.02722143146994));
#40284=CARTESIAN_POINT('Ctrl Pts',(-0.144448947038345,-1.,4.03445411510333));
#40285=CARTESIAN_POINT('Ctrl Pts',(-0.144448947038345,1.,4.03445411510333));
#40286=CARTESIAN_POINT('Ctrl Pts',(-0.1418896714855,-1.,4.04168069633781));
#40287=CARTESIAN_POINT('Ctrl Pts',(-0.1418896714855,1.,4.04168069633781));
#40288=CARTESIAN_POINT('Ctrl Pts',(-0.139290267180057,-1.,4.04890199238036));
#40289=CARTESIAN_POINT('Ctrl Pts',(-0.139290267180057,1.,4.04890199238036));
#40290=CARTESIAN_POINT('Ctrl Pts',(-0.136651205046119,-1.,4.05611873400172));
#40291=CARTESIAN_POINT('Ctrl Pts',(-0.136651205046119,1.,4.05611873400172));
#40292=CARTESIAN_POINT('Ctrl Pts',(-0.133972916144245,-1.,4.06333121018596));
#40293=CARTESIAN_POINT('Ctrl Pts',(-0.133972916144245,1.,4.06333121018596));
#40294=CARTESIAN_POINT('Ctrl Pts',(-0.131255793548941,-1.,4.0705393152874));
#40295=CARTESIAN_POINT('Ctrl Pts',(-0.131255793548941,1.,4.0705393152874));
#40296=CARTESIAN_POINT('Ctrl Pts',(-0.128500200484838,-1.,4.07774270738954));
#40297=CARTESIAN_POINT('Ctrl Pts',(-0.128500200484838,1.,4.07774270738954));
#40298=CARTESIAN_POINT('Ctrl Pts',(-0.12570647682254,-1.,4.08494093372377));
#40299=CARTESIAN_POINT('Ctrl Pts',(-0.12570647682254,1.,4.08494093372377));
#40300=CARTESIAN_POINT('Ctrl Pts',(-0.122874946249107,-1.,4.09213355850756));
#40301=CARTESIAN_POINT('Ctrl Pts',(-0.122874946249107,1.,4.09213355850756));
#40302=CARTESIAN_POINT('Ctrl Pts',(-0.120005924388124,-1.,4.09932031767002));
#40303=CARTESIAN_POINT('Ctrl Pts',(-0.120005924388124,1.,4.09932031767002));
#40304=CARTESIAN_POINT('Ctrl Pts',(-0.117099722731648,-1.,4.10650113381833));
#40305=CARTESIAN_POINT('Ctrl Pts',(-0.117099722731648,1.,4.10650113381833));
#40306=CARTESIAN_POINT('Ctrl Pts',(-0.114156649609546,-1.,4.11367603924961));
#40307=CARTESIAN_POINT('Ctrl Pts',(-0.114156649609546,1.,4.11367603924961));
#40308=CARTESIAN_POINT('Ctrl Pts',(-0.111177012683347,-1.,4.1208451250225));
#40309=CARTESIAN_POINT('Ctrl Pts',(-0.111177012683347,1.,4.1208451250225));
#40310=CARTESIAN_POINT('Ctrl Pts',(-0.10816112052837,-1.,4.12800848371504));
#40311=CARTESIAN_POINT('Ctrl Pts',(-0.10816112052837,1.,4.12800848371504));
#40312=CARTESIAN_POINT('Ctrl Pts',(-0.105109286538945,-1.,4.13516614458895));
#40313=CARTESIAN_POINT('Ctrl Pts',(-0.105109286538945,1.,4.13516614458895));
#40314=CARTESIAN_POINT('Ctrl Pts',(-0.102021826577584,-1.,4.14231804939538));
#40315=CARTESIAN_POINT('Ctrl Pts',(-0.102021826577584,1.,4.14231804939538));
#40316=CARTESIAN_POINT('Ctrl Pts',(-0.0988990478901228,-1.,4.14946408918485));
#40317=CARTESIAN_POINT('Ctrl Pts',(-0.0988990478901228,1.,4.14946408918485));
#40318=CARTESIAN_POINT('Ctrl Pts',(-0.0957412403298009,-1.,4.15660412653577));
#40319=CARTESIAN_POINT('Ctrl Pts',(-0.0957412403298009,1.,4.15660412653577));
#40320=CARTESIAN_POINT('Ctrl Pts',(-0.0925486672167534,-1.,4.16373802265839));
#40321=CARTESIAN_POINT('Ctrl Pts',(-0.0925486672167534,1.,4.16373802265839));
#40322=CARTESIAN_POINT('Ctrl Pts',(-0.0893215560848652,-1.,4.17086566490794));
#40323=CARTESIAN_POINT('Ctrl Pts',(-0.0893215560848652,1.,4.17086566490794));
#40324=CARTESIAN_POINT('Ctrl Pts',(-0.0860600915549399,-1.,4.17798698668094));
#40325=CARTESIAN_POINT('Ctrl Pts',(-0.0860600915549399,1.,4.17798698668094));
#40326=CARTESIAN_POINT('Ctrl Pts',(-0.0827644164385681,-1.,4.18510195327123));
#40327=CARTESIAN_POINT('Ctrl Pts',(-0.0827644164385681,1.,4.18510195327123));
#40328=CARTESIAN_POINT('Ctrl Pts',(-0.0801005887114322,-1.,4.19078883320504));
#40329=CARTESIAN_POINT('Ctrl Pts',(-0.0801005887114322,1.,4.19078883320504));
#40330=CARTESIAN_POINT('Ctrl Pts',(-0.07808739562424,-1.,4.19505112859416));
#40331=CARTESIAN_POINT('Ctrl Pts',(-0.07808739562424,1.,4.19505112859416));
#40332=CARTESIAN_POINT('Ctrl Pts',(-0.0767384596141467,-1.,4.1978913862118));
#40333=CARTESIAN_POINT('Ctrl Pts',(-0.0767384596141467,1.,4.1978913862118));
#40334=CARTESIAN_POINT('Ctrl Pts',(-0.0760622897878249,-1.,4.19931119685982));
#40335=CARTESIAN_POINT('Ctrl Pts',(-0.0760622897878249,1.,4.19931119685982));
#40336=CARTESIAN_POINT('',(-0.203156094896102,1.,3.74449296983004));
#40337=CARTESIAN_POINT('Ctrl Pts',(-0.203156094896101,-1.,3.74449296983004));
#40338=CARTESIAN_POINT('Ctrl Pts',(-0.203156094896101,-0.666666666666667,
3.74449296983004));
#40339=CARTESIAN_POINT('Ctrl Pts',(-0.203156094896101,-0.333333333333333,
3.74449296983004));
#40340=CARTESIAN_POINT('Ctrl Pts',(-0.203156094896101,0.333333333333333,
3.74449296983004));
#40341=CARTESIAN_POINT('Ctrl Pts',(-0.203156094896101,0.666666666666667,
3.74449296983004));
#40342=CARTESIAN_POINT('Ctrl Pts',(-0.203156094896101,1.,3.74449296983004));
#40343=CARTESIAN_POINT('',(-0.0760622897878249,1.,4.19931119685982));
#40344=CARTESIAN_POINT('',(-0.0760622897878249,0.,4.19931119685982));
#40345=CARTESIAN_POINT('Ctrl Pts',(-0.203156094896101,1.,3.74449296983004));
#40346=CARTESIAN_POINT('Ctrl Pts',(-0.203188003946657,1.,3.74453008995092));
#40347=CARTESIAN_POINT('Ctrl Pts',(-0.203266610110531,1.,3.74471097893845));
#40348=CARTESIAN_POINT('Ctrl Pts',(-0.203375226874122,1.,3.74535749969115));
#40349=CARTESIAN_POINT('Ctrl Pts',(-0.203484186269415,1.,3.74703926501752));
#40350=CARTESIAN_POINT('Ctrl Pts',(-0.203550035479166,1.,3.75054693397875));
#40351=CARTESIAN_POINT('Ctrl Pts',(-0.203530796848322,1.,3.75585118707734));
#40352=CARTESIAN_POINT('Ctrl Pts',(-0.203414634707479,1.,3.76242717936885));
#40353=CARTESIAN_POINT('Ctrl Pts',(-0.203192390045165,1.,3.7699207159487));
#40354=CARTESIAN_POINT('Ctrl Pts',(-0.202854729699081,1.,3.77793553476614));
#40355=CARTESIAN_POINT('Ctrl Pts',(-0.20239426051216,1.,3.78609175019242));
#40356=CARTESIAN_POINT('Ctrl Pts',(-0.201807533800837,1.,3.7940835418736));
#40357=CARTESIAN_POINT('Ctrl Pts',(-0.201097756307326,1.,3.80175247447337));
#40358=CARTESIAN_POINT('Ctrl Pts',(-0.200274679433365,1.,3.80909529318669));
#40359=CARTESIAN_POINT('Ctrl Pts',(-0.199351525297447,1.,3.81620203429815));
#40360=CARTESIAN_POINT('Ctrl Pts',(-0.198342616900487,1.,3.82321127349016));
#40361=CARTESIAN_POINT('Ctrl Pts',(-0.197260935827362,1.,3.83026221776456));
#40362=CARTESIAN_POINT('Ctrl Pts',(-0.196115198971859,1.,3.83743910616195));
#40363=CARTESIAN_POINT('Ctrl Pts',(-0.194909009460221,1.,3.84475203346977));
#40364=CARTESIAN_POINT('Ctrl Pts',(-0.193642806777723,1.,3.85216762263966));
#40365=CARTESIAN_POINT('Ctrl Pts',(-0.192315153044971,1.,3.85962774407633));
#40366=CARTESIAN_POINT('Ctrl Pts',(-0.19092419041862,1.,3.86707158624783));
#40367=CARTESIAN_POINT('Ctrl Pts',(-0.189469253358273,1.,3.87445976418412));
#40368=CARTESIAN_POINT('Ctrl Pts',(-0.187951632512685,1.,3.88178563496228));
#40369=CARTESIAN_POINT('Ctrl Pts',(-0.186373724985281,1.,3.88906196725848));
#40370=CARTESIAN_POINT('Ctrl Pts',(-0.184738537728043,1.,3.89631300742646));
#40371=CARTESIAN_POINT('Ctrl Pts',(-0.183049081993191,1.,3.90356488555132));
#40372=CARTESIAN_POINT('Ctrl Pts',(-0.181307740731786,1.,3.91083557557175));
#40373=CARTESIAN_POINT('Ctrl Pts',(-0.179515885822882,1.,3.91812876180926));
#40374=CARTESIAN_POINT('Ctrl Pts',(-0.177674246152318,1.,3.92543942697655));
#40375=CARTESIAN_POINT('Ctrl Pts',(-0.175783136893868,1.,3.93275726771042));
#40376=CARTESIAN_POINT('Ctrl Pts',(-0.17384273497461,1.,3.94007083096217));
#40377=CARTESIAN_POINT('Ctrl Pts',(-0.17185335536924,1.,3.94737164900868));
#40378=CARTESIAN_POINT('Ctrl Pts',(-0.169815666374139,1.,3.95465744665268));
#40379=CARTESIAN_POINT('Ctrl Pts',(-0.16773054702332,1.,3.96192990160296));
#40380=CARTESIAN_POINT('Ctrl Pts',(-0.165598992851102,1.,3.96919313621407));
#40381=CARTESIAN_POINT('Ctrl Pts',(-0.163422004609999,1.,3.97645194630943));
#40382=CARTESIAN_POINT('Ctrl Pts',(-0.161200482186085,1.,3.98371010319872));
#40383=CARTESIAN_POINT('Ctrl Pts',(-0.158935123982793,1.,3.99096873945878));
#40384=CARTESIAN_POINT('Ctrl Pts',(-0.156626481393734,1.,3.99822717425893));
#40385=CARTESIAN_POINT('Ctrl Pts',(-0.154275004872311,1.,4.00548360245319));
#40386=CARTESIAN_POINT('Ctrl Pts',(-0.151881094022911,1.,4.01273584234689));
#40387=CARTESIAN_POINT('Ctrl Pts',(-0.149445144968707,1.,4.01998203715564));
#40388=CARTESIAN_POINT('Ctrl Pts',(-0.146967602878994,1.,4.02722143146994));
#40389=CARTESIAN_POINT('Ctrl Pts',(-0.144448947038345,1.,4.03445411510333));
#40390=CARTESIAN_POINT('Ctrl Pts',(-0.1418896714855,1.,4.04168069633781));
#40391=CARTESIAN_POINT('Ctrl Pts',(-0.139290267180057,1.,4.04890199238036));
#40392=CARTESIAN_POINT('Ctrl Pts',(-0.136651205046119,1.,4.05611873400172));
#40393=CARTESIAN_POINT('Ctrl Pts',(-0.133972916144245,1.,4.06333121018596));
#40394=CARTESIAN_POINT('Ctrl Pts',(-0.131255793548941,1.,4.0705393152874));
#40395=CARTESIAN_POINT('Ctrl Pts',(-0.128500200484838,1.,4.07774270738954));
#40396=CARTESIAN_POINT('Ctrl Pts',(-0.12570647682254,1.,4.08494093372377));
#40397=CARTESIAN_POINT('Ctrl Pts',(-0.122874946249107,1.,4.09213355850756));
#40398=CARTESIAN_POINT('Ctrl Pts',(-0.120005924388124,1.,4.09932031767002));
#40399=CARTESIAN_POINT('Ctrl Pts',(-0.117099722731648,1.,4.10650113381833));
#40400=CARTESIAN_POINT('Ctrl Pts',(-0.114156649609546,1.,4.11367603924961));
#40401=CARTESIAN_POINT('Ctrl Pts',(-0.111177012683347,1.,4.1208451250225));
#40402=CARTESIAN_POINT('Ctrl Pts',(-0.10816112052837,1.,4.12800848371504));
#40403=CARTESIAN_POINT('Ctrl Pts',(-0.105109286538945,1.,4.13516614458895));
#40404=CARTESIAN_POINT('Ctrl Pts',(-0.102021826577584,1.,4.14231804939538));
#40405=CARTESIAN_POINT('Ctrl Pts',(-0.0988990478901228,1.,4.14946408918485));
#40406=CARTESIAN_POINT('Ctrl Pts',(-0.0957412403298009,1.,4.15660412653577));
#40407=CARTESIAN_POINT('Ctrl Pts',(-0.0925486672167534,1.,4.16373802265839));
#40408=CARTESIAN_POINT('Ctrl Pts',(-0.0893215560848652,1.,4.17086566490794));
#40409=CARTESIAN_POINT('Ctrl Pts',(-0.0860600915549399,1.,4.17798698668094));
#40410=CARTESIAN_POINT('Ctrl Pts',(-0.0827644164385681,1.,4.18510195327123));
#40411=CARTESIAN_POINT('Ctrl Pts',(-0.0801005887114322,1.,4.19078883320504));
#40412=CARTESIAN_POINT('Ctrl Pts',(-0.07808739562424,1.,4.19505112859416));
#40413=CARTESIAN_POINT('Ctrl Pts',(-0.0767384596141467,1.,4.1978913862118));
#40414=CARTESIAN_POINT('Ctrl Pts',(-0.0760622897878249,1.,4.19931119685982));
#40415=CARTESIAN_POINT('Origin',(-0.0760622897878249,0.,4.19931119685982));
#40416=CARTESIAN_POINT('',(0.0760622897878233,1.,4.19931119685982));
#40417=CARTESIAN_POINT('Origin',(0.,0.,0.));
#40418=CARTESIAN_POINT('',(-0.385112848330762,1.,3.73017266276651));
#40419=CARTESIAN_POINT('Origin',(0.,1.,0.));
#40420=CARTESIAN_POINT('Ctrl Pts',(-0.385112848330762,1.,3.73017266276651));
#40421=CARTESIAN_POINT('Ctrl Pts',(-0.385112848330762,0.666666666666667,
3.73017266276651));
#40422=CARTESIAN_POINT('Ctrl Pts',(-0.385112848330762,0.333333333333333,
3.73017266276651));
#40423=CARTESIAN_POINT('Ctrl Pts',(-0.385112848330762,-0.333333333333333,
3.73017266276651));
#40424=CARTESIAN_POINT('Ctrl Pts',(-0.385112848330762,-0.666666666666667,
3.73017266276651));
#40425=CARTESIAN_POINT('Ctrl Pts',(-0.385112848330762,-1.,3.73017266276651));
#40426=CARTESIAN_POINT('Ctrl Pts',(-0.581791163835815,-1.,4.15950947128175));
#40427=CARTESIAN_POINT('Ctrl Pts',(-0.581791163835815,1.,4.15950947128175));
#40428=CARTESIAN_POINT('Ctrl Pts',(-0.580901211463535,-1.,4.1582129171283));
#40429=CARTESIAN_POINT('Ctrl Pts',(-0.580901211463535,1.,4.1582129171283));
#40430=CARTESIAN_POINT('Ctrl Pts',(-0.579124568914235,-1.,4.15561864788576));
#40431=CARTESIAN_POINT('Ctrl Pts',(-0.579124568914235,1.,4.15561864788576));
#40432=CARTESIAN_POINT('Ctrl Pts',(-0.576469391676688,-1.,4.151723761217));
#40433=CARTESIAN_POINT('Ctrl Pts',(-0.576469391676688,1.,4.151723761217));
#40434=CARTESIAN_POINT('Ctrl Pts',(-0.572948736069522,-1.,4.14652361068081));
#40435=CARTESIAN_POINT('Ctrl Pts',(-0.572948736069522,1.,4.14652361068081));
#40436=CARTESIAN_POINT('Ctrl Pts',(-0.568580610189775,-1.,4.14001179830547));
#40437=CARTESIAN_POINT('Ctrl Pts',(-0.568580610189775,1.,4.14001179830547));
#40438=CARTESIAN_POINT('Ctrl Pts',(-0.564245279537149,-1.,4.13348835727104));
#40439=CARTESIAN_POINT('Ctrl Pts',(-0.564245279537149,1.,4.13348835727104));
#40440=CARTESIAN_POINT('Ctrl Pts',(-0.559942890594774,-1.,4.12695329951961));
#40441=CARTESIAN_POINT('Ctrl Pts',(-0.559942890594774,1.,4.12695329951961));
#40442=CARTESIAN_POINT('Ctrl Pts',(-0.555673636129977,-1.,4.12040666195664));
#40443=CARTESIAN_POINT('Ctrl Pts',(-0.555673636129977,1.,4.12040666195664));
#40444=CARTESIAN_POINT('Ctrl Pts',(-0.551437758497033,-1.,4.11384852024721));
#40445=CARTESIAN_POINT('Ctrl Pts',(-0.551437758497033,1.,4.11384852024721));
#40446=CARTESIAN_POINT('Ctrl Pts',(-0.547235539485637,-1.,4.10727897027977));
#40447=CARTESIAN_POINT('Ctrl Pts',(-0.547235539485637,1.,4.10727897027977));
#40448=CARTESIAN_POINT('Ctrl Pts',(-0.543067286877757,-1.,4.10069810243979));
#40449=CARTESIAN_POINT('Ctrl Pts',(-0.543067286877757,1.,4.10069810243979));
#40450=CARTESIAN_POINT('Ctrl Pts',(-0.538933321179756,-1.,4.09410597627));
#40451=CARTESIAN_POINT('Ctrl Pts',(-0.538933321179756,1.,4.09410597627));
#40452=CARTESIAN_POINT('Ctrl Pts',(-0.534833963477273,-1.,4.08750259988885));
#40453=CARTESIAN_POINT('Ctrl Pts',(-0.534833963477273,1.,4.08750259988885));
#40454=CARTESIAN_POINT('Ctrl Pts',(-0.530769518728571,-1.,4.08088789536836));
#40455=CARTESIAN_POINT('Ctrl Pts',(-0.530769518728571,1.,4.08088789536836));
#40456=CARTESIAN_POINT('Ctrl Pts',(-0.526740277227498,-1.,4.07426172299847));
#40457=CARTESIAN_POINT('Ctrl Pts',(-0.526740277227498,1.,4.07426172299847));
#40458=CARTESIAN_POINT('Ctrl Pts',(-0.522746528603107,-1.,4.06762394471314));
#40459=CARTESIAN_POINT('Ctrl Pts',(-0.522746528603107,1.,4.06762394471314));
#40460=CARTESIAN_POINT('Ctrl Pts',(-0.518788572336924,-1.,4.06097448038013));
#40461=CARTESIAN_POINT('Ctrl Pts',(-0.518788572336924,1.,4.06097448038013));
#40462=CARTESIAN_POINT('Ctrl Pts',(-0.514866728193017,-1.,4.05431335771199));
#40463=CARTESIAN_POINT('Ctrl Pts',(-0.514866728193017,1.,4.05431335771199));
#40464=CARTESIAN_POINT('Ctrl Pts',(-0.51098134921897,-1.,4.04764078815447));
#40465=CARTESIAN_POINT('Ctrl Pts',(-0.51098134921897,1.,4.04764078815447));
#40466=CARTESIAN_POINT('Ctrl Pts',(-0.507132823288136,-1.,4.04095715148915));
#40467=CARTESIAN_POINT('Ctrl Pts',(-0.507132823288136,1.,4.04095715148915));
#40468=CARTESIAN_POINT('Ctrl Pts',(-0.503321556915346,-1.,4.03426284174272));
#40469=CARTESIAN_POINT('Ctrl Pts',(-0.503321556915346,1.,4.03426284174272));
#40470=CARTESIAN_POINT('Ctrl Pts',(-0.499547962340821,-1.,4.02755813980101));
#40471=CARTESIAN_POINT('Ctrl Pts',(-0.499547962340821,1.,4.02755813980101));
#40472=CARTESIAN_POINT('Ctrl Pts',(-0.495812444326251,-1.,4.02084308851832));
#40473=CARTESIAN_POINT('Ctrl Pts',(-0.495812444326251,1.,4.02084308851832));
#40474=CARTESIAN_POINT('Ctrl Pts',(-0.492115383418018,-1.,4.01411733503546));
#40475=CARTESIAN_POINT('Ctrl Pts',(-0.492115383418018,1.,4.01411733503546));
#40476=CARTESIAN_POINT('Ctrl Pts',(-0.488457130424633,-1.,4.0073800839099));
#40477=CARTESIAN_POINT('Ctrl Pts',(-0.488457130424633,1.,4.0073800839099));
#40478=CARTESIAN_POINT('Ctrl Pts',(-0.484838042421835,-1.,4.00063045119288));
#40479=CARTESIAN_POINT('Ctrl Pts',(-0.484838042421835,1.,4.00063045119288));
#40480=CARTESIAN_POINT('Ctrl Pts',(-0.481258512209675,-1.,3.99386775880679));
#40481=CARTESIAN_POINT('Ctrl Pts',(-0.481258512209675,1.,3.99386775880679));
#40482=CARTESIAN_POINT('Ctrl Pts',(-0.477718999122027,-1.,3.98709184306738));
#40483=CARTESIAN_POINT('Ctrl Pts',(-0.477718999122027,1.,3.98709184306738));
#40484=CARTESIAN_POINT('Ctrl Pts',(-0.47422006101951,-1.,3.98030338044409));
#40485=CARTESIAN_POINT('Ctrl Pts',(-0.47422006101951,1.,3.98030338044409));
#40486=CARTESIAN_POINT('Ctrl Pts',(-0.470762379613439,-1.,3.97350414289392));
#40487=CARTESIAN_POINT('Ctrl Pts',(-0.470762379613439,1.,3.97350414289392));
#40488=CARTESIAN_POINT('Ctrl Pts',(-0.467346690880643,-1.,3.9666962227393));
#40489=CARTESIAN_POINT('Ctrl Pts',(-0.467346690880643,1.,3.9666962227393));
#40490=CARTESIAN_POINT('Ctrl Pts',(-0.463973722115733,-1.,3.95988133243538));
#40491=CARTESIAN_POINT('Ctrl Pts',(-0.463973722115733,1.,3.95988133243538));
#40492=CARTESIAN_POINT('Ctrl Pts',(-0.460644124429121,-1.,3.95306005817364));
#40493=CARTESIAN_POINT('Ctrl Pts',(-0.460644124429121,1.,3.95306005817364));
#40494=CARTESIAN_POINT('Ctrl Pts',(-0.457358410451683,-1.,3.94623117206678));
#40495=CARTESIAN_POINT('Ctrl Pts',(-0.457358410451683,1.,3.94623117206678));
#40496=CARTESIAN_POINT('Ctrl Pts',(-0.454116879027584,-1.,3.93939080846298));
#40497=CARTESIAN_POINT('Ctrl Pts',(-0.454116879027584,1.,3.93939080846298));
#40498=CARTESIAN_POINT('Ctrl Pts',(-0.450919768356348,-1.,3.93253407403123));
#40499=CARTESIAN_POINT('Ctrl Pts',(-0.450919768356348,1.,3.93253407403123));
#40500=CARTESIAN_POINT('Ctrl Pts',(-0.447767416837293,-1.,3.92565674143416));
#40501=CARTESIAN_POINT('Ctrl Pts',(-0.447767416837293,1.,3.92565674143416));
#40502=CARTESIAN_POINT('Ctrl Pts',(-0.444660430230591,-1.,3.91875701610719));
#40503=CARTESIAN_POINT('Ctrl Pts',(-0.444660430230591,1.,3.91875701610719));
#40504=CARTESIAN_POINT('Ctrl Pts',(-0.441599824524054,-1.,3.91183704069153));
#40505=CARTESIAN_POINT('Ctrl Pts',(-0.441599824524054,1.,3.91183704069153));
#40506=CARTESIAN_POINT('Ctrl Pts',(-0.43858723545825,-1.,3.90490512938563));
#40507=CARTESIAN_POINT('Ctrl Pts',(-0.43858723545825,1.,3.90490512938563));
#40508=CARTESIAN_POINT('Ctrl Pts',(-0.435624629433528,-1.,3.89797256655462));
#40509=CARTESIAN_POINT('Ctrl Pts',(-0.435624629433528,1.,3.89797256655462));
#40510=CARTESIAN_POINT('Ctrl Pts',(-0.432713929544458,-1.,3.89104947940611));
#40511=CARTESIAN_POINT('Ctrl Pts',(-0.432713929544458,1.,3.89104947940611));
#40512=CARTESIAN_POINT('Ctrl Pts',(-0.429856640579741,-1.,3.88414070943341));
#40513=CARTESIAN_POINT('Ctrl Pts',(-0.429856640579741,1.,3.88414070943341));
#40514=CARTESIAN_POINT('Ctrl Pts',(-0.427053541173457,-1.,3.87724240306597));
#40515=CARTESIAN_POINT('Ctrl Pts',(-0.427053541173457,1.,3.87724240306597));
#40516=CARTESIAN_POINT('Ctrl Pts',(-0.424304173195111,-1.,3.87033643487851));
#40517=CARTESIAN_POINT('Ctrl Pts',(-0.424304173195111,1.,3.87033643487851));
#40518=CARTESIAN_POINT('Ctrl Pts',(-0.421607423177534,-1.,3.86339652542709));
#40519=CARTESIAN_POINT('Ctrl Pts',(-0.421607423177534,1.,3.86339652542709));
#40520=CARTESIAN_POINT('Ctrl Pts',(-0.418962468086773,-1.,3.85639825647996));
#40521=CARTESIAN_POINT('Ctrl Pts',(-0.418962468086773,1.,3.85639825647996));
#40522=CARTESIAN_POINT('Ctrl Pts',(-0.416369678052907,-1.,3.84932864157497));
#40523=CARTESIAN_POINT('Ctrl Pts',(-0.416369678052907,1.,3.84932864157497));
#40524=CARTESIAN_POINT('Ctrl Pts',(-0.413831367016748,-1.,3.84219403994762));
#40525=CARTESIAN_POINT('Ctrl Pts',(-0.413831367016748,1.,3.84219403994762));
#40526=CARTESIAN_POINT('Ctrl Pts',(-0.411353038798519,-1.,3.83503345578698));
#40527=CARTESIAN_POINT('Ctrl Pts',(-0.411353038798519,1.,3.83503345578698));
#40528=CARTESIAN_POINT('Ctrl Pts',(-0.40894237144746,-1.,3.82790724256471));
#40529=CARTESIAN_POINT('Ctrl Pts',(-0.40894237144746,1.,3.82790724256471));
#40530=CARTESIAN_POINT('Ctrl Pts',(-0.406607038258985,-1.,3.8208730391381));
#40531=CARTESIAN_POINT('Ctrl Pts',(-0.406607038258985,1.,3.8208730391381));
#40532=CARTESIAN_POINT('Ctrl Pts',(-0.404352694628273,-1.,3.81396374287793));
#40533=CARTESIAN_POINT('Ctrl Pts',(-0.404352694628273,1.,3.81396374287793));
#40534=CARTESIAN_POINT('Ctrl Pts',(-0.402181320148436,-1.,3.80716881962728));
#40535=CARTESIAN_POINT('Ctrl Pts',(-0.402181320148436,1.,3.80716881962728));
#40536=CARTESIAN_POINT('Ctrl Pts',(-0.4000883465046,-1.,3.80040370384546));
#40537=CARTESIAN_POINT('Ctrl Pts',(-0.4000883465046,1.,3.80040370384546));
#40538=CARTESIAN_POINT('Ctrl Pts',(-0.39806481868397,-1.,3.7935288716329));
#40539=CARTESIAN_POINT('Ctrl Pts',(-0.39806481868397,1.,3.7935288716329));
#40540=CARTESIAN_POINT('Ctrl Pts',(-0.396103205334841,-1.,3.78640521279313));
#40541=CARTESIAN_POINT('Ctrl Pts',(-0.396103205334841,1.,3.78640521279313));
#40542=CARTESIAN_POINT('Ctrl Pts',(-0.394202481011499,-1.,3.77894173114283));
#40543=CARTESIAN_POINT('Ctrl Pts',(-0.394202481011499,1.,3.77894173114283));
#40544=CARTESIAN_POINT('Ctrl Pts',(-0.392372786223433,-1.,3.77114011595967));
#40545=CARTESIAN_POINT('Ctrl Pts',(-0.392372786223433,1.,3.77114011595967));
#40546=CARTESIAN_POINT('Ctrl Pts',(-0.39064207297956,-1.,3.76315635033257));
#40547=CARTESIAN_POINT('Ctrl Pts',(-0.39064207297956,1.,3.76315635033257));
#40548=CARTESIAN_POINT('Ctrl Pts',(-0.389054775898702,-1.,3.75529302895152));
#40549=CARTESIAN_POINT('Ctrl Pts',(-0.389054775898702,1.,3.75529302895152));
#40550=CARTESIAN_POINT('Ctrl Pts',(-0.387663020050836,-1.,3.74792651696654));
#40551=CARTESIAN_POINT('Ctrl Pts',(-0.387663020050836,1.,3.74792651696654));
#40552=CARTESIAN_POINT('Ctrl Pts',(-0.386519576222251,-1.,3.74144965781276));
#40553=CARTESIAN_POINT('Ctrl Pts',(-0.386519576222251,1.,3.74144965781276));
#40554=CARTESIAN_POINT('Ctrl Pts',(-0.385670806454566,-1.,3.73621371845318));
#40555=CARTESIAN_POINT('Ctrl Pts',(-0.385670806454566,1.,3.73621371845318));
#40556=CARTESIAN_POINT('Ctrl Pts',(-0.385147887988951,-1.,3.73245705638843));
#40557=CARTESIAN_POINT('Ctrl Pts',(-0.385147887988951,1.,3.73245705638843));
#40558=CARTESIAN_POINT('Ctrl Pts',(-0.385001870183213,-1.,3.73072465900175));
#40559=CARTESIAN_POINT('Ctrl Pts',(-0.385001870183213,1.,3.73072465900175));
#40560=CARTESIAN_POINT('Ctrl Pts',(-0.385047711603462,-1.,3.73015851028356));
#40561=CARTESIAN_POINT('Ctrl Pts',(-0.385047711603462,1.,3.73015851028356));
#40562=CARTESIAN_POINT('Ctrl Pts',(-0.385147278814642,-1.,3.73010668803042));
#40563=CARTESIAN_POINT('Ctrl Pts',(-0.385147278814642,1.,3.73010668803042));
#40564=CARTESIAN_POINT('Ctrl Pts',(-0.38521431477633,-1.,3.73016218570874));
#40565=CARTESIAN_POINT('Ctrl Pts',(-0.38521431477633,1.,3.73016218570874));
#40566=CARTESIAN_POINT('',(-0.581791163835815,1.,4.15950947128175));
#40567=CARTESIAN_POINT('Ctrl Pts',(-0.581791163835815,1.,4.15950947128175));
#40568=CARTESIAN_POINT('Ctrl Pts',(-0.580901211463535,1.,4.1582129171283));
#40569=CARTESIAN_POINT('Ctrl Pts',(-0.579124568914235,1.,4.15561864788576));
#40570=CARTESIAN_POINT('Ctrl Pts',(-0.576469391676688,1.,4.151723761217));
#40571=CARTESIAN_POINT('Ctrl Pts',(-0.572948736069522,1.,4.14652361068081));
#40572=CARTESIAN_POINT('Ctrl Pts',(-0.568580610189775,1.,4.14001179830547));
#40573=CARTESIAN_POINT('Ctrl Pts',(-0.564245279537149,1.,4.13348835727104));
#40574=CARTESIAN_POINT('Ctrl Pts',(-0.559942890594774,1.,4.12695329951961));
#40575=CARTESIAN_POINT('Ctrl Pts',(-0.555673636129977,1.,4.12040666195664));
#40576=CARTESIAN_POINT('Ctrl Pts',(-0.551437758497033,1.,4.11384852024721));
#40577=CARTESIAN_POINT('Ctrl Pts',(-0.547235539485637,1.,4.10727897027977));
#40578=CARTESIAN_POINT('Ctrl Pts',(-0.543067286877757,1.,4.10069810243979));
#40579=CARTESIAN_POINT('Ctrl Pts',(-0.538933321179756,1.,4.09410597627));
#40580=CARTESIAN_POINT('Ctrl Pts',(-0.534833963477273,1.,4.08750259988885));
#40581=CARTESIAN_POINT('Ctrl Pts',(-0.530769518728571,1.,4.08088789536836));
#40582=CARTESIAN_POINT('Ctrl Pts',(-0.526740277227498,1.,4.07426172299847));
#40583=CARTESIAN_POINT('Ctrl Pts',(-0.522746528603107,1.,4.06762394471314));
#40584=CARTESIAN_POINT('Ctrl Pts',(-0.518788572336924,1.,4.06097448038013));
#40585=CARTESIAN_POINT('Ctrl Pts',(-0.514866728193017,1.,4.05431335771199));
#40586=CARTESIAN_POINT('Ctrl Pts',(-0.51098134921897,1.,4.04764078815447));
#40587=CARTESIAN_POINT('Ctrl Pts',(-0.507132823288136,1.,4.04095715148915));
#40588=CARTESIAN_POINT('Ctrl Pts',(-0.503321556915346,1.,4.03426284174272));
#40589=CARTESIAN_POINT('Ctrl Pts',(-0.499547962340821,1.,4.02755813980101));
#40590=CARTESIAN_POINT('Ctrl Pts',(-0.495812444326251,1.,4.02084308851832));
#40591=CARTESIAN_POINT('Ctrl Pts',(-0.492115383418018,1.,4.01411733503546));
#40592=CARTESIAN_POINT('Ctrl Pts',(-0.488457130424633,1.,4.0073800839099));
#40593=CARTESIAN_POINT('Ctrl Pts',(-0.484838042421835,1.,4.00063045119288));
#40594=CARTESIAN_POINT('Ctrl Pts',(-0.481258512209675,1.,3.99386775880679));
#40595=CARTESIAN_POINT('Ctrl Pts',(-0.477718999122027,1.,3.98709184306738));
#40596=CARTESIAN_POINT('Ctrl Pts',(-0.47422006101951,1.,3.98030338044409));
#40597=CARTESIAN_POINT('Ctrl Pts',(-0.470762379613439,1.,3.97350414289392));
#40598=CARTESIAN_POINT('Ctrl Pts',(-0.467346690880643,1.,3.9666962227393));
#40599=CARTESIAN_POINT('Ctrl Pts',(-0.463973722115733,1.,3.95988133243538));
#40600=CARTESIAN_POINT('Ctrl Pts',(-0.460644124429121,1.,3.95306005817364));
#40601=CARTESIAN_POINT('Ctrl Pts',(-0.457358410451683,1.,3.94623117206678));
#40602=CARTESIAN_POINT('Ctrl Pts',(-0.454116879027584,1.,3.93939080846298));
#40603=CARTESIAN_POINT('Ctrl Pts',(-0.450919768356348,1.,3.93253407403123));
#40604=CARTESIAN_POINT('Ctrl Pts',(-0.447767416837293,1.,3.92565674143416));
#40605=CARTESIAN_POINT('Ctrl Pts',(-0.444660430230591,1.,3.91875701610719));
#40606=CARTESIAN_POINT('Ctrl Pts',(-0.441599824524054,1.,3.91183704069153));
#40607=CARTESIAN_POINT('Ctrl Pts',(-0.43858723545825,1.,3.90490512938563));
#40608=CARTESIAN_POINT('Ctrl Pts',(-0.435624629433528,1.,3.89797256655462));
#40609=CARTESIAN_POINT('Ctrl Pts',(-0.432713929544458,1.,3.89104947940611));
#40610=CARTESIAN_POINT('Ctrl Pts',(-0.429856640579741,1.,3.88414070943341));
#40611=CARTESIAN_POINT('Ctrl Pts',(-0.427053541173457,1.,3.87724240306597));
#40612=CARTESIAN_POINT('Ctrl Pts',(-0.424304173195111,1.,3.87033643487851));
#40613=CARTESIAN_POINT('Ctrl Pts',(-0.421607423177534,1.,3.86339652542709));
#40614=CARTESIAN_POINT('Ctrl Pts',(-0.418962468086773,1.,3.85639825647996));
#40615=CARTESIAN_POINT('Ctrl Pts',(-0.416369678052907,1.,3.84932864157497));
#40616=CARTESIAN_POINT('Ctrl Pts',(-0.413831367016748,1.,3.84219403994762));
#40617=CARTESIAN_POINT('Ctrl Pts',(-0.411353038798519,1.,3.83503345578698));
#40618=CARTESIAN_POINT('Ctrl Pts',(-0.40894237144746,1.,3.82790724256471));
#40619=CARTESIAN_POINT('Ctrl Pts',(-0.406607038258985,1.,3.8208730391381));
#40620=CARTESIAN_POINT('Ctrl Pts',(-0.404352694628273,1.,3.81396374287793));
#40621=CARTESIAN_POINT('Ctrl Pts',(-0.402181320148436,1.,3.80716881962728));
#40622=CARTESIAN_POINT('Ctrl Pts',(-0.4000883465046,1.,3.80040370384546));
#40623=CARTESIAN_POINT('Ctrl Pts',(-0.39806481868397,1.,3.7935288716329));
#40624=CARTESIAN_POINT('Ctrl Pts',(-0.396103205334841,1.,3.78640521279313));
#40625=CARTESIAN_POINT('Ctrl Pts',(-0.394202481011499,1.,3.77894173114283));
#40626=CARTESIAN_POINT('Ctrl Pts',(-0.392372786223433,1.,3.77114011595967));
#40627=CARTESIAN_POINT('Ctrl Pts',(-0.39064207297956,1.,3.76315635033257));
#40628=CARTESIAN_POINT('Ctrl Pts',(-0.389054775898702,1.,3.75529302895152));
#40629=CARTESIAN_POINT('Ctrl Pts',(-0.387663020050836,1.,3.74792651696654));
#40630=CARTESIAN_POINT('Ctrl Pts',(-0.386519576222251,1.,3.74144965781276));
#40631=CARTESIAN_POINT('Ctrl Pts',(-0.385670806454566,1.,3.73621371845318));
#40632=CARTESIAN_POINT('Ctrl Pts',(-0.385187124634206,1.,3.73273893363406));
#40633=CARTESIAN_POINT('Ctrl Pts',(-0.385031656499164,1.,3.73106082862548));
#40634=CARTESIAN_POINT('Ctrl Pts',(-0.385037797881504,1.,3.73040527621055));
#40635=CARTESIAN_POINT('Ctrl Pts',(-0.385087139000375,1.,3.73021431755274));
#40636=CARTESIAN_POINT('Ctrl Pts',(-0.385112848330762,1.,3.73017266276651));
#40637=CARTESIAN_POINT('',(-0.581791163835815,0.,4.15950947128175));
#40638=CARTESIAN_POINT('Ctrl Pts',(-0.7863229229206,-1.,3.66663282329846));
#40639=CARTESIAN_POINT('Ctrl Pts',(-0.7863229229206,1.,3.66663282329846));
#40640=CARTESIAN_POINT('Ctrl Pts',(-0.786369528183326,-1.,3.66655932661986));
#40641=CARTESIAN_POINT('Ctrl Pts',(-0.786369528183326,1.,3.66655932661986));
#40642=CARTESIAN_POINT('Ctrl Pts',(-0.786480236185697,-1.,3.66657784455334));
#40643=CARTESIAN_POINT('Ctrl Pts',(-0.786480236185697,1.,3.66657784455334));
#40644=CARTESIAN_POINT('Ctrl Pts',(-0.786698783542764,-1.,3.66710211820482));
#40645=CARTESIAN_POINT('Ctrl Pts',(-0.786698783542764,1.,3.66710211820482));
#40646=CARTESIAN_POINT('Ctrl Pts',(-0.787095252590501,-1.,3.66879484801113));
#40647=CARTESIAN_POINT('Ctrl Pts',(-0.787095252590501,1.,3.66879484801113));
#40648=CARTESIAN_POINT('Ctrl Pts',(-0.787758799995743,-1.,3.67252923663655));
#40649=CARTESIAN_POINT('Ctrl Pts',(-0.787758799995743,1.,3.67252923663655));
#40650=CARTESIAN_POINT('Ctrl Pts',(-0.788569566220285,-1.,3.67777119516252));
#40651=CARTESIAN_POINT('Ctrl Pts',(-0.788569566220285,1.,3.67777119516252));
#40652=CARTESIAN_POINT('Ctrl Pts',(-0.789483546064387,-1.,3.68428439783905));
#40653=CARTESIAN_POINT('Ctrl Pts',(-0.789483546064387,1.,3.68428439783905));
#40654=CARTESIAN_POINT('Ctrl Pts',(-0.790436284988788,-1.,3.69172044327364));
#40655=CARTESIAN_POINT('Ctrl Pts',(-0.790436284988788,1.,3.69172044327364));
#40656=CARTESIAN_POINT('Ctrl Pts',(-0.79135657569598,-1.,3.69968940808721));
#40657=CARTESIAN_POINT('Ctrl Pts',(-0.79135657569598,1.,3.69968940808721));
#40658=CARTESIAN_POINT('Ctrl Pts',(-0.792177688845818,-1.,3.70781724021806));
#40659=CARTESIAN_POINT('Ctrl Pts',(-0.792177688845818,1.,3.70781724021806));
#40660=CARTESIAN_POINT('Ctrl Pts',(-0.792848377370287,-1.,3.71580242396124));
#40661=CARTESIAN_POINT('Ctrl Pts',(-0.792848377370287,1.,3.71580242396124));
#40662=CARTESIAN_POINT('Ctrl Pts',(-0.793347023784205,-1.,3.72348797293734));
#40663=CARTESIAN_POINT('Ctrl Pts',(-0.793347023784205,1.,3.72348797293734));
#40664=CARTESIAN_POINT('Ctrl Pts',(-0.793682750269684,-1.,3.73086914695805));
#40665=CARTESIAN_POINT('Ctrl Pts',(-0.793682750269684,1.,3.73086914695805));
#40666=CARTESIAN_POINT('Ctrl Pts',(-0.793882700937017,-1.,3.73803280541687));
#40667=CARTESIAN_POINT('Ctrl Pts',(-0.793882700937017,1.,3.73803280541687));
#40668=CARTESIAN_POINT('Ctrl Pts',(-0.793982700459952,-1.,3.74511357728861));
#40669=CARTESIAN_POINT('Ctrl Pts',(-0.793982700459952,1.,3.74511357728861));
#40670=CARTESIAN_POINT('Ctrl Pts',(-0.794017347371377,-1.,3.75224692493864));
#40671=CARTESIAN_POINT('Ctrl Pts',(-0.794017347371377,1.,3.75224692493864));
#40672=CARTESIAN_POINT('Ctrl Pts',(-0.794008429134907,-1.,3.75951468666257));
#40673=CARTESIAN_POINT('Ctrl Pts',(-0.794008429134907,1.,3.75951468666257));
#40674=CARTESIAN_POINT('Ctrl Pts',(-0.793961083688992,-1.,3.76692626931111));
#40675=CARTESIAN_POINT('Ctrl Pts',(-0.793961083688992,1.,3.76692626931111));
#40676=CARTESIAN_POINT('Ctrl Pts',(-0.793870523787408,-1.,3.77444863801212));
#40677=CARTESIAN_POINT('Ctrl Pts',(-0.793870523787408,1.,3.77444863801212));
#40678=CARTESIAN_POINT('Ctrl Pts',(-0.7937262357813,-1.,3.78202460377598));
#40679=CARTESIAN_POINT('Ctrl Pts',(-0.7937262357813,1.,3.78202460377598));
#40680=CARTESIAN_POINT('Ctrl Pts',(-0.793516871680993,-1.,3.78959439439235));
#40681=CARTESIAN_POINT('Ctrl Pts',(-0.793516871680993,1.,3.78959439439235));
#40682=CARTESIAN_POINT('Ctrl Pts',(-0.793235612973273,-1.,3.79711921389897));
#40683=CARTESIAN_POINT('Ctrl Pts',(-0.793235612973273,1.,3.79711921389897));
#40684=CARTESIAN_POINT('Ctrl Pts',(-0.792882695234778,-1.,3.80459229925637));
#40685=CARTESIAN_POINT('Ctrl Pts',(-0.792882695234778,1.,3.80459229925637));
#40686=CARTESIAN_POINT('Ctrl Pts',(-0.792462483517634,-1.,3.81202588694756));
#40687=CARTESIAN_POINT('Ctrl Pts',(-0.792462483517634,1.,3.81202588694756));
#40688=CARTESIAN_POINT('Ctrl Pts',(-0.791981740718635,-1.,3.81944345442249));
#40689=CARTESIAN_POINT('Ctrl Pts',(-0.791981740718635,1.,3.81944345442249));
#40690=CARTESIAN_POINT('Ctrl Pts',(-0.791447528662369,-1.,3.82687033899792));
#40691=CARTESIAN_POINT('Ctrl Pts',(-0.791447528662369,1.,3.82687033899792));
#40692=CARTESIAN_POINT('Ctrl Pts',(-0.790865012705301,-1.,3.83432392054786));
#40693=CARTESIAN_POINT('Ctrl Pts',(-0.790865012705301,1.,3.83432392054786));
#40694=CARTESIAN_POINT('Ctrl Pts',(-0.790236124191242,-1.,3.84180762342454));
#40695=CARTESIAN_POINT('Ctrl Pts',(-0.790236124191242,1.,3.84180762342454));
#40696=CARTESIAN_POINT('Ctrl Pts',(-0.789560798155582,-1.,3.84931637808894));
#40697=CARTESIAN_POINT('Ctrl Pts',(-0.789560798155582,1.,3.84931637808894));
#40698=CARTESIAN_POINT('Ctrl Pts',(-0.788837734090672,-1.,3.85683995872529));
#40699=CARTESIAN_POINT('Ctrl Pts',(-0.788837734090672,1.,3.85683995872529));
#40700=CARTESIAN_POINT('Ctrl Pts',(-0.788065315093778,-1.,3.86436702561345));
#40701=CARTESIAN_POINT('Ctrl Pts',(-0.788065315093778,1.,3.86436702561345));
#40702=CARTESIAN_POINT('Ctrl Pts',(-0.787242527617999,-1.,3.87188916600912));
#40703=CARTESIAN_POINT('Ctrl Pts',(-0.787242527617999,1.,3.87188916600912));
#40704=CARTESIAN_POINT('Ctrl Pts',(-0.786369675812609,-1.,3.8794040281819));
#40705=CARTESIAN_POINT('Ctrl Pts',(-0.786369675812609,1.,3.8794040281819));
#40706=CARTESIAN_POINT('Ctrl Pts',(-0.78544789034073,-1.,3.88691313167398));
#40707=CARTESIAN_POINT('Ctrl Pts',(-0.78544789034073,1.,3.88691313167398));
#40708=CARTESIAN_POINT('Ctrl Pts',(-0.784478799358336,-1.,3.89442039235103));
#40709=CARTESIAN_POINT('Ctrl Pts',(-0.784478799358336,1.,3.89442039235103));
#40710=CARTESIAN_POINT('Ctrl Pts',(-0.783464141529081,-1.,3.9019303904397));
#40711=CARTESIAN_POINT('Ctrl Pts',(-0.783464141529081,1.,3.9019303904397));
#40712=CARTESIAN_POINT('Ctrl Pts',(-0.782405395622764,-1.,3.90944671004542));
#40713=CARTESIAN_POINT('Ctrl Pts',(-0.782405395622764,1.,3.90944671004542));
#40714=CARTESIAN_POINT('Ctrl Pts',(-0.781303428618367,-1.,3.91697036054676));
#40715=CARTESIAN_POINT('Ctrl Pts',(-0.781303428618367,1.,3.91697036054676));
#40716=CARTESIAN_POINT('Ctrl Pts',(-0.780158678615543,-1.,3.92450058323823));
#40717=CARTESIAN_POINT('Ctrl Pts',(-0.780158678615543,1.,3.92450058323823));
#40718=CARTESIAN_POINT('Ctrl Pts',(-0.778971308134821,-1.,3.93203552473174));
#40719=CARTESIAN_POINT('Ctrl Pts',(-0.778971308134821,1.,3.93203552473174));
#40720=CARTESIAN_POINT('Ctrl Pts',(-0.777741370568559,-1.,3.93957296768103));
#40721=CARTESIAN_POINT('Ctrl Pts',(-0.777741370568559,1.,3.93957296768103));
#40722=CARTESIAN_POINT('Ctrl Pts',(-0.776468966697921,-1.,3.94711101619447));
#40723=CARTESIAN_POINT('Ctrl Pts',(-0.776468966697921,1.,3.94711101619447));
#40724=CARTESIAN_POINT('Ctrl Pts',(-0.775154418039352,-1.,3.9546488545231));
#40725=CARTESIAN_POINT('Ctrl Pts',(-0.775154418039352,1.,3.9546488545231));
#40726=CARTESIAN_POINT('Ctrl Pts',(-0.773798212026566,-1.,3.96218649639807));
#40727=CARTESIAN_POINT('Ctrl Pts',(-0.773798212026566,1.,3.96218649639807));
#40728=CARTESIAN_POINT('Ctrl Pts',(-0.772400931772136,-1.,3.96972446532772));
#40729=CARTESIAN_POINT('Ctrl Pts',(-0.772400931772136,1.,3.96972446532772));
#40730=CARTESIAN_POINT('Ctrl Pts',(-0.770963190030471,-1.,3.97726349165488));
#40731=CARTESIAN_POINT('Ctrl Pts',(-0.770963190030471,1.,3.97726349165488));
#40732=CARTESIAN_POINT('Ctrl Pts',(-0.769485566245544,-1.,3.98480422348451));
#40733=CARTESIAN_POINT('Ctrl Pts',(-0.769485566245544,1.,3.98480422348451));
#40734=CARTESIAN_POINT('Ctrl Pts',(-0.767968531377915,-1.,3.9923468788101));
#40735=CARTESIAN_POINT('Ctrl Pts',(-0.767968531377915,1.,3.9923468788101));
#40736=CARTESIAN_POINT('Ctrl Pts',(-0.766412457136064,-1.,3.99989129179622));
#40737=CARTESIAN_POINT('Ctrl Pts',(-0.766412457136064,1.,3.99989129179622));
#40738=CARTESIAN_POINT('Ctrl Pts',(-0.764817648785198,-1.,4.00743706791509));
#40739=CARTESIAN_POINT('Ctrl Pts',(-0.764817648785198,1.,4.00743706791509));
#40740=CARTESIAN_POINT('Ctrl Pts',(-0.763184371182935,-1.,4.01498370680496));
#40741=CARTESIAN_POINT('Ctrl Pts',(-0.763184371182935,1.,4.01498370680496));
#40742=CARTESIAN_POINT('Ctrl Pts',(-0.761512875859804,-1.,4.02253072741268));
#40743=CARTESIAN_POINT('Ctrl Pts',(-0.761512875859804,1.,4.02253072741268));
#40744=CARTESIAN_POINT('Ctrl Pts',(-0.759803433243752,-1.,4.03007781954412));
#40745=CARTESIAN_POINT('Ctrl Pts',(-0.759803433243752,1.,4.03007781954412));
#40746=CARTESIAN_POINT('Ctrl Pts',(-0.758056338884944,-1.,4.03762485803119));
#40747=CARTESIAN_POINT('Ctrl Pts',(-0.758056338884944,1.,4.03762485803119));
#40748=CARTESIAN_POINT('Ctrl Pts',(-0.756271902369581,-1.,4.04517182653997));
#40749=CARTESIAN_POINT('Ctrl Pts',(-0.756271902369581,1.,4.04517182653997));
#40750=CARTESIAN_POINT('Ctrl Pts',(-0.754450441816078,-1.,4.05271876687915));
#40751=CARTESIAN_POINT('Ctrl Pts',(-0.754450441816078,1.,4.05271876687915));
#40752=CARTESIAN_POINT('Ctrl Pts',(-0.752592276483072,-1.,4.06026572221515));
#40753=CARTESIAN_POINT('Ctrl Pts',(-0.752592276483072,1.,4.06026572221515));
#40754=CARTESIAN_POINT('Ctrl Pts',(-0.750697720484036,-1.,4.06781267242378));
#40755=CARTESIAN_POINT('Ctrl Pts',(-0.750697720484036,1.,4.06781267242378));
#40756=CARTESIAN_POINT('Ctrl Pts',(-0.748767076680557,-1.,4.07535951056152));
#40757=CARTESIAN_POINT('Ctrl Pts',(-0.748767076680557,1.,4.07535951056152));
#40758=CARTESIAN_POINT('Ctrl Pts',(-0.746800631492315,-1.,4.08290608095642));
#40759=CARTESIAN_POINT('Ctrl Pts',(-0.746800631492315,1.,4.08290608095642));
#40760=CARTESIAN_POINT('Ctrl Pts',(-0.7447986497065,-1.,4.09045220253573));
#40761=CARTESIAN_POINT('Ctrl Pts',(-0.7447986497065,1.,4.09045220253573));
#40762=CARTESIAN_POINT('Ctrl Pts',(-0.742761369689841,-1.,4.09799769702611));
#40763=CARTESIAN_POINT('Ctrl Pts',(-0.742761369689841,1.,4.09799769702611));
#40764=CARTESIAN_POINT('Ctrl Pts',(-0.740688998553377,-1.,4.10554241757547));
#40765=CARTESIAN_POINT('Ctrl Pts',(-0.740688998553377,1.,4.10554241757547));
#40766=CARTESIAN_POINT('Ctrl Pts',(-0.738581708225844,-1.,4.11308626951927));
#40767=CARTESIAN_POINT('Ctrl Pts',(-0.738581708225844,1.,4.11308626951927));
#40768=CARTESIAN_POINT('Ctrl Pts',(-0.736439634331345,-1.,4.120629196238));
#40769=CARTESIAN_POINT('Ctrl Pts',(-0.736439634331345,1.,4.120629196238));
#40770=CARTESIAN_POINT('Ctrl Pts',(-0.734698226764092,-1.,4.12666277570844));
#40771=CARTESIAN_POINT('Ctrl Pts',(-0.734698226764092,1.,4.12666277570844));
#40772=CARTESIAN_POINT('Ctrl Pts',(-0.733376589323546,-1.,4.13118752795207));
#40773=CARTESIAN_POINT('Ctrl Pts',(-0.733376589323546,1.,4.13118752795207));
#40774=CARTESIAN_POINT('Ctrl Pts',(-0.73248857513516,-1.,4.1342038373684));
#40775=CARTESIAN_POINT('Ctrl Pts',(-0.73248857513516,1.,4.1342038373684));
#40776=CARTESIAN_POINT('Ctrl Pts',(-0.73204283740062,-1.,4.13571194405636));
#40777=CARTESIAN_POINT('Ctrl Pts',(-0.73204283740062,1.,4.13571194405636));
#40778=CARTESIAN_POINT('',(-0.786422660831985,1.,3.66661143271685));
#40779=CARTESIAN_POINT('Ctrl Pts',(-0.786422660831985,-1.,3.66661143271685));
#40780=CARTESIAN_POINT('Ctrl Pts',(-0.786422660831985,-0.666666666666667,
3.66661143271685));
#40781=CARTESIAN_POINT('Ctrl Pts',(-0.786422660831985,-0.333333333333333,
3.66661143271685));
#40782=CARTESIAN_POINT('Ctrl Pts',(-0.786422660831985,0.333333333333333,
3.66661143271685));
#40783=CARTESIAN_POINT('Ctrl Pts',(-0.786422660831985,0.666666666666667,
3.66661143271685));
#40784=CARTESIAN_POINT('Ctrl Pts',(-0.786422660831985,1.,3.66661143271685));
#40785=CARTESIAN_POINT('',(-0.73204283740062,1.,4.13571194405636));
#40786=CARTESIAN_POINT('',(-0.73204283740062,0.,4.13571194405636));
#40787=CARTESIAN_POINT('Ctrl Pts',(-0.786422660831985,1.,3.66661143271685));
#40788=CARTESIAN_POINT('Ctrl Pts',(-0.786459983895432,1.,3.6666431041522));
#40789=CARTESIAN_POINT('Ctrl Pts',(-0.786565919558984,1.,3.66680946938292));
#40790=CARTESIAN_POINT('Ctrl Pts',(-0.786774337198062,1.,3.66743103898702));
#40791=CARTESIAN_POINT('Ctrl Pts',(-0.787145041181546,1.,3.66907505398677));
#40792=CARTESIAN_POINT('Ctrl Pts',(-0.787758799995743,1.,3.67252923663655));
#40793=CARTESIAN_POINT('Ctrl Pts',(-0.788569566220285,1.,3.67777119516252));
#40794=CARTESIAN_POINT('Ctrl Pts',(-0.789483546064387,1.,3.68428439783905));
#40795=CARTESIAN_POINT('Ctrl Pts',(-0.790436284988788,1.,3.69172044327364));
#40796=CARTESIAN_POINT('Ctrl Pts',(-0.79135657569598,1.,3.69968940808721));
#40797=CARTESIAN_POINT('Ctrl Pts',(-0.792177688845818,1.,3.70781724021806));
#40798=CARTESIAN_POINT('Ctrl Pts',(-0.792848377370287,1.,3.71580242396124));
#40799=CARTESIAN_POINT('Ctrl Pts',(-0.793347023784205,1.,3.72348797293734));
#40800=CARTESIAN_POINT('Ctrl Pts',(-0.793682750269684,1.,3.73086914695805));
#40801=CARTESIAN_POINT('Ctrl Pts',(-0.793882700937017,1.,3.73803280541687));
#40802=CARTESIAN_POINT('Ctrl Pts',(-0.793982700459952,1.,3.74511357728861));
#40803=CARTESIAN_POINT('Ctrl Pts',(-0.794017347371377,1.,3.75224692493864));
#40804=CARTESIAN_POINT('Ctrl Pts',(-0.794008429134907,1.,3.75951468666257));
#40805=CARTESIAN_POINT('Ctrl Pts',(-0.793961083688992,1.,3.76692626931111));
#40806=CARTESIAN_POINT('Ctrl Pts',(-0.793870523787408,1.,3.77444863801212));
#40807=CARTESIAN_POINT('Ctrl Pts',(-0.7937262357813,1.,3.78202460377598));
#40808=CARTESIAN_POINT('Ctrl Pts',(-0.793516871680993,1.,3.78959439439235));
#40809=CARTESIAN_POINT('Ctrl Pts',(-0.793235612973273,1.,3.79711921389897));
#40810=CARTESIAN_POINT('Ctrl Pts',(-0.792882695234778,1.,3.80459229925637));
#40811=CARTESIAN_POINT('Ctrl Pts',(-0.792462483517634,1.,3.81202588694756));
#40812=CARTESIAN_POINT('Ctrl Pts',(-0.791981740718635,1.,3.81944345442249));
#40813=CARTESIAN_POINT('Ctrl Pts',(-0.791447528662369,1.,3.82687033899792));
#40814=CARTESIAN_POINT('Ctrl Pts',(-0.790865012705301,1.,3.83432392054786));
#40815=CARTESIAN_POINT('Ctrl Pts',(-0.790236124191242,1.,3.84180762342454));
#40816=CARTESIAN_POINT('Ctrl Pts',(-0.789560798155582,1.,3.84931637808894));
#40817=CARTESIAN_POINT('Ctrl Pts',(-0.788837734090672,1.,3.85683995872529));
#40818=CARTESIAN_POINT('Ctrl Pts',(-0.788065315093778,1.,3.86436702561345));
#40819=CARTESIAN_POINT('Ctrl Pts',(-0.787242527617999,1.,3.87188916600912));
#40820=CARTESIAN_POINT('Ctrl Pts',(-0.786369675812609,1.,3.8794040281819));
#40821=CARTESIAN_POINT('Ctrl Pts',(-0.78544789034073,1.,3.88691313167398));
#40822=CARTESIAN_POINT('Ctrl Pts',(-0.784478799358336,1.,3.89442039235103));
#40823=CARTESIAN_POINT('Ctrl Pts',(-0.783464141529081,1.,3.9019303904397));
#40824=CARTESIAN_POINT('Ctrl Pts',(-0.782405395622764,1.,3.90944671004542));
#40825=CARTESIAN_POINT('Ctrl Pts',(-0.781303428618367,1.,3.91697036054676));
#40826=CARTESIAN_POINT('Ctrl Pts',(-0.780158678615543,1.,3.92450058323823));
#40827=CARTESIAN_POINT('Ctrl Pts',(-0.778971308134821,1.,3.93203552473174));
#40828=CARTESIAN_POINT('Ctrl Pts',(-0.777741370568559,1.,3.93957296768103));
#40829=CARTESIAN_POINT('Ctrl Pts',(-0.776468966697921,1.,3.94711101619447));
#40830=CARTESIAN_POINT('Ctrl Pts',(-0.775154418039352,1.,3.9546488545231));
#40831=CARTESIAN_POINT('Ctrl Pts',(-0.773798212026566,1.,3.96218649639807));
#40832=CARTESIAN_POINT('Ctrl Pts',(-0.772400931772136,1.,3.96972446532772));
#40833=CARTESIAN_POINT('Ctrl Pts',(-0.770963190030471,1.,3.97726349165488));
#40834=CARTESIAN_POINT('Ctrl Pts',(-0.769485566245544,1.,3.98480422348451));
#40835=CARTESIAN_POINT('Ctrl Pts',(-0.767968531377915,1.,3.9923468788101));
#40836=CARTESIAN_POINT('Ctrl Pts',(-0.766412457136064,1.,3.99989129179622));
#40837=CARTESIAN_POINT('Ctrl Pts',(-0.764817648785198,1.,4.00743706791509));
#40838=CARTESIAN_POINT('Ctrl Pts',(-0.763184371182935,1.,4.01498370680496));
#40839=CARTESIAN_POINT('Ctrl Pts',(-0.761512875859804,1.,4.02253072741268));
#40840=CARTESIAN_POINT('Ctrl Pts',(-0.759803433243752,1.,4.03007781954412));
#40841=CARTESIAN_POINT('Ctrl Pts',(-0.758056338884944,1.,4.03762485803119));
#40842=CARTESIAN_POINT('Ctrl Pts',(-0.756271902369581,1.,4.04517182653997));
#40843=CARTESIAN_POINT('Ctrl Pts',(-0.754450441816078,1.,4.05271876687915));
#40844=CARTESIAN_POINT('Ctrl Pts',(-0.752592276483072,1.,4.06026572221515));
#40845=CARTESIAN_POINT('Ctrl Pts',(-0.750697720484036,1.,4.06781267242378));
#40846=CARTESIAN_POINT('Ctrl Pts',(-0.748767076680557,1.,4.07535951056152));
#40847=CARTESIAN_POINT('Ctrl Pts',(-0.746800631492315,1.,4.08290608095642));
#40848=CARTESIAN_POINT('Ctrl Pts',(-0.7447986497065,1.,4.09045220253573));
#40849=CARTESIAN_POINT('Ctrl Pts',(-0.742761369689841,1.,4.09799769702611));
#40850=CARTESIAN_POINT('Ctrl Pts',(-0.740688998553377,1.,4.10554241757547));
#40851=CARTESIAN_POINT('Ctrl Pts',(-0.738581708225844,1.,4.11308626951927));
#40852=CARTESIAN_POINT('Ctrl Pts',(-0.736439634331345,1.,4.120629196238));
#40853=CARTESIAN_POINT('Ctrl Pts',(-0.734698226764092,1.,4.12666277570844));
#40854=CARTESIAN_POINT('Ctrl Pts',(-0.733376589323546,1.,4.13118752795207));
#40855=CARTESIAN_POINT('Ctrl Pts',(-0.73248857513516,1.,4.1342038373684));
#40856=CARTESIAN_POINT('Ctrl Pts',(-0.73204283740062,1.,4.13571194405636));
#40857=CARTESIAN_POINT('Origin',(-0.73204283740062,0.,4.13571194405636));
#40858=CARTESIAN_POINT('',(-0.581791163835815,1.,4.15950947128175));
#40859=CARTESIAN_POINT('Origin',(0.,0.,0.));
#40860=CARTESIAN_POINT('',(-0.963899035117249,1.,3.62400312501245));
#40861=CARTESIAN_POINT('Origin',(0.,1.,0.));
#40862=CARTESIAN_POINT('Ctrl Pts',(-0.963899035117249,1.,3.62400312501245));
#40863=CARTESIAN_POINT('Ctrl Pts',(-0.963899035117249,0.666666666666667,
3.62400312501245));
#40864=CARTESIAN_POINT('Ctrl Pts',(-0.963899035117249,0.333333333333333,
3.62400312501245));
#40865=CARTESIAN_POINT('Ctrl Pts',(-0.963899035117249,-0.333333333333333,
3.62400312501245));
#40866=CARTESIAN_POINT('Ctrl Pts',(-0.963899035117249,-0.666666666666667,
3.62400312501245));
#40867=CARTESIAN_POINT('Ctrl Pts',(-0.963899035117249,-1.,3.62400312501245));
#40868=CARTESIAN_POINT('Ctrl Pts',(-1.22531898815164,-1.,4.01728681790024));
#40869=CARTESIAN_POINT('Ctrl Pts',(-1.22531898815164,1.,4.01728681790024));
#40870=CARTESIAN_POINT('Ctrl Pts',(-1.22423716681447,-1.,4.0161454457032));
#40871=CARTESIAN_POINT('Ctrl Pts',(-1.22423716681447,1.,4.0161454457032));
#40872=CARTESIAN_POINT('Ctrl Pts',(-1.22207656456199,-1.,4.01386104434674));
#40873=CARTESIAN_POINT('Ctrl Pts',(-1.22207656456199,1.,4.01386104434674));
#40874=CARTESIAN_POINT('Ctrl Pts',(-1.21884478244983,-1.,4.01042947142681));
#40875=CARTESIAN_POINT('Ctrl Pts',(-1.21884478244983,1.,4.01042947142681));
#40876=CARTESIAN_POINT('Ctrl Pts',(-1.21455398918813,-1.,4.00584409524937));
#40877=CARTESIAN_POINT('Ctrl Pts',(-1.21455398918813,1.,4.00584409524937));
#40878=CARTESIAN_POINT('Ctrl Pts',(-1.20922097030107,-1.,4.00009577952534));
#40879=CARTESIAN_POINT('Ctrl Pts',(-1.20922097030107,1.,4.00009577952534));
#40880=CARTESIAN_POINT('Ctrl Pts',(-1.2039185237544,-1.,3.99433084800649));
#40881=CARTESIAN_POINT('Ctrl Pts',(-1.2039185237544,1.,3.99433084800649));
#40882=CARTESIAN_POINT('Ctrl Pts',(-1.19864679609596,-1.,3.98854928957287));
#40883=CARTESIAN_POINT('Ctrl Pts',(-1.19864679609596,1.,3.98854928957287));
#40884=CARTESIAN_POINT('Ctrl Pts',(-1.19340598349307,-1.,3.98275111052015));
#40885=CARTESIAN_POINT('Ctrl Pts',(-1.19340598349307,1.,3.98275111052015));
#40886=CARTESIAN_POINT('Ctrl Pts',(-1.18819633715285,-1.,3.97693634766926));
#40887=CARTESIAN_POINT('Ctrl Pts',(-1.18819633715285,1.,3.97693634766926));
#40888=CARTESIAN_POINT('Ctrl Pts',(-1.18301815039596,-1.,3.9711050516465));
#40889=CARTESIAN_POINT('Ctrl Pts',(-1.18301815039596,1.,3.9711050516465));
#40890=CARTESIAN_POINT('Ctrl Pts',(-1.17787174135445,-1.,3.96525726357682));
#40891=CARTESIAN_POINT('Ctrl Pts',(-1.17787174135445,1.,3.96525726357682));
#40892=CARTESIAN_POINT('Ctrl Pts',(-1.17275743590327,-1.,3.95939299213164));
#40893=CARTESIAN_POINT('Ctrl Pts',(-1.17275743590327,1.,3.95939299213164));
#40894=CARTESIAN_POINT('Ctrl Pts',(-1.16767555244495,-1.,3.95351219510062));
#40895=CARTESIAN_POINT('Ctrl Pts',(-1.16767555244495,1.,3.95351219510062));
#40896=CARTESIAN_POINT('Ctrl Pts',(-1.16262637999261,-1.,3.9476147478092));
#40897=CARTESIAN_POINT('Ctrl Pts',(-1.16262637999261,1.,3.9476147478092));
#40898=CARTESIAN_POINT('Ctrl Pts',(-1.1576101834106,-1.,3.94170046685542));
#40899=CARTESIAN_POINT('Ctrl Pts',(-1.1576101834106,1.,3.94170046685542));
#40900=CARTESIAN_POINT('Ctrl Pts',(-1.15262722716391,-1.,3.9357691705651));
#40901=CARTESIAN_POINT('Ctrl Pts',(-1.15262722716391,1.,3.9357691705651));
#40902=CARTESIAN_POINT('Ctrl Pts',(-1.14767779451147,-1.,3.92982073294334));
#40903=CARTESIAN_POINT('Ctrl Pts',(-1.14767779451147,1.,3.92982073294334));
#40904=CARTESIAN_POINT('Ctrl Pts',(-1.14276220561575,-1.,3.92385513133937));
#40905=CARTESIAN_POINT('Ctrl Pts',(-1.14276220561575,1.,3.92385513133937));
#40906=CARTESIAN_POINT('Ctrl Pts',(-1.13788084225511,-1.,3.91787251936688));
#40907=CARTESIAN_POINT('Ctrl Pts',(-1.13788084225511,1.,3.91787251936688));
#40908=CARTESIAN_POINT('Ctrl Pts',(-1.13303414693849,-1.,3.91187321145495));
#40909=CARTESIAN_POINT('Ctrl Pts',(-1.13303414693849,1.,3.91187321145495));
#40910=CARTESIAN_POINT('Ctrl Pts',(-1.12822258281518,-1.,3.90585753318622));
#40911=CARTESIAN_POINT('Ctrl Pts',(-1.12822258281518,1.,3.90585753318622));
#40912=CARTESIAN_POINT('Ctrl Pts',(-1.12344660099029,-1.,3.89982569749978));
#40913=CARTESIAN_POINT('Ctrl Pts',(-1.12344660099029,1.,3.89982569749978));
#40914=CARTESIAN_POINT('Ctrl Pts',(-1.11870660794609,-1.,3.89377768340362));
#40915=CARTESIAN_POINT('Ctrl Pts',(-1.11870660794609,1.,3.89377768340362));
#40916=CARTESIAN_POINT('Ctrl Pts',(-1.11400292434447,-1.,3.88771308285229));
#40917=CARTESIAN_POINT('Ctrl Pts',(-1.11400292434447,1.,3.88771308285229));
#40918=CARTESIAN_POINT('Ctrl Pts',(-1.10933577224029,-1.,3.88163105531791));
#40919=CARTESIAN_POINT('Ctrl Pts',(-1.10933577224029,1.,3.88163105531791));
#40920=CARTESIAN_POINT('Ctrl Pts',(-1.10470536603303,-1.,3.87553067187566));
#40921=CARTESIAN_POINT('Ctrl Pts',(-1.10470536603303,1.,3.87553067187566));
#40922=CARTESIAN_POINT('Ctrl Pts',(-1.10011198761202,-1.,3.86941120134872));
#40923=CARTESIAN_POINT('Ctrl Pts',(-1.10011198761202,1.,3.86941120134872));
#40924=CARTESIAN_POINT('Ctrl Pts',(-1.09555606505012,-1.,3.86327241021242));
#40925=CARTESIAN_POINT('Ctrl Pts',(-1.09555606505012,1.,3.86327241021242));
#40926=CARTESIAN_POINT('Ctrl Pts',(-1.09103825516288,-1.,3.85711487933911));
#40927=CARTESIAN_POINT('Ctrl Pts',(-1.09103825516288,1.,3.85711487933911));
#40928=CARTESIAN_POINT('Ctrl Pts',(-1.08655950846377,-1.,3.8509402522269));
#40929=CARTESIAN_POINT('Ctrl Pts',(-1.08655950846377,1.,3.8509402522269));
#40930=CARTESIAN_POINT('Ctrl Pts',(-1.08212087917986,-1.,3.84475048030615));
#40931=CARTESIAN_POINT('Ctrl Pts',(-1.08212087917986,1.,3.84475048030615));
#40932=CARTESIAN_POINT('Ctrl Pts',(-1.07772335353856,-1.,3.83854714117486));
#40933=CARTESIAN_POINT('Ctrl Pts',(-1.07772335353856,1.,3.83854714117486));
#40934=CARTESIAN_POINT('Ctrl Pts',(-1.0733676663346,-1.,3.83233071195145));
#40935=CARTESIAN_POINT('Ctrl Pts',(-1.0733676663346,1.,3.83233071195145));
#40936=CARTESIAN_POINT('Ctrl Pts',(-1.0690541318036,-1.,3.82609989967278));
#40937=CARTESIAN_POINT('Ctrl Pts',(-1.0690541318036,1.,3.82609989967278));
#40938=CARTESIAN_POINT('Ctrl Pts',(-1.06478244038931,-1.,3.81985083953012));
#40939=CARTESIAN_POINT('Ctrl Pts',(-1.06478244038931,1.,3.81985083953012));
#40940=CARTESIAN_POINT('Ctrl Pts',(-1.06055206187298,-1.,3.81357866117485));
#40941=CARTESIAN_POINT('Ctrl Pts',(-1.06055206187298,1.,3.81357866117485));
#40942=CARTESIAN_POINT('Ctrl Pts',(-1.05636266918643,-1.,3.80727913637784));
#40943=CARTESIAN_POINT('Ctrl Pts',(-1.05636266918643,1.,3.80727913637784));
#40944=CARTESIAN_POINT('Ctrl Pts',(-1.05221457990015,-1.,3.80095039790678));
#40945=CARTESIAN_POINT('Ctrl Pts',(-1.05221457990015,1.,3.80095039790678));
#40946=CARTESIAN_POINT('Ctrl Pts',(-1.04810913267641,-1.,3.79459440308793));
#40947=CARTESIAN_POINT('Ctrl Pts',(-1.04810913267641,1.,3.79459440308793));
#40948=CARTESIAN_POINT('Ctrl Pts',(-1.04404924374426,-1.,3.78821910787195));
#40949=CARTESIAN_POINT('Ctrl Pts',(-1.04404924374426,1.,3.78821910787195));
#40950=CARTESIAN_POINT('Ctrl Pts',(-1.04003862055804,-1.,3.78183535008192));
#40951=CARTESIAN_POINT('Ctrl Pts',(-1.04003862055804,1.,3.78183535008192));
#40952=CARTESIAN_POINT('Ctrl Pts',(-1.03608074678013,-1.,3.77545283140445));
#40953=CARTESIAN_POINT('Ctrl Pts',(-1.03608074678013,1.,3.77545283140445));
#40954=CARTESIAN_POINT('Ctrl Pts',(-1.0321778660492,-1.,3.76907609832522));
#40955=CARTESIAN_POINT('Ctrl Pts',(-1.0321778660492,1.,3.76907609832522));
#40956=CARTESIAN_POINT('Ctrl Pts',(-1.02833014458181,-1.,3.76270122291232));
#40957=CARTESIAN_POINT('Ctrl Pts',(-1.02833014458181,1.,3.76270122291232));
#40958=CARTESIAN_POINT('Ctrl Pts',(-1.0245342944466,-1.,3.75631037456194));
#40959=CARTESIAN_POINT('Ctrl Pts',(-1.0245342944466,1.,3.75631037456194));
#40960=CARTESIAN_POINT('Ctrl Pts',(-1.02078510487428,-1.,3.74987777155834));
#40961=CARTESIAN_POINT('Ctrl Pts',(-1.02078510487428,1.,3.74987777155834));
#40962=CARTESIAN_POINT('Ctrl Pts',(-1.01707794311079,-1.,3.74337942504959));
#40963=CARTESIAN_POINT('Ctrl Pts',(-1.01707794311079,1.,3.74337942504959));
#40964=CARTESIAN_POINT('Ctrl Pts',(-1.01341114319903,-1.,3.73680245055734));
#40965=CARTESIAN_POINT('Ctrl Pts',(-1.01341114319903,1.,3.73680245055734));
#40966=CARTESIAN_POINT('Ctrl Pts',(-1.00978798539496,-1.,3.73015276704426));
#40967=CARTESIAN_POINT('Ctrl Pts',(-1.00978798539496,1.,3.73015276704426));
#40968=CARTESIAN_POINT('Ctrl Pts',(-1.0062200073571,-1.,3.72346803750595));
#40969=CARTESIAN_POINT('Ctrl Pts',(-1.0062200073571,1.,3.72346803750595));
#40970=CARTESIAN_POINT('Ctrl Pts',(-1.00272423396822,-1.,3.71680667125118));
#40971=CARTESIAN_POINT('Ctrl Pts',(-1.00272423396822,1.,3.71680667125118));
#40972=CARTESIAN_POINT('Ctrl Pts',(-0.999317260756531,-1.,3.71022439713938));
#40973=CARTESIAN_POINT('Ctrl Pts',(-0.999317260756531,1.,3.71022439713938));
#40974=CARTESIAN_POINT('Ctrl Pts',(-0.996009819772518,-1.,3.70375282282138));
#40975=CARTESIAN_POINT('Ctrl Pts',(-0.996009819772518,1.,3.70375282282138));
#40976=CARTESIAN_POINT('Ctrl Pts',(-0.99280221833201,-1.,3.69738123415662));
#40977=CARTESIAN_POINT('Ctrl Pts',(-0.99280221833201,1.,3.69738123415662));
#40978=CARTESIAN_POINT('Ctrl Pts',(-0.989676715398558,-1.,3.69102682138846));
#40979=CARTESIAN_POINT('Ctrl Pts',(-0.989676715398558,1.,3.69102682138846));
#40980=CARTESIAN_POINT('Ctrl Pts',(-0.986602639863838,-1.,3.68455317926068));
#40981=CARTESIAN_POINT('Ctrl Pts',(-0.986602639863838,1.,3.68455317926068));
#40982=CARTESIAN_POINT('Ctrl Pts',(-0.983550791470419,-1.,3.67782408841715));
#40983=CARTESIAN_POINT('Ctrl Pts',(-0.983550791470419,1.,3.67782408841715));
#40984=CARTESIAN_POINT('Ctrl Pts',(-0.980505922458267,-1.,3.67074983340361));
#40985=CARTESIAN_POINT('Ctrl Pts',(-0.980505922458267,1.,3.67074983340361));
#40986=CARTESIAN_POINT('Ctrl Pts',(-0.977478312751618,-1.,3.66333049637475));
#40987=CARTESIAN_POINT('Ctrl Pts',(-0.977478312751618,1.,3.66333049637475));
#40988=CARTESIAN_POINT('Ctrl Pts',(-0.974519971354848,-1.,3.65571576735126));
#40989=CARTESIAN_POINT('Ctrl Pts',(-0.974519971354848,1.,3.65571576735126));
#40990=CARTESIAN_POINT('Ctrl Pts',(-0.971722122061341,-1.,3.64819756447455));
#40991=CARTESIAN_POINT('Ctrl Pts',(-0.971722122061341,1.,3.64819756447455));
#40992=CARTESIAN_POINT('Ctrl Pts',(-0.969195124675866,-1.,3.64113946505766));
#40993=CARTESIAN_POINT('Ctrl Pts',(-0.969195124675866,1.,3.64113946505766));
#40994=CARTESIAN_POINT('Ctrl Pts',(-0.967052554541386,-1.,3.63492122081143));
#40995=CARTESIAN_POINT('Ctrl Pts',(-0.967052554541386,1.,3.63492122081143));
#40996=CARTESIAN_POINT('Ctrl Pts',(-0.965395153165293,-1.,3.62988252139846));
#40997=CARTESIAN_POINT('Ctrl Pts',(-0.965395153165293,1.,3.62988252139846));
#40998=CARTESIAN_POINT('Ctrl Pts',(-0.964291001273288,-1.,3.62625391254797));
#40999=CARTESIAN_POINT('Ctrl Pts',(-0.964291001273288,1.,3.62625391254797));
#41000=CARTESIAN_POINT('Ctrl Pts',(-0.963875774530619,-1.,3.6245656860652));
#41001=CARTESIAN_POINT('Ctrl Pts',(-0.963875774530619,1.,3.6245656860652));
#41002=CARTESIAN_POINT('Ctrl Pts',(-0.963832486395051,-1.,3.62399933639914));
#41003=CARTESIAN_POINT('Ctrl Pts',(-0.963832486395051,1.,3.62399933639914));
#41004=CARTESIAN_POINT('Ctrl Pts',(-0.963922720982193,-1.,3.62393257642052));
#41005=CARTESIAN_POINT('Ctrl Pts',(-0.963922720982193,1.,3.62393257642052));
#41006=CARTESIAN_POINT('Ctrl Pts',(-0.963997613369571,-1.,3.62397690409552));
#41007=CARTESIAN_POINT('Ctrl Pts',(-0.963997613369571,1.,3.62397690409552));
#41008=CARTESIAN_POINT('',(-1.22531898815164,1.,4.01728681790024));
#41009=CARTESIAN_POINT('Ctrl Pts',(-1.22531898815164,1.,4.01728681790024));
#41010=CARTESIAN_POINT('Ctrl Pts',(-1.22423716681447,1.,4.0161454457032));
#41011=CARTESIAN_POINT('Ctrl Pts',(-1.22207656456199,1.,4.01386104434674));
#41012=CARTESIAN_POINT('Ctrl Pts',(-1.21884478244983,1.,4.01042947142681));
#41013=CARTESIAN_POINT('Ctrl Pts',(-1.21455398918813,1.,4.00584409524937));
#41014=CARTESIAN_POINT('Ctrl Pts',(-1.20922097030107,1.,4.00009577952534));
#41015=CARTESIAN_POINT('Ctrl Pts',(-1.2039185237544,1.,3.99433084800649));
#41016=CARTESIAN_POINT('Ctrl Pts',(-1.19864679609596,1.,3.98854928957287));
#41017=CARTESIAN_POINT('Ctrl Pts',(-1.19340598349307,1.,3.98275111052015));
#41018=CARTESIAN_POINT('Ctrl Pts',(-1.18819633715285,1.,3.97693634766926));
#41019=CARTESIAN_POINT('Ctrl Pts',(-1.18301815039596,1.,3.9711050516465));
#41020=CARTESIAN_POINT('Ctrl Pts',(-1.17787174135445,1.,3.96525726357682));
#41021=CARTESIAN_POINT('Ctrl Pts',(-1.17275743590327,1.,3.95939299213164));
#41022=CARTESIAN_POINT('Ctrl Pts',(-1.16767555244495,1.,3.95351219510062));
#41023=CARTESIAN_POINT('Ctrl Pts',(-1.16262637999261,1.,3.9476147478092));
#41024=CARTESIAN_POINT('Ctrl Pts',(-1.1576101834106,1.,3.94170046685542));
#41025=CARTESIAN_POINT('Ctrl Pts',(-1.15262722716391,1.,3.9357691705651));
#41026=CARTESIAN_POINT('Ctrl Pts',(-1.14767779451147,1.,3.92982073294334));
#41027=CARTESIAN_POINT('Ctrl Pts',(-1.14276220561575,1.,3.92385513133937));
#41028=CARTESIAN_POINT('Ctrl Pts',(-1.13788084225511,1.,3.91787251936688));
#41029=CARTESIAN_POINT('Ctrl Pts',(-1.13303414693849,1.,3.91187321145495));
#41030=CARTESIAN_POINT('Ctrl Pts',(-1.12822258281518,1.,3.90585753318622));
#41031=CARTESIAN_POINT('Ctrl Pts',(-1.12344660099029,1.,3.89982569749978));
#41032=CARTESIAN_POINT('Ctrl Pts',(-1.11870660794609,1.,3.89377768340362));
#41033=CARTESIAN_POINT('Ctrl Pts',(-1.11400292434447,1.,3.88771308285229));
#41034=CARTESIAN_POINT('Ctrl Pts',(-1.10933577224029,1.,3.88163105531791));
#41035=CARTESIAN_POINT('Ctrl Pts',(-1.10470536603303,1.,3.87553067187566));
#41036=CARTESIAN_POINT('Ctrl Pts',(-1.10011198761202,1.,3.86941120134872));
#41037=CARTESIAN_POINT('Ctrl Pts',(-1.09555606505012,1.,3.86327241021242));
#41038=CARTESIAN_POINT('Ctrl Pts',(-1.09103825516288,1.,3.85711487933911));
#41039=CARTESIAN_POINT('Ctrl Pts',(-1.08655950846377,1.,3.8509402522269));
#41040=CARTESIAN_POINT('Ctrl Pts',(-1.08212087917986,1.,3.84475048030615));
#41041=CARTESIAN_POINT('Ctrl Pts',(-1.07772335353856,1.,3.83854714117486));
#41042=CARTESIAN_POINT('Ctrl Pts',(-1.0733676663346,1.,3.83233071195145));
#41043=CARTESIAN_POINT('Ctrl Pts',(-1.0690541318036,1.,3.82609989967278));
#41044=CARTESIAN_POINT('Ctrl Pts',(-1.06478244038931,1.,3.81985083953012));
#41045=CARTESIAN_POINT('Ctrl Pts',(-1.06055206187298,1.,3.81357866117485));
#41046=CARTESIAN_POINT('Ctrl Pts',(-1.05636266918643,1.,3.80727913637784));
#41047=CARTESIAN_POINT('Ctrl Pts',(-1.05221457990015,1.,3.80095039790678));
#41048=CARTESIAN_POINT('Ctrl Pts',(-1.04810913267641,1.,3.79459440308793));
#41049=CARTESIAN_POINT('Ctrl Pts',(-1.04404924374426,1.,3.78821910787195));
#41050=CARTESIAN_POINT('Ctrl Pts',(-1.04003862055804,1.,3.78183535008192));
#41051=CARTESIAN_POINT('Ctrl Pts',(-1.03608074678013,1.,3.77545283140445));
#41052=CARTESIAN_POINT('Ctrl Pts',(-1.0321778660492,1.,3.76907609832522));
#41053=CARTESIAN_POINT('Ctrl Pts',(-1.02833014458181,1.,3.76270122291232));
#41054=CARTESIAN_POINT('Ctrl Pts',(-1.0245342944466,1.,3.75631037456194));
#41055=CARTESIAN_POINT('Ctrl Pts',(-1.02078510487428,1.,3.74987777155834));
#41056=CARTESIAN_POINT('Ctrl Pts',(-1.01707794311079,1.,3.74337942504959));
#41057=CARTESIAN_POINT('Ctrl Pts',(-1.01341114319903,1.,3.73680245055734));
#41058=CARTESIAN_POINT('Ctrl Pts',(-1.00978798539496,1.,3.73015276704426));
#41059=CARTESIAN_POINT('Ctrl Pts',(-1.0062200073571,1.,3.72346803750595));
#41060=CARTESIAN_POINT('Ctrl Pts',(-1.00272423396822,1.,3.71680667125118));
#41061=CARTESIAN_POINT('Ctrl Pts',(-0.999317260756531,1.,3.71022439713938));
#41062=CARTESIAN_POINT('Ctrl Pts',(-0.996009819772518,1.,3.70375282282138));
#41063=CARTESIAN_POINT('Ctrl Pts',(-0.99280221833201,1.,3.69738123415662));
#41064=CARTESIAN_POINT('Ctrl Pts',(-0.989676715398558,1.,3.69102682138846));
#41065=CARTESIAN_POINT('Ctrl Pts',(-0.986602639863838,1.,3.68455317926068));
#41066=CARTESIAN_POINT('Ctrl Pts',(-0.983550791470419,1.,3.67782408841715));
#41067=CARTESIAN_POINT('Ctrl Pts',(-0.980505922458267,1.,3.67074983340361));
#41068=CARTESIAN_POINT('Ctrl Pts',(-0.977478312751618,1.,3.66333049637475));
#41069=CARTESIAN_POINT('Ctrl Pts',(-0.974519971354848,1.,3.65571576735126));
#41070=CARTESIAN_POINT('Ctrl Pts',(-0.971722122061341,1.,3.64819756447455));
#41071=CARTESIAN_POINT('Ctrl Pts',(-0.969195124675866,1.,3.64113946505766));
#41072=CARTESIAN_POINT('Ctrl Pts',(-0.967052554541386,1.,3.63492122081143));
#41073=CARTESIAN_POINT('Ctrl Pts',(-0.965395153165293,1.,3.62988252139846));
#41074=CARTESIAN_POINT('Ctrl Pts',(-0.964373850166457,1.,3.62652618145335));
#41075=CARTESIAN_POINT('Ctrl Pts',(-0.963957782642843,1.,3.62489305727662));
#41076=CARTESIAN_POINT('Ctrl Pts',(-0.963861297423241,1.,3.62424461507588));
#41077=CARTESIAN_POINT('Ctrl Pts',(-0.963880158555582,1.,3.6240482887845));
#41078=CARTESIAN_POINT('Ctrl Pts',(-0.963899035117249,1.,3.62400312501245));
#41079=CARTESIAN_POINT('',(-1.22531898815164,0.,4.01728681790024));
#41080=CARTESIAN_POINT('Ctrl Pts',(-1.35022972712301,-1.,3.49848248301936));
#41081=CARTESIAN_POINT('Ctrl Pts',(-1.35022972712301,1.,3.49848248301936));
#41082=CARTESIAN_POINT('Ctrl Pts',(-1.35026426118402,-1.,3.4984026005375));
#41083=CARTESIAN_POINT('Ctrl Pts',(-1.35026426118402,1.,3.4984026005375));
#41084=CARTESIAN_POINT('Ctrl Pts',(-1.35037650303019,-1.,3.49840357193736));
#41085=CARTESIAN_POINT('Ctrl Pts',(-1.35037650303019,1.,3.49840357193736));
#41086=CARTESIAN_POINT('Ctrl Pts',(-1.35067437417483,-1.,3.49888720257132));
#41087=CARTESIAN_POINT('Ctrl Pts',(-1.35067437417483,1.,3.49888720257132));
#41088=CARTESIAN_POINT('Ctrl Pts',(-1.3513307633124,-1.,3.5004970706414));
#41089=CARTESIAN_POINT('Ctrl Pts',(-1.3513307633124,1.,3.5004970706414));
#41090=CARTESIAN_POINT('Ctrl Pts',(-1.35257032843486,-1.,3.50408168106261));
#41091=CARTESIAN_POINT('Ctrl Pts',(-1.35257032843486,1.,3.50408168106261));
#41092=CARTESIAN_POINT('Ctrl Pts',(-1.35419113575956,-1.,3.50913227059999));
#41093=CARTESIAN_POINT('Ctrl Pts',(-1.35419113575956,1.,3.50913227059999));
#41094=CARTESIAN_POINT('Ctrl Pts',(-1.35611275237152,-1.,3.51542230699556));
#41095=CARTESIAN_POINT('Ctrl Pts',(-1.35611275237152,1.,3.51542230699556));
#41096=CARTESIAN_POINT('Ctrl Pts',(-1.35821701528836,-1.,3.52261776116748));
#41097=CARTESIAN_POINT('Ctrl Pts',(-1.35821701528836,1.,3.52261776116748));
#41098=CARTESIAN_POINT('Ctrl Pts',(-1.36037259643734,-1.,3.530344649616));
#41099=CARTESIAN_POINT('Ctrl Pts',(-1.36037259643734,1.,3.530344649616));
#41100=CARTESIAN_POINT('Ctrl Pts',(-1.36245507339307,-1.,3.53824396424961));
#41101=CARTESIAN_POINT('Ctrl Pts',(-1.36245507339307,1.,3.53824396424961));
#41102=CARTESIAN_POINT('Ctrl Pts',(-1.36436666257598,-1.,3.54602591832973));
#41103=CARTESIAN_POINT('Ctrl Pts',(-1.36436666257598,1.,3.54602591832973));
#41104=CARTESIAN_POINT('Ctrl Pts',(-1.3660614545677,-1.,3.55353883995949));
#41105=CARTESIAN_POINT('Ctrl Pts',(-1.3660614545677,1.,3.55353883995949));
#41106=CARTESIAN_POINT('Ctrl Pts',(-1.36754771771233,-1.,3.56077662028649));
#41107=CARTESIAN_POINT('Ctrl Pts',(-1.36754771771233,1.,3.56077662028649));
#41108=CARTESIAN_POINT('Ctrl Pts',(-1.36886584973389,-1.,3.5678208030466));
#41109=CARTESIAN_POINT('Ctrl Pts',(-1.36886584973389,1.,3.5678208030466));
#41110=CARTESIAN_POINT('Ctrl Pts',(-1.37007229485659,-1.,3.57479875549486));
#41111=CARTESIAN_POINT('Ctrl Pts',(-1.37007229485659,1.,3.57479875549486));
#41112=CARTESIAN_POINT('Ctrl Pts',(-1.37122241663062,-1.,3.58183885982715));
#41113=CARTESIAN_POINT('Ctrl Pts',(-1.37122241663062,1.,3.58183885982715));
#41114=CARTESIAN_POINT('Ctrl Pts',(-1.37235053660976,-1.,3.58901853846365));
#41115=CARTESIAN_POINT('Ctrl Pts',(-1.37235053660976,1.,3.58901853846365));
#41116=CARTESIAN_POINT('Ctrl Pts',(-1.37346320103157,-1.,3.59634627869048));
#41117=CARTESIAN_POINT('Ctrl Pts',(-1.37346320103157,1.,3.59634627869048));
#41118=CARTESIAN_POINT('Ctrl Pts',(-1.37455051379623,-1.,3.60379020123988));
#41119=CARTESIAN_POINT('Ctrl Pts',(-1.37455051379623,1.,3.60379020123988));
#41120=CARTESIAN_POINT('Ctrl Pts',(-1.37559314436634,-1.,3.61129546591064));
#41121=CARTESIAN_POINT('Ctrl Pts',(-1.37559314436634,1.,3.61129546591064));
#41122=CARTESIAN_POINT('Ctrl Pts',(-1.37657053403107,-1.,3.6188048116042));
#41123=CARTESIAN_POINT('Ctrl Pts',(-1.37657053403107,1.,3.6188048116042));
#41124=CARTESIAN_POINT('Ctrl Pts',(-1.37746987919881,-1.,3.62628098665145));
#41125=CARTESIAN_POINT('Ctrl Pts',(-1.37746987919881,1.,3.62628098665145));
#41126=CARTESIAN_POINT('Ctrl Pts',(-1.37829035457339,-1.,3.63371727442486));
#41127=CARTESIAN_POINT('Ctrl Pts',(-1.37829035457339,1.,3.63371727442486));
#41128=CARTESIAN_POINT('Ctrl Pts',(-1.37903818567359,-1.,3.64112507791141));
#41129=CARTESIAN_POINT('Ctrl Pts',(-1.37903818567359,1.,3.64112507791141));
#41130=CARTESIAN_POINT('Ctrl Pts',(-1.37972372481603,-1.,3.64852652756456));
#41131=CARTESIAN_POINT('Ctrl Pts',(-1.37972372481603,1.,3.64852652756456));
#41132=CARTESIAN_POINT('Ctrl Pts',(-1.38035791051213,-1.,3.6559455440439));
#41133=CARTESIAN_POINT('Ctrl Pts',(-1.38035791051213,1.,3.6559455440439));
#41134=CARTESIAN_POINT('Ctrl Pts',(-1.38094856333552,-1.,3.66339848520857));
#41135=CARTESIAN_POINT('Ctrl Pts',(-1.38094856333552,1.,3.66339848520857));
#41136=CARTESIAN_POINT('Ctrl Pts',(-1.38149812653868,-1.,3.67088843112262));
#41137=CARTESIAN_POINT('Ctrl Pts',(-1.38149812653868,1.,3.67088843112262));
#41138=CARTESIAN_POINT('Ctrl Pts',(-1.3820057429062,-1.,3.67841038482414));
#41139=CARTESIAN_POINT('Ctrl Pts',(-1.3820057429062,1.,3.67841038482414));
#41140=CARTESIAN_POINT('Ctrl Pts',(-1.38246852827182,-1.,3.68595444983837));
#41141=CARTESIAN_POINT('Ctrl Pts',(-1.38246852827182,1.,3.68595444983837));
#41142=CARTESIAN_POINT('Ctrl Pts',(-1.38288311171651,-1.,3.69350967899526));
#41143=CARTESIAN_POINT('Ctrl Pts',(-1.38288311171651,1.,3.69350967899526));
#41144=CARTESIAN_POINT('Ctrl Pts',(-1.38324717612865,-1.,3.701067921679));
#41145=CARTESIAN_POINT('Ctrl Pts',(-1.38324717612865,1.,3.701067921679));
#41146=CARTESIAN_POINT('Ctrl Pts',(-1.38356065402124,-1.,3.70862680753347));
#41147=CARTESIAN_POINT('Ctrl Pts',(-1.38356065402124,1.,3.70862680753347));
#41148=CARTESIAN_POINT('Ctrl Pts',(-1.38382489984586,-1.,3.7161876605181));
#41149=CARTESIAN_POINT('Ctrl Pts',(-1.38382489984586,1.,3.7161876605181));
#41150=CARTESIAN_POINT('Ctrl Pts',(-1.3840421342895,-1.,3.72375409358803));
#41151=CARTESIAN_POINT('Ctrl Pts',(-1.3840421342895,1.,3.72375409358803));
#41152=CARTESIAN_POINT('Ctrl Pts',(-1.38421479111531,-1.,3.73133035859282));
#41153=CARTESIAN_POINT('Ctrl Pts',(-1.38421479111531,1.,3.73133035859282));
#41154=CARTESIAN_POINT('Ctrl Pts',(-1.38434489156458,-1.,3.73891976418104));
#41155=CARTESIAN_POINT('Ctrl Pts',(-1.38434489156458,1.,3.73891976418104));
#41156=CARTESIAN_POINT('Ctrl Pts',(-1.38443344984394,-1.,3.74652317167876));
#41157=CARTESIAN_POINT('Ctrl Pts',(-1.38443344984394,1.,3.74652317167876));
#41158=CARTESIAN_POINT('Ctrl Pts',(-1.38448077997163,-1.,3.7541397631875));
#41159=CARTESIAN_POINT('Ctrl Pts',(-1.38448077997163,1.,3.7541397631875));
#41160=CARTESIAN_POINT('Ctrl Pts',(-1.3844867525335,-1.,3.76176768271367));
#41161=CARTESIAN_POINT('Ctrl Pts',(-1.3844867525335,1.,3.76176768271367));
#41162=CARTESIAN_POINT('Ctrl Pts',(-1.38445107339518,-1.,3.76940473185779));
#41163=CARTESIAN_POINT('Ctrl Pts',(-1.38445107339518,1.,3.76940473185779));
#41164=CARTESIAN_POINT('Ctrl Pts',(-1.38437354551428,-1.,3.77704902230418));
#41165=CARTESIAN_POINT('Ctrl Pts',(-1.38437354551428,1.,3.77704902230418));
#41166=CARTESIAN_POINT('Ctrl Pts',(-1.38425435883756,-1.,3.78469969805082));
#41167=CARTESIAN_POINT('Ctrl Pts',(-1.38425435883756,1.,3.78469969805082));
#41168=CARTESIAN_POINT('Ctrl Pts',(-1.38409399694566,-1.,3.79235669640841));
#41169=CARTESIAN_POINT('Ctrl Pts',(-1.38409399694566,1.,3.79235669640841));
#41170=CARTESIAN_POINT('Ctrl Pts',(-1.38389311766682,-1.,3.80002044322111));
#41171=CARTESIAN_POINT('Ctrl Pts',(-1.38389311766682,1.,3.80002044322111));
#41172=CARTESIAN_POINT('Ctrl Pts',(-1.3836524404622,-1.,3.80769156398411));
#41173=CARTESIAN_POINT('Ctrl Pts',(-1.3836524404622,1.,3.80769156398411));
#41174=CARTESIAN_POINT('Ctrl Pts',(-1.38337263902782,-1.,3.81537060817811));
#41175=CARTESIAN_POINT('Ctrl Pts',(-1.38337263902782,1.,3.81537060817811));
#41176=CARTESIAN_POINT('Ctrl Pts',(-1.38305421262763,-1.,3.82305771743829));
#41177=CARTESIAN_POINT('Ctrl Pts',(-1.38305421262763,1.,3.82305771743829));
#41178=CARTESIAN_POINT('Ctrl Pts',(-1.38269750245138,-1.,3.8307526698229));
#41179=CARTESIAN_POINT('Ctrl Pts',(-1.38269750245138,1.,3.8307526698229));
#41180=CARTESIAN_POINT('Ctrl Pts',(-1.38230274828822,-1.,3.83845502790746));
#41181=CARTESIAN_POINT('Ctrl Pts',(-1.38230274828822,1.,3.83845502790746));
#41182=CARTESIAN_POINT('Ctrl Pts',(-1.38187013346109,-1.,3.84616425605764));
#41183=CARTESIAN_POINT('Ctrl Pts',(-1.38187013346109,1.,3.84616425605764));
#41184=CARTESIAN_POINT('Ctrl Pts',(-1.38139983115049,-1.,3.85387983979481));
#41185=CARTESIAN_POINT('Ctrl Pts',(-1.38139983115049,1.,3.85387983979481));
#41186=CARTESIAN_POINT('Ctrl Pts',(-1.38089205992989,-1.,3.86160143043959));
#41187=CARTESIAN_POINT('Ctrl Pts',(-1.38089205992989,1.,3.86160143043959));
#41188=CARTESIAN_POINT('Ctrl Pts',(-1.38034709213014,-1.,3.86932885813068));
#41189=CARTESIAN_POINT('Ctrl Pts',(-1.38034709213014,1.,3.86932885813068));
#41190=CARTESIAN_POINT('Ctrl Pts',(-1.37976523097073,-1.,3.87706205830532));
#41191=CARTESIAN_POINT('Ctrl Pts',(-1.37976523097073,1.,3.87706205830532));
#41192=CARTESIAN_POINT('Ctrl Pts',(-1.37914679719383,-1.,3.88480102249277));
#41193=CARTESIAN_POINT('Ctrl Pts',(-1.37914679719383,1.,3.88480102249277));
#41194=CARTESIAN_POINT('Ctrl Pts',(-1.3784921128802,-1.,3.89254574338496));
#41195=CARTESIAN_POINT('Ctrl Pts',(-1.3784921128802,1.,3.89254574338496));
#41196=CARTESIAN_POINT('Ctrl Pts',(-1.37780148512792,-1.,3.90029615196727));
#41197=CARTESIAN_POINT('Ctrl Pts',(-1.37780148512792,1.,3.90029615196727));
#41198=CARTESIAN_POINT('Ctrl Pts',(-1.3770751963402,-1.,3.90805209523486));
#41199=CARTESIAN_POINT('Ctrl Pts',(-1.3770751963402,1.,3.90805209523486));
#41200=CARTESIAN_POINT('Ctrl Pts',(-1.37631350505797,-1.,3.91581337462644));
#41201=CARTESIAN_POINT('Ctrl Pts',(-1.37631350505797,1.,3.91581337462644));
#41202=CARTESIAN_POINT('Ctrl Pts',(-1.37551664448242,-1.,3.92357976987672));
#41203=CARTESIAN_POINT('Ctrl Pts',(-1.37551664448242,1.,3.92357976987672));
#41204=CARTESIAN_POINT('Ctrl Pts',(-1.37468482215751,-1.,3.93135106761844));
#41205=CARTESIAN_POINT('Ctrl Pts',(-1.37468482215751,1.,3.93135106761844));
#41206=CARTESIAN_POINT('Ctrl Pts',(-1.37381821967165,-1.,3.93912709040818));
#41207=CARTESIAN_POINT('Ctrl Pts',(-1.37381821967165,1.,3.93912709040818));
#41208=CARTESIAN_POINT('Ctrl Pts',(-1.37291699202807,-1.,3.94690771785133));
#41209=CARTESIAN_POINT('Ctrl Pts',(-1.37291699202807,1.,3.94690771785133));
#41210=CARTESIAN_POINT('Ctrl Pts',(-1.37198126432386,-1.,3.95469287280914));
#41211=CARTESIAN_POINT('Ctrl Pts',(-1.37198126432386,1.,3.95469287280914));
#41212=CARTESIAN_POINT('Ctrl Pts',(-1.3712051561502,-1.,3.96092458506535));
#41213=CARTESIAN_POINT('Ctrl Pts',(-1.3712051561502,1.,3.96092458506535));
#41214=CARTESIAN_POINT('Ctrl Pts',(-1.37060761745635,-1.,3.96560037974645));
#41215=CARTESIAN_POINT('Ctrl Pts',(-1.37060761745635,1.,3.96560037974645));
#41216=CARTESIAN_POINT('Ctrl Pts',(-1.37020239094614,-1.,3.9687184694131));
#41217=CARTESIAN_POINT('Ctrl Pts',(-1.37020239094614,1.,3.9687184694131));
#41218=CARTESIAN_POINT('Ctrl Pts',(-1.36999806084572,-1.,3.97027773754922));
#41219=CARTESIAN_POINT('Ctrl Pts',(-1.36999806084572,1.,3.97027773754922));
#41220=CARTESIAN_POINT('',(-1.35032489087101,1.,3.4984457533445));
#41221=CARTESIAN_POINT('Ctrl Pts',(-1.35032489087101,-1.,3.4984457533445));
#41222=CARTESIAN_POINT('Ctrl Pts',(-1.35032489087101,-0.666666666666667,
3.4984457533445));
#41223=CARTESIAN_POINT('Ctrl Pts',(-1.35032489087101,-0.333333333333333,
3.4984457533445));
#41224=CARTESIAN_POINT('Ctrl Pts',(-1.35032489087101,0.333333333333333,
3.4984457533445));
#41225=CARTESIAN_POINT('Ctrl Pts',(-1.35032489087101,0.666666666666667,
3.4984457533445));
#41226=CARTESIAN_POINT('Ctrl Pts',(-1.35032489087101,1.,3.4984457533445));
#41227=CARTESIAN_POINT('',(-1.36999806084572,1.,3.97027773754922));
#41228=CARTESIAN_POINT('',(-1.36999806084572,0.,3.97027773754922));
#41229=CARTESIAN_POINT('Ctrl Pts',(-1.35032489087101,1.,3.4984457533445));
#41230=CARTESIAN_POINT('Ctrl Pts',(-1.35036670892966,1.,3.49847119623846));
#41231=CARTESIAN_POINT('Ctrl Pts',(-1.35049736560527,1.,3.49861894124827));
#41232=CARTESIAN_POINT('Ctrl Pts',(-1.35080045218587,1.,3.49920025459723));
#41233=CARTESIAN_POINT('Ctrl Pts',(-1.35142377279517,1.,3.5007660381649));
#41234=CARTESIAN_POINT('Ctrl Pts',(-1.35257032843486,1.,3.50408168106261));
#41235=CARTESIAN_POINT('Ctrl Pts',(-1.35419113575956,1.,3.50913227059999));
#41236=CARTESIAN_POINT('Ctrl Pts',(-1.35611275237152,1.,3.51542230699556));
#41237=CARTESIAN_POINT('Ctrl Pts',(-1.35821701528836,1.,3.52261776116748));
#41238=CARTESIAN_POINT('Ctrl Pts',(-1.36037259643734,1.,3.530344649616));
#41239=CARTESIAN_POINT('Ctrl Pts',(-1.36245507339307,1.,3.53824396424961));
#41240=CARTESIAN_POINT('Ctrl Pts',(-1.36436666257598,1.,3.54602591832973));
#41241=CARTESIAN_POINT('Ctrl Pts',(-1.3660614545677,1.,3.55353883995949));
#41242=CARTESIAN_POINT('Ctrl Pts',(-1.36754771771233,1.,3.56077662028649));
#41243=CARTESIAN_POINT('Ctrl Pts',(-1.36886584973389,1.,3.5678208030466));
#41244=CARTESIAN_POINT('Ctrl Pts',(-1.37007229485659,1.,3.57479875549486));
#41245=CARTESIAN_POINT('Ctrl Pts',(-1.37122241663062,1.,3.58183885982715));
#41246=CARTESIAN_POINT('Ctrl Pts',(-1.37235053660976,1.,3.58901853846365));
#41247=CARTESIAN_POINT('Ctrl Pts',(-1.37346320103157,1.,3.59634627869048));
#41248=CARTESIAN_POINT('Ctrl Pts',(-1.37455051379623,1.,3.60379020123988));
#41249=CARTESIAN_POINT('Ctrl Pts',(-1.37559314436634,1.,3.61129546591064));
#41250=CARTESIAN_POINT('Ctrl Pts',(-1.37657053403107,1.,3.6188048116042));
#41251=CARTESIAN_POINT('Ctrl Pts',(-1.37746987919881,1.,3.62628098665145));
#41252=CARTESIAN_POINT('Ctrl Pts',(-1.37829035457339,1.,3.63371727442486));
#41253=CARTESIAN_POINT('Ctrl Pts',(-1.37903818567359,1.,3.64112507791141));
#41254=CARTESIAN_POINT('Ctrl Pts',(-1.37972372481603,1.,3.64852652756456));
#41255=CARTESIAN_POINT('Ctrl Pts',(-1.38035791051213,1.,3.6559455440439));
#41256=CARTESIAN_POINT('Ctrl Pts',(-1.38094856333552,1.,3.66339848520857));
#41257=CARTESIAN_POINT('Ctrl Pts',(-1.38149812653868,1.,3.67088843112262));
#41258=CARTESIAN_POINT('Ctrl Pts',(-1.3820057429062,1.,3.67841038482414));
#41259=CARTESIAN_POINT('Ctrl Pts',(-1.38246852827182,1.,3.68595444983837));
#41260=CARTESIAN_POINT('Ctrl Pts',(-1.38288311171651,1.,3.69350967899526));
#41261=CARTESIAN_POINT('Ctrl Pts',(-1.38324717612865,1.,3.701067921679));
#41262=CARTESIAN_POINT('Ctrl Pts',(-1.38356065402124,1.,3.70862680753347));
#41263=CARTESIAN_POINT('Ctrl Pts',(-1.38382489984586,1.,3.7161876605181));
#41264=CARTESIAN_POINT('Ctrl Pts',(-1.3840421342895,1.,3.72375409358803));
#41265=CARTESIAN_POINT('Ctrl Pts',(-1.38421479111531,1.,3.73133035859282));
#41266=CARTESIAN_POINT('Ctrl Pts',(-1.38434489156458,1.,3.73891976418104));
#41267=CARTESIAN_POINT('Ctrl Pts',(-1.38443344984394,1.,3.74652317167876));
#41268=CARTESIAN_POINT('Ctrl Pts',(-1.38448077997163,1.,3.7541397631875));
#41269=CARTESIAN_POINT('Ctrl Pts',(-1.3844867525335,1.,3.76176768271367));
#41270=CARTESIAN_POINT('Ctrl Pts',(-1.38445107339518,1.,3.76940473185779));
#41271=CARTESIAN_POINT('Ctrl Pts',(-1.38437354551428,1.,3.77704902230418));
#41272=CARTESIAN_POINT('Ctrl Pts',(-1.38425435883756,1.,3.78469969805082));
#41273=CARTESIAN_POINT('Ctrl Pts',(-1.38409399694566,1.,3.79235669640841));
#41274=CARTESIAN_POINT('Ctrl Pts',(-1.38389311766682,1.,3.80002044322111));
#41275=CARTESIAN_POINT('Ctrl Pts',(-1.3836524404622,1.,3.80769156398411));
#41276=CARTESIAN_POINT('Ctrl Pts',(-1.38337263902782,1.,3.81537060817811));
#41277=CARTESIAN_POINT('Ctrl Pts',(-1.38305421262763,1.,3.82305771743829));
#41278=CARTESIAN_POINT('Ctrl Pts',(-1.38269750245138,1.,3.8307526698229));
#41279=CARTESIAN_POINT('Ctrl Pts',(-1.38230274828822,1.,3.83845502790746));
#41280=CARTESIAN_POINT('Ctrl Pts',(-1.38187013346109,1.,3.84616425605764));
#41281=CARTESIAN_POINT('Ctrl Pts',(-1.38139983115049,1.,3.85387983979481));
#41282=CARTESIAN_POINT('Ctrl Pts',(-1.38089205992989,1.,3.86160143043959));
#41283=CARTESIAN_POINT('Ctrl Pts',(-1.38034709213014,1.,3.86932885813068));
#41284=CARTESIAN_POINT('Ctrl Pts',(-1.37976523097073,1.,3.87706205830532));
#41285=CARTESIAN_POINT('Ctrl Pts',(-1.37914679719383,1.,3.88480102249277));
#41286=CARTESIAN_POINT('Ctrl Pts',(-1.3784921128802,1.,3.89254574338496));
#41287=CARTESIAN_POINT('Ctrl Pts',(-1.37780148512792,1.,3.90029615196727));
#41288=CARTESIAN_POINT('Ctrl Pts',(-1.3770751963402,1.,3.90805209523486));
#41289=CARTESIAN_POINT('Ctrl Pts',(-1.37631350505797,1.,3.91581337462644));
#41290=CARTESIAN_POINT('Ctrl Pts',(-1.37551664448242,1.,3.92357976987672));
#41291=CARTESIAN_POINT('Ctrl Pts',(-1.37468482215751,1.,3.93135106761844));
#41292=CARTESIAN_POINT('Ctrl Pts',(-1.37381821967165,1.,3.93912709040818));
#41293=CARTESIAN_POINT('Ctrl Pts',(-1.37291699202807,1.,3.94690771785133));
#41294=CARTESIAN_POINT('Ctrl Pts',(-1.37198126432386,1.,3.95469287280914));
#41295=CARTESIAN_POINT('Ctrl Pts',(-1.3712051561502,1.,3.96092458506535));
#41296=CARTESIAN_POINT('Ctrl Pts',(-1.37060761745635,1.,3.96560037974645));
#41297=CARTESIAN_POINT('Ctrl Pts',(-1.37020239094614,1.,3.9687184694131));
#41298=CARTESIAN_POINT('Ctrl Pts',(-1.36999806084572,1.,3.97027773754922));
#41299=CARTESIAN_POINT('Origin',(-1.36999806084572,0.,3.97027773754922));
#41300=CARTESIAN_POINT('',(-1.22531898815164,1.,4.01728681790024));
#41301=CARTESIAN_POINT('Origin',(0.,0.,0.));
#41302=CARTESIAN_POINT('',(-1.51895082866166,1.,3.42859860294378));
#41303=CARTESIAN_POINT('Origin',(0.,1.,0.));
#41304=CARTESIAN_POINT('Ctrl Pts',(-1.51895082866166,1.,3.42859860294378));
#41305=CARTESIAN_POINT('Ctrl Pts',(-1.51895082866166,0.666666666666667,
3.42859860294378));
#41306=CARTESIAN_POINT('Ctrl Pts',(-1.51895082866166,0.333333333333333,
3.42859860294378));
#41307=CARTESIAN_POINT('Ctrl Pts',(-1.51895082866166,-0.333333333333333,
3.42859860294378));
#41308=CARTESIAN_POINT('Ctrl Pts',(-1.51895082866166,-0.666666666666667,
3.42859860294378));
#41309=CARTESIAN_POINT('Ctrl Pts',(-1.51895082866166,-1.,3.42859860294378));
#41310=CARTESIAN_POINT('Ctrl Pts',(-1.83867539237861,-1.,3.77614523045147));
#41311=CARTESIAN_POINT('Ctrl Pts',(-1.83867539237861,1.,3.77614523045147));
#41312=CARTESIAN_POINT('Ctrl Pts',(-1.83742834010821,-1.,3.77518714458232));
#41313=CARTESIAN_POINT('Ctrl Pts',(-1.83742834010821,1.,3.77518714458232));
#41314=CARTESIAN_POINT('Ctrl Pts',(-1.83493697935064,-1.,3.77326886065484));
#41315=CARTESIAN_POINT('Ctrl Pts',(-1.83493697935064,1.,3.77326886065484));
#41316=CARTESIAN_POINT('Ctrl Pts',(-1.83120816956515,-1.,3.77038509819777));
#41317=CARTESIAN_POINT('Ctrl Pts',(-1.83120816956515,1.,3.77038509819777));
#41318=CARTESIAN_POINT('Ctrl Pts',(-1.82625289221933,-1.,3.76652740355856));
#41319=CARTESIAN_POINT('Ctrl Pts',(-1.82625289221933,1.,3.76652740355856));
#41320=CARTESIAN_POINT('Ctrl Pts',(-1.82008629694924,-1.,3.76168412709652));
#41321=CARTESIAN_POINT('Ctrl Pts',(-1.82008629694924,1.,3.76168412709652));
#41322=CARTESIAN_POINT('Ctrl Pts',(-1.81394729834032,-1.,3.75681965683995));
#41323=CARTESIAN_POINT('Ctrl Pts',(-1.81394729834032,1.,3.75681965683995));
#41324=CARTESIAN_POINT('Ctrl Pts',(-1.80783603939662,-1.,3.75193395888069));
#41325=CARTESIAN_POINT('Ctrl Pts',(-1.80783603939662,1.,3.75193395888069));
#41326=CARTESIAN_POINT('Ctrl Pts',(-1.80175271485519,-1.,3.74702700874954));
#41327=CARTESIAN_POINT('Ctrl Pts',(-1.80175271485519,1.,3.74702700874954));
#41328=CARTESIAN_POINT('Ctrl Pts',(-1.79569757859041,-1.,3.74209880351667));
#41329=CARTESIAN_POINT('Ctrl Pts',(-1.79569757859041,1.,3.74209880351667));
#41330=CARTESIAN_POINT('Ctrl Pts',(-1.78967092823139,-1.,3.73714934729962));
#41331=CARTESIAN_POINT('Ctrl Pts',(-1.78967092823139,1.,3.73714934729962));
#41332=CARTESIAN_POINT('Ctrl Pts',(-1.78367308442682,-1.,3.73217863095022));
#41333=CARTESIAN_POINT('Ctrl Pts',(-1.78367308442682,1.,3.73217863095022));
#41334=CARTESIAN_POINT('Ctrl Pts',(-1.77770437039606,-1.,3.72718661205504));
#41335=CARTESIAN_POINT('Ctrl Pts',(-1.77770437039606,1.,3.72718661205504));
#41336=CARTESIAN_POINT('Ctrl Pts',(-1.77176509401846,-1.,3.72217319911429));
#41337=CARTESIAN_POINT('Ctrl Pts',(-1.77176509401846,1.,3.72217319911429));
#41338=CARTESIAN_POINT('Ctrl Pts',(-1.76585552124549,-1.,3.71713822377675));
#41339=CARTESIAN_POINT('Ctrl Pts',(-1.76585552124549,1.,3.71713822377675));
#41340=CARTESIAN_POINT('Ctrl Pts',(-1.75997588499021,-1.,3.71208146346454));
#41341=CARTESIAN_POINT('Ctrl Pts',(-1.75997588499021,1.,3.71208146346454));
#41342=CARTESIAN_POINT('Ctrl Pts',(-1.75412641804148,-1.,3.70700269736876));
#41343=CARTESIAN_POINT('Ctrl Pts',(-1.75412641804148,1.,3.70700269736876));
#41344=CARTESIAN_POINT('Ctrl Pts',(-1.74830738046092,-1.,3.70190175673422));
#41345=CARTESIAN_POINT('Ctrl Pts',(-1.74830738046092,1.,3.70190175673422));
#41346=CARTESIAN_POINT('Ctrl Pts',(-1.74251908492589,-1.,3.6967785691046));
#41347=CARTESIAN_POINT('Ctrl Pts',(-1.74251908492589,1.,3.6967785691046));
#41348=CARTESIAN_POINT('Ctrl Pts',(-1.73676193254493,-1.,3.69163322647906));
#41349=CARTESIAN_POINT('Ctrl Pts',(-1.73676193254493,1.,3.69163322647906));
#41350=CARTESIAN_POINT('Ctrl Pts',(-1.73103640956647,-1.,3.68646597019188));
#41351=CARTESIAN_POINT('Ctrl Pts',(-1.73103640956647,1.,3.68646597019188));
#41352=CARTESIAN_POINT('Ctrl Pts',(-1.72534302437003,-1.,3.68127704936472));
#41353=CARTESIAN_POINT('Ctrl Pts',(-1.72534302437003,1.,3.68127704936472));
#41354=CARTESIAN_POINT('Ctrl Pts',(-1.71968225581787,-1.,3.67606660374665));
#41355=CARTESIAN_POINT('Ctrl Pts',(-1.71968225581787,1.,3.67606660374665));
#41356=CARTESIAN_POINT('Ctrl Pts',(-1.71405450210392,-1.,3.67083454901629));
#41357=CARTESIAN_POINT('Ctrl Pts',(-1.71405450210392,1.,3.67083454901629));
#41358=CARTESIAN_POINT('Ctrl Pts',(-1.70846001610983,-1.,3.6655804319893));
#41359=CARTESIAN_POINT('Ctrl Pts',(-1.70846001610983,1.,3.6655804319893));
#41360=CARTESIAN_POINT('Ctrl Pts',(-1.70289888566904,-1.,3.6603033877491));
#41361=CARTESIAN_POINT('Ctrl Pts',(-1.70289888566904,1.,3.6603033877491));
#41362=CARTESIAN_POINT('Ctrl Pts',(-1.69737117722559,-1.,3.65500246526798));
#41363=CARTESIAN_POINT('Ctrl Pts',(-1.69737117722559,1.,3.65500246526798));
#41364=CARTESIAN_POINT('Ctrl Pts',(-1.691877054817,-1.,3.64967689827393));
#41365=CARTESIAN_POINT('Ctrl Pts',(-1.691877054817,1.,3.64967689827393));
#41366=CARTESIAN_POINT('Ctrl Pts',(-1.68641690471455,-1.,3.64432638915199));
#41367=CARTESIAN_POINT('Ctrl Pts',(-1.68641690471455,1.,3.64432638915199));
#41368=CARTESIAN_POINT('Ctrl Pts',(-1.68099146651577,-1.,3.63895140887443));
#41369=CARTESIAN_POINT('Ctrl Pts',(-1.68099146651577,1.,3.63895140887443));
#41370=CARTESIAN_POINT('Ctrl Pts',(-1.67560193613145,-1.,3.63355343201211));
#41371=CARTESIAN_POINT('Ctrl Pts',(-1.67560193613145,1.,3.63355343201211));
#41372=CARTESIAN_POINT('Ctrl Pts',(-1.67024966008037,-1.,3.62813422105257));
#41373=CARTESIAN_POINT('Ctrl Pts',(-1.67024966008037,1.,3.62813422105257));
#41374=CARTESIAN_POINT('Ctrl Pts',(-1.66493585923853,-1.,3.62269517989104));
#41375=CARTESIAN_POINT('Ctrl Pts',(-1.66493585923853,1.,3.62269517989104));
#41376=CARTESIAN_POINT('Ctrl Pts',(-1.65966133399186,-1.,3.61723666482457));
#41377=CARTESIAN_POINT('Ctrl Pts',(-1.65966133399186,1.,3.61723666482457));
#41378=CARTESIAN_POINT('Ctrl Pts',(-1.65442619244327,-1.,3.61175734965129));
#41379=CARTESIAN_POINT('Ctrl Pts',(-1.65442619244327,1.,3.61175734965129));
#41380=CARTESIAN_POINT('Ctrl Pts',(-1.64922952425833,-1.,3.60625346556992));
#41381=CARTESIAN_POINT('Ctrl Pts',(-1.64922952425833,1.,3.60625346556992));
#41382=CARTESIAN_POINT('Ctrl Pts',(-1.6440700438558,-1.,3.6007202851384));
#41383=CARTESIAN_POINT('Ctrl Pts',(-1.6440700438558,1.,3.6007202851384));
#41384=CARTESIAN_POINT('Ctrl Pts',(-1.63894676675349,-1.,3.59515368334887));
#41385=CARTESIAN_POINT('Ctrl Pts',(-1.63894676675349,1.,3.59515368334887));
#41386=CARTESIAN_POINT('Ctrl Pts',(-1.63385971451259,-1.,3.58955176627876));
#41387=CARTESIAN_POINT('Ctrl Pts',(-1.63385971451259,1.,3.58955176627876));
#41388=CARTESIAN_POINT('Ctrl Pts',(-1.62881051550748,-1.,3.5839162577435));
#41389=CARTESIAN_POINT('Ctrl Pts',(-1.62881051550748,1.,3.5839162577435));
#41390=CARTESIAN_POINT('Ctrl Pts',(-1.62380329464851,-1.,3.57825455954405));
#41391=CARTESIAN_POINT('Ctrl Pts',(-1.62380329464851,1.,3.57825455954405));
#41392=CARTESIAN_POINT('Ctrl Pts',(-1.61884340915412,-1.,3.57257679609826));
#41393=CARTESIAN_POINT('Ctrl Pts',(-1.61884340915412,1.,3.57257679609826));
#41394=CARTESIAN_POINT('Ctrl Pts',(-1.61393581747522,-1.,3.56689200468404));
#41395=CARTESIAN_POINT('Ctrl Pts',(-1.61393581747522,1.,3.56689200468404));
#41396=CARTESIAN_POINT('Ctrl Pts',(-1.60908344685459,-1.,3.56120432482986));
#41397=CARTESIAN_POINT('Ctrl Pts',(-1.60908344685459,1.,3.56120432482986));
#41398=CARTESIAN_POINT('Ctrl Pts',(-1.60428584699848,-1.,3.55550985096117));
#41399=CARTESIAN_POINT('Ctrl Pts',(-1.60428584699848,1.,3.55550985096117));
#41400=CARTESIAN_POINT('Ctrl Pts',(-1.59953698113444,-1.,3.54979148634426));
#41401=CARTESIAN_POINT('Ctrl Pts',(-1.59953698113444,1.,3.54979148634426));
#41402=CARTESIAN_POINT('Ctrl Pts',(-1.5948276694975,-1.,3.544024581823));
#41403=CARTESIAN_POINT('Ctrl Pts',(-1.5948276694975,1.,3.544024581823));
#41404=CARTESIAN_POINT('Ctrl Pts',(-1.59014958368725,-1.,3.53818616861045));
#41405=CARTESIAN_POINT('Ctrl Pts',(-1.59014958368725,1.,3.53818616861045));
#41406=CARTESIAN_POINT('Ctrl Pts',(-1.58549906268083,-1.,3.53226378147068));
#41407=CARTESIAN_POINT('Ctrl Pts',(-1.58549906268083,1.,3.53226378147068));
#41408=CARTESIAN_POINT('Ctrl Pts',(-1.58088027227856,-1.,3.52626275334899));
#41409=CARTESIAN_POINT('Ctrl Pts',(-1.58088027227856,1.,3.52626275334899));
#41410=CARTESIAN_POINT('Ctrl Pts',(-1.5763104998818,-1.,3.52021847865961));
#41411=CARTESIAN_POINT('Ctrl Pts',(-1.5763104998818,1.,3.52021847865961));
#41412=CARTESIAN_POINT('Ctrl Pts',(-1.57181569799774,-1.,3.51418598431733));
#41413=CARTESIAN_POINT('Ctrl Pts',(-1.57181569799774,1.,3.51418598431733));
#41414=CARTESIAN_POINT('Ctrl Pts',(-1.56742097575041,-1.,3.50821771695427));
#41415=CARTESIAN_POINT('Ctrl Pts',(-1.56742097575041,1.,3.50821771695427));
#41416=CARTESIAN_POINT('Ctrl Pts',(-1.56314187758689,-1.,3.50234321621607));
#41417=CARTESIAN_POINT('Ctrl Pts',(-1.56314187758689,1.,3.50234321621607));
#41418=CARTESIAN_POINT('Ctrl Pts',(-1.55897703097859,-1.,3.49655185179623));
#41419=CARTESIAN_POINT('Ctrl Pts',(-1.55897703097859,1.,3.49655185179623));
#41420=CARTESIAN_POINT('Ctrl Pts',(-1.5548959590107,-1.,3.49076460877317));
#41421=CARTESIAN_POINT('Ctrl Pts',(-1.5548959590107,1.,3.49076460877317));
#41422=CARTESIAN_POINT('Ctrl Pts',(-1.55084702970382,-1.,3.48485155928414));
#41423=CARTESIAN_POINT('Ctrl Pts',(-1.55084702970382,1.,3.48485155928414));
#41424=CARTESIAN_POINT('Ctrl Pts',(-1.54678009290207,-1.,3.47868272898599));
#41425=CARTESIAN_POINT('Ctrl Pts',(-1.54678009290207,1.,3.47868272898599));
#41426=CARTESIAN_POINT('Ctrl Pts',(-1.54266605398152,-1.,3.47217189224576));
#41427=CARTESIAN_POINT('Ctrl Pts',(-1.54266605398152,1.,3.47217189224576));
#41428=CARTESIAN_POINT('Ctrl Pts',(-1.53851507915533,-1.,3.46531752207222));
#41429=CARTESIAN_POINT('Ctrl Pts',(-1.53851507915533,1.,3.46531752207222));
#41430=CARTESIAN_POINT('Ctrl Pts',(-1.53440195378902,-1.,3.45825932955273));
#41431=CARTESIAN_POINT('Ctrl Pts',(-1.53440195378902,1.,3.45825932955273));
#41432=CARTESIAN_POINT('Ctrl Pts',(-1.530462444618,-1.,3.45127136828667));
#41433=CARTESIAN_POINT('Ctrl Pts',(-1.530462444618,1.,3.45127136828667));
#41434=CARTESIAN_POINT('Ctrl Pts',(-1.52686242875717,-1.,3.44469547527));
#41435=CARTESIAN_POINT('Ctrl Pts',(-1.52686242875717,1.,3.44469547527));
#41436=CARTESIAN_POINT('Ctrl Pts',(-1.52377348950429,-1.,3.43888895974182));
#41437=CARTESIAN_POINT('Ctrl Pts',(-1.52377348950429,1.,3.43888895974182));
#41438=CARTESIAN_POINT('Ctrl Pts',(-1.52134826724227,-1.,3.43417156977749));
#41439=CARTESIAN_POINT('Ctrl Pts',(-1.52134826724227,1.,3.43417156977749));
#41440=CARTESIAN_POINT('Ctrl Pts',(-1.51969006980792,-1.,3.43076036253384));
#41441=CARTESIAN_POINT('Ctrl Pts',(-1.51969006980792,1.,3.43076036253384));
#41442=CARTESIAN_POINT('Ctrl Pts',(-1.51901585838879,-1.,3.42915787669388));
#41443=CARTESIAN_POINT('Ctrl Pts',(-1.51901585838879,1.,3.42915787669388));
#41444=CARTESIAN_POINT('Ctrl Pts',(-1.51888450659497,-1.,3.42860527148835));
#41445=CARTESIAN_POINT('Ctrl Pts',(-1.51888450659497,1.,3.42860527148835));
#41446=CARTESIAN_POINT('Ctrl Pts',(-1.51896318668306,-1.,3.42852521763648));
#41447=CARTESIAN_POINT('Ctrl Pts',(-1.51896318668306,1.,3.42852521763648));
#41448=CARTESIAN_POINT('Ctrl Pts',(-1.519044091397,-1.,3.42855728381368));
#41449=CARTESIAN_POINT('Ctrl Pts',(-1.519044091397,1.,3.42855728381368));
#41450=CARTESIAN_POINT('',(-1.83867539237861,1.,3.77614523045147));
#41451=CARTESIAN_POINT('Ctrl Pts',(-1.83867539237861,1.,3.77614523045147));
#41452=CARTESIAN_POINT('Ctrl Pts',(-1.83742834010821,1.,3.77518714458232));
#41453=CARTESIAN_POINT('Ctrl Pts',(-1.83493697935064,1.,3.77326886065484));
#41454=CARTESIAN_POINT('Ctrl Pts',(-1.83120816956515,1.,3.77038509819777));
#41455=CARTESIAN_POINT('Ctrl Pts',(-1.82625289221933,1.,3.76652740355856));
#41456=CARTESIAN_POINT('Ctrl Pts',(-1.82008629694924,1.,3.76168412709652));
#41457=CARTESIAN_POINT('Ctrl Pts',(-1.81394729834032,1.,3.75681965683995));
#41458=CARTESIAN_POINT('Ctrl Pts',(-1.80783603939662,1.,3.75193395888069));
#41459=CARTESIAN_POINT('Ctrl Pts',(-1.80175271485519,1.,3.74702700874954));
#41460=CARTESIAN_POINT('Ctrl Pts',(-1.79569757859041,1.,3.74209880351667));
#41461=CARTESIAN_POINT('Ctrl Pts',(-1.78967092823139,1.,3.73714934729962));
#41462=CARTESIAN_POINT('Ctrl Pts',(-1.78367308442682,1.,3.73217863095022));
#41463=CARTESIAN_POINT('Ctrl Pts',(-1.77770437039606,1.,3.72718661205504));
#41464=CARTESIAN_POINT('Ctrl Pts',(-1.77176509401846,1.,3.72217319911429));
#41465=CARTESIAN_POINT('Ctrl Pts',(-1.76585552124549,1.,3.71713822377675));
#41466=CARTESIAN_POINT('Ctrl Pts',(-1.75997588499021,1.,3.71208146346454));
#41467=CARTESIAN_POINT('Ctrl Pts',(-1.75412641804148,1.,3.70700269736876));
#41468=CARTESIAN_POINT('Ctrl Pts',(-1.74830738046092,1.,3.70190175673422));
#41469=CARTESIAN_POINT('Ctrl Pts',(-1.74251908492589,1.,3.6967785691046));
#41470=CARTESIAN_POINT('Ctrl Pts',(-1.73676193254493,1.,3.69163322647906));
#41471=CARTESIAN_POINT('Ctrl Pts',(-1.73103640956647,1.,3.68646597019188));
#41472=CARTESIAN_POINT('Ctrl Pts',(-1.72534302437003,1.,3.68127704936472));
#41473=CARTESIAN_POINT('Ctrl Pts',(-1.71968225581787,1.,3.67606660374665));
#41474=CARTESIAN_POINT('Ctrl Pts',(-1.71405450210392,1.,3.67083454901629));
#41475=CARTESIAN_POINT('Ctrl Pts',(-1.70846001610983,1.,3.6655804319893));
#41476=CARTESIAN_POINT('Ctrl Pts',(-1.70289888566904,1.,3.6603033877491));
#41477=CARTESIAN_POINT('Ctrl Pts',(-1.69737117722559,1.,3.65500246526798));
#41478=CARTESIAN_POINT('Ctrl Pts',(-1.691877054817,1.,3.64967689827393));
#41479=CARTESIAN_POINT('Ctrl Pts',(-1.68641690471455,1.,3.64432638915199));
#41480=CARTESIAN_POINT('Ctrl Pts',(-1.68099146651577,1.,3.63895140887443));
#41481=CARTESIAN_POINT('Ctrl Pts',(-1.67560193613145,1.,3.63355343201211));
#41482=CARTESIAN_POINT('Ctrl Pts',(-1.67024966008037,1.,3.62813422105257));
#41483=CARTESIAN_POINT('Ctrl Pts',(-1.66493585923853,1.,3.62269517989104));
#41484=CARTESIAN_POINT('Ctrl Pts',(-1.65966133399186,1.,3.61723666482457));
#41485=CARTESIAN_POINT('Ctrl Pts',(-1.65442619244327,1.,3.61175734965129));
#41486=CARTESIAN_POINT('Ctrl Pts',(-1.64922952425833,1.,3.60625346556992));
#41487=CARTESIAN_POINT('Ctrl Pts',(-1.6440700438558,1.,3.6007202851384));
#41488=CARTESIAN_POINT('Ctrl Pts',(-1.63894676675349,1.,3.59515368334887));
#41489=CARTESIAN_POINT('Ctrl Pts',(-1.63385971451259,1.,3.58955176627876));
#41490=CARTESIAN_POINT('Ctrl Pts',(-1.62881051550748,1.,3.5839162577435));
#41491=CARTESIAN_POINT('Ctrl Pts',(-1.62380329464851,1.,3.57825455954405));
#41492=CARTESIAN_POINT('Ctrl Pts',(-1.61884340915412,1.,3.57257679609826));
#41493=CARTESIAN_POINT('Ctrl Pts',(-1.61393581747522,1.,3.56689200468404));
#41494=CARTESIAN_POINT('Ctrl Pts',(-1.60908344685459,1.,3.56120432482986));
#41495=CARTESIAN_POINT('Ctrl Pts',(-1.60428584699848,1.,3.55550985096117));
#41496=CARTESIAN_POINT('Ctrl Pts',(-1.59953698113444,1.,3.54979148634426));
#41497=CARTESIAN_POINT('Ctrl Pts',(-1.5948276694975,1.,3.544024581823));
#41498=CARTESIAN_POINT('Ctrl Pts',(-1.59014958368725,1.,3.53818616861045));
#41499=CARTESIAN_POINT('Ctrl Pts',(-1.58549906268083,1.,3.53226378147068));
#41500=CARTESIAN_POINT('Ctrl Pts',(-1.58088027227856,1.,3.52626275334899));
#41501=CARTESIAN_POINT('Ctrl Pts',(-1.5763104998818,1.,3.52021847865961));
#41502=CARTESIAN_POINT('Ctrl Pts',(-1.57181569799774,1.,3.51418598431733));
#41503=CARTESIAN_POINT('Ctrl Pts',(-1.56742097575041,1.,3.50821771695427));
#41504=CARTESIAN_POINT('Ctrl Pts',(-1.56314187758689,1.,3.50234321621607));
#41505=CARTESIAN_POINT('Ctrl Pts',(-1.55897703097859,1.,3.49655185179623));
#41506=CARTESIAN_POINT('Ctrl Pts',(-1.5548959590107,1.,3.49076460877317));
#41507=CARTESIAN_POINT('Ctrl Pts',(-1.55084702970382,1.,3.48485155928414));
#41508=CARTESIAN_POINT('Ctrl Pts',(-1.54678009290207,1.,3.47868272898599));
#41509=CARTESIAN_POINT('Ctrl Pts',(-1.54266605398152,1.,3.47217189224576));
#41510=CARTESIAN_POINT('Ctrl Pts',(-1.53851507915533,1.,3.46531752207222));
#41511=CARTESIAN_POINT('Ctrl Pts',(-1.53440195378902,1.,3.45825932955273));
#41512=CARTESIAN_POINT('Ctrl Pts',(-1.530462444618,1.,3.45127136828667));
#41513=CARTESIAN_POINT('Ctrl Pts',(-1.52686242875717,1.,3.44469547527));
#41514=CARTESIAN_POINT('Ctrl Pts',(-1.52377348950429,1.,3.43888895974182));
#41515=CARTESIAN_POINT('Ctrl Pts',(-1.52134826724227,1.,3.43417156977749));
#41516=CARTESIAN_POINT('Ctrl Pts',(-1.5198144909343,1.,3.4310163189349));
#41517=CARTESIAN_POINT('Ctrl Pts',(-1.51914806898539,1.,3.42946838852728));
#41518=CARTESIAN_POINT('Ctrl Pts',(-1.51895133295017,1.,3.42884302333978));
#41519=CARTESIAN_POINT('Ctrl Pts',(-1.51893924967231,1.,3.42864616361967));
#41520=CARTESIAN_POINT('Ctrl Pts',(-1.51895082866166,1.,3.42859860294378));
#41521=CARTESIAN_POINT('',(-1.83867539237861,0.,3.77614523045147));
#41522=CARTESIAN_POINT('Ctrl Pts',(-1.88088939428811,-1.,3.24418789321065));
#41523=CARTESIAN_POINT('Ctrl Pts',(-1.88088939428811,1.,3.24418789321065));
#41524=CARTESIAN_POINT('Ctrl Pts',(-1.8809110068042,-1.,3.24410359189733));
#41525=CARTESIAN_POINT('Ctrl Pts',(-1.8809110068042,1.,3.24410359189733));
#41526=CARTESIAN_POINT('Ctrl Pts',(-1.8810220187274,-1.,3.24408699284449));
#41527=CARTESIAN_POINT('Ctrl Pts',(-1.8810220187274,1.,3.24408699284449));
#41528=CARTESIAN_POINT('Ctrl Pts',(-1.88139187908347,-1.,3.24451807186964));
#41529=CARTESIAN_POINT('Ctrl Pts',(-1.88139187908347,1.,3.24451807186964));
#41530=CARTESIAN_POINT('Ctrl Pts',(-1.88229202583187,-1.,3.24600543790876));
#41531=CARTESIAN_POINT('Ctrl Pts',(-1.88229202583187,1.,3.24600543790876));
#41532=CARTESIAN_POINT('Ctrl Pts',(-1.88407708646435,-1.,3.24935200512055));
#41533=CARTESIAN_POINT('Ctrl Pts',(-1.88407708646435,1.,3.24935200512055));
#41534=CARTESIAN_POINT('Ctrl Pts',(-1.88646802523372,-1.,3.25408686339298));
#41535=CARTESIAN_POINT('Ctrl Pts',(-1.88646802523372,1.,3.25408686339298));
#41536=CARTESIAN_POINT('Ctrl Pts',(-1.88934996203508,-1.,3.2599988519361));
#41537=CARTESIAN_POINT('Ctrl Pts',(-1.88934996203508,1.,3.2599988519361));
#41538=CARTESIAN_POINT('Ctrl Pts',(-1.89255393500769,-1.,3.2667765388833));
#41539=CARTESIAN_POINT('Ctrl Pts',(-1.89255393500769,1.,3.2667765388833));
#41540=CARTESIAN_POINT('Ctrl Pts',(-1.89589172903662,-1.,3.27407108932908));
#41541=CARTESIAN_POINT('Ctrl Pts',(-1.89589172903662,1.,3.27407108932908));
#41542=CARTESIAN_POINT('Ctrl Pts',(-1.89918429230425,-1.,3.28154737912287));
#41543=CARTESIAN_POINT('Ctrl Pts',(-1.89918429230425,1.,3.28154737912287));
#41544=CARTESIAN_POINT('Ctrl Pts',(-1.9022897124757,-1.,3.28893448600364));
#41545=CARTESIAN_POINT('Ctrl Pts',(-1.9022897124757,1.,3.28893448600364));
#41546=CARTESIAN_POINT('Ctrl Pts',(-1.9051389186417,-1.,3.29608978722258));
#41547=CARTESIAN_POINT('Ctrl Pts',(-1.9051389186417,1.,3.29608978722258));
#41548=CARTESIAN_POINT('Ctrl Pts',(-1.90773912171424,-1.,3.30300595568341));
#41549=CARTESIAN_POINT('Ctrl Pts',(-1.90773912171424,1.,3.30300595568341));
#41550=CARTESIAN_POINT('Ctrl Pts',(-1.91014297830502,-1.,3.30975721158694));
#41551=CARTESIAN_POINT('Ctrl Pts',(-1.91014297830502,1.,3.30975721158694));
#41552=CARTESIAN_POINT('Ctrl Pts',(-1.91242616234459,-1.,3.31646052426395));
#41553=CARTESIAN_POINT('Ctrl Pts',(-1.91242616234459,1.,3.31646052426395));
#41554=CARTESIAN_POINT('Ctrl Pts',(-1.91466343916612,-1.,3.32323403454507));
#41555=CARTESIAN_POINT('Ctrl Pts',(-1.91466343916612,1.,3.32323403454507));
#41556=CARTESIAN_POINT('Ctrl Pts',(-1.91690081930297,-1.,3.33014884257812));
#41557=CARTESIAN_POINT('Ctrl Pts',(-1.91690081930297,1.,3.33014884257812));
#41558=CARTESIAN_POINT('Ctrl Pts',(-1.91914609610173,-1.,3.33721230709948));
#41559=CARTESIAN_POINT('Ctrl Pts',(-1.91914609610173,1.,3.33721230709948));
#41560=CARTESIAN_POINT('Ctrl Pts',(-1.92138450828378,-1.,3.34439448941915));
#41561=CARTESIAN_POINT('Ctrl Pts',(-1.92138450828378,1.,3.34439448941915));
#41562=CARTESIAN_POINT('Ctrl Pts',(-1.92358838440518,-1.,3.35164424847206));
#41563=CARTESIAN_POINT('Ctrl Pts',(-1.92358838440518,1.,3.35164424847206));
#41564=CARTESIAN_POINT('Ctrl Pts',(-1.92572846125763,-1.,3.35890824422976));
#41565=CARTESIAN_POINT('Ctrl Pts',(-1.92572846125763,1.,3.35890824422976));
#41566=CARTESIAN_POINT('Ctrl Pts',(-1.92778626543803,-1.,3.36615168657597));
#41567=CARTESIAN_POINT('Ctrl Pts',(-1.92778626543803,1.,3.36615168657597));
#41568=CARTESIAN_POINT('Ctrl Pts',(-1.92975993109897,-1.,3.37336807068078));
#41569=CARTESIAN_POINT('Ctrl Pts',(-1.92975993109897,1.,3.37336807068078));
#41570=CARTESIAN_POINT('Ctrl Pts',(-1.93165739093292,-1.,3.38056768525577));
#41571=CARTESIAN_POINT('Ctrl Pts',(-1.93165739093292,1.,3.38056768525577));
#41572=CARTESIAN_POINT('Ctrl Pts',(-1.93349233176794,-1.,3.38777076883267));
#41573=CARTESIAN_POINT('Ctrl Pts',(-1.93349233176794,1.,3.38777076883267));
#41574=CARTESIAN_POINT('Ctrl Pts',(-1.93527929945982,-1.,3.39499923640789));
#41575=CARTESIAN_POINT('Ctrl Pts',(-1.93527929945982,1.,3.39499923640789));
#41576=CARTESIAN_POINT('Ctrl Pts',(-1.93702857723089,-1.,3.40226802104093));
#41577=CARTESIAN_POINT('Ctrl Pts',(-1.93702857723089,1.,3.40226802104093));
#41578=CARTESIAN_POINT('Ctrl Pts',(-1.93874306008132,-1.,3.40957978266622));
#41579=CARTESIAN_POINT('Ctrl Pts',(-1.93874306008132,1.,3.40957978266622));
#41580=CARTESIAN_POINT('Ctrl Pts',(-1.94042111965237,-1.,3.41692971994082));
#41581=CARTESIAN_POINT('Ctrl Pts',(-1.94042111965237,1.,3.41692971994082));
#41582=CARTESIAN_POINT('Ctrl Pts',(-1.94205835913692,-1.,3.42430850941497));
#41583=CARTESIAN_POINT('Ctrl Pts',(-1.94205835913692,1.,3.42430850941497));
#41584=CARTESIAN_POINT('Ctrl Pts',(-1.94364973660285,-1.,3.43170586602436));
#41585=CARTESIAN_POINT('Ctrl Pts',(-1.94364973660285,1.,3.43170586602436));
#41586=CARTESIAN_POINT('Ctrl Pts',(-1.94519168842883,-1.,3.43911410197693));
#41587=CARTESIAN_POINT('Ctrl Pts',(-1.94519168842883,1.,3.43911410197693));
#41588=CARTESIAN_POINT('Ctrl Pts',(-1.94668377715332,-1.,3.44653088665685));
#41589=CARTESIAN_POINT('Ctrl Pts',(-1.94668377715332,1.,3.44653088665685));
#41590=CARTESIAN_POINT('Ctrl Pts',(-1.94812754766524,-1.,3.45395731584051));
#41591=CARTESIAN_POINT('Ctrl Pts',(-1.94812754766524,1.,3.45395731584051));
#41592=CARTESIAN_POINT('Ctrl Pts',(-1.94952575850196,-1.,3.46139661060959));
#41593=CARTESIAN_POINT('Ctrl Pts',(-1.94952575850196,1.,3.46139661060959));
#41594=CARTESIAN_POINT('Ctrl Pts',(-1.95088147859876,-1.,3.4688525897419));
#41595=CARTESIAN_POINT('Ctrl Pts',(-1.95088147859876,1.,3.4688525897419));
#41596=CARTESIAN_POINT('Ctrl Pts',(-1.95219722189878,-1.,3.47632820495926));
#41597=CARTESIAN_POINT('Ctrl Pts',(-1.95219722189878,1.,3.47632820495926));
#41598=CARTESIAN_POINT('Ctrl Pts',(-1.95347412486316,-1.,3.48382414832648));
#41599=CARTESIAN_POINT('Ctrl Pts',(-1.95347412486316,1.,3.48382414832648));
#41600=CARTESIAN_POINT('Ctrl Pts',(-1.95471236969653,-1.,3.49133956289154));
#41601=CARTESIAN_POINT('Ctrl Pts',(-1.95471236969653,1.,3.49133956289154));
#41602=CARTESIAN_POINT('Ctrl Pts',(-1.9559115382367,-1.,3.49887263575602));
#41603=CARTESIAN_POINT('Ctrl Pts',(-1.9559115382367,1.,3.49887263575602));
#41604=CARTESIAN_POINT('Ctrl Pts',(-1.95707099606514,-1.,3.50642124159913));
#41605=CARTESIAN_POINT('Ctrl Pts',(-1.95707099606514,1.,3.50642124159913));
#41606=CARTESIAN_POINT('Ctrl Pts',(-1.95819025316768,-1.,3.51398354617772));
#41607=CARTESIAN_POINT('Ctrl Pts',(-1.95819025316768,1.,3.51398354617772));
#41608=CARTESIAN_POINT('Ctrl Pts',(-1.95926936324436,-1.,3.52155867431438));
#41609=CARTESIAN_POINT('Ctrl Pts',(-1.95926936324436,1.,3.52155867431438));
#41610=CARTESIAN_POINT('Ctrl Pts',(-1.96030879411534,-1.,3.52914648844289));
#41611=CARTESIAN_POINT('Ctrl Pts',(-1.96030879411534,1.,3.52914648844289));
#41612=CARTESIAN_POINT('Ctrl Pts',(-1.96130926212661,-1.,3.53674730625759));
#41613=CARTESIAN_POINT('Ctrl Pts',(-1.96130926212661,1.,3.53674730625759));
#41614=CARTESIAN_POINT('Ctrl Pts',(-1.96227157573058,-1.,3.54436163300425));
#41615=CARTESIAN_POINT('Ctrl Pts',(-1.96227157573058,1.,3.54436163300425));
#41616=CARTESIAN_POINT('Ctrl Pts',(-1.96319648628667,-1.,3.55198990600929));
#41617=CARTESIAN_POINT('Ctrl Pts',(-1.96319648628667,1.,3.55198990600929));
#41618=CARTESIAN_POINT('Ctrl Pts',(-1.96408450906868,-1.,3.55963218706201));
#41619=CARTESIAN_POINT('Ctrl Pts',(-1.96408450906868,1.,3.55963218706201));
#41620=CARTESIAN_POINT('Ctrl Pts',(-1.96493594634643,-1.,3.56728820357933));
#41621=CARTESIAN_POINT('Ctrl Pts',(-1.96493594634643,1.,3.56728820357933));
#41622=CARTESIAN_POINT('Ctrl Pts',(-1.96575096652857,-1.,3.57495748601088));
#41623=CARTESIAN_POINT('Ctrl Pts',(-1.96575096652857,1.,3.57495748601088));
#41624=CARTESIAN_POINT('Ctrl Pts',(-1.9665296668894,-1.,3.58263947663884));
#41625=CARTESIAN_POINT('Ctrl Pts',(-1.9665296668894,1.,3.58263947663884));
#41626=CARTESIAN_POINT('Ctrl Pts',(-1.96727213799507,-1.,3.5903336402273));
#41627=CARTESIAN_POINT('Ctrl Pts',(-1.96727213799507,1.,3.5903336402273));
#41628=CARTESIAN_POINT('Ctrl Pts',(-1.96797854118257,-1.,3.59803959819725));
#41629=CARTESIAN_POINT('Ctrl Pts',(-1.96797854118257,1.,3.59803959819725));
#41630=CARTESIAN_POINT('Ctrl Pts',(-1.96864911885775,-1.,3.60575714017676));
#41631=CARTESIAN_POINT('Ctrl Pts',(-1.96864911885775,1.,3.60575714017676));
#41632=CARTESIAN_POINT('Ctrl Pts',(-1.96928416040712,-1.,3.61348615496393));
#41633=CARTESIAN_POINT('Ctrl Pts',(-1.96928416040712,1.,3.61348615496393));
#41634=CARTESIAN_POINT('Ctrl Pts',(-1.96988398129888,-1.,3.62122658401722));
#41635=CARTESIAN_POINT('Ctrl Pts',(-1.96988398129888,1.,3.62122658401722));
#41636=CARTESIAN_POINT('Ctrl Pts',(-1.97044889850518,-1.,3.62897836973397));
#41637=CARTESIAN_POINT('Ctrl Pts',(-1.97044889850518,1.,3.62897836973397));
#41638=CARTESIAN_POINT('Ctrl Pts',(-1.97097920454698,-1.,3.63674139590853));
#41639=CARTESIAN_POINT('Ctrl Pts',(-1.97097920454698,1.,3.63674139590853));
#41640=CARTESIAN_POINT('Ctrl Pts',(-1.97147515441539,-1.,3.64451546724221));
#41641=CARTESIAN_POINT('Ctrl Pts',(-1.97147515441539,1.,3.64451546724221));
#41642=CARTESIAN_POINT('Ctrl Pts',(-1.97193697240645,-1.,3.65230034717364));
#41643=CARTESIAN_POINT('Ctrl Pts',(-1.97193697240645,1.,3.65230034717364));
#41644=CARTESIAN_POINT('Ctrl Pts',(-1.97236485439317,-1.,3.66009578166865));
#41645=CARTESIAN_POINT('Ctrl Pts',(-1.97236485439317,1.,3.66009578166865));
#41646=CARTESIAN_POINT('Ctrl Pts',(-1.9727589719863,-1.,3.66790152751984));
#41647=CARTESIAN_POINT('Ctrl Pts',(-1.9727589719863,1.,3.66790152751984));
#41648=CARTESIAN_POINT('Ctrl Pts',(-1.97311947678035,-1.,3.67571738106175));
#41649=CARTESIAN_POINT('Ctrl Pts',(-1.97311947678035,1.,3.67571738106175));
#41650=CARTESIAN_POINT('Ctrl Pts',(-1.97344650303631,-1.,3.68354319913416));
#41651=CARTESIAN_POINT('Ctrl Pts',(-1.97344650303631,1.,3.68354319913416));
#41652=CARTESIAN_POINT('Ctrl Pts',(-1.97374016224397,-1.,3.69137888597855));
#41653=CARTESIAN_POINT('Ctrl Pts',(-1.97374016224397,1.,3.69137888597855));
#41654=CARTESIAN_POINT('Ctrl Pts',(-1.97394846382289,-1.,3.69765528558292));
#41655=CARTESIAN_POINT('Ctrl Pts',(-1.97394846382289,1.,3.69765528558292));
#41656=CARTESIAN_POINT('Ctrl Pts',(-1.97408973726149,-1.,3.70236698911837));
#41657=CARTESIAN_POINT('Ctrl Pts',(-1.97408973726149,1.,3.70236698911837));
#41658=CARTESIAN_POINT('Ctrl Pts',(-1.974177276451,-1.,3.7055100813194));
#41659=CARTESIAN_POINT('Ctrl Pts',(-1.974177276451,1.,3.7055100813194));
#41660=CARTESIAN_POINT('Ctrl Pts',(-1.97421938526992,-1.,3.70708211654725));
#41661=CARTESIAN_POINT('Ctrl Pts',(-1.97421938526992,1.,3.70708211654725));
#41662=CARTESIAN_POINT('',(-1.88097764062542,1.,3.24413672884902));
#41663=CARTESIAN_POINT('Ctrl Pts',(-1.88097764062542,-1.,3.24413672884902));
#41664=CARTESIAN_POINT('Ctrl Pts',(-1.88097764062542,-0.666666666666667,
3.24413672884902));
#41665=CARTESIAN_POINT('Ctrl Pts',(-1.88097764062542,-0.333333333333333,
3.24413672884902));
#41666=CARTESIAN_POINT('Ctrl Pts',(-1.88097764062542,0.333333333333333,
3.24413672884902));
#41667=CARTESIAN_POINT('Ctrl Pts',(-1.88097764062542,0.666666666666667,
3.24413672884902));
#41668=CARTESIAN_POINT('Ctrl Pts',(-1.88097764062542,1.,3.24413672884902));
#41669=CARTESIAN_POINT('',(-1.97421938526992,1.,3.70708211654725));
#41670=CARTESIAN_POINT('',(-1.97421938526992,0.,3.70708211654725));
#41671=CARTESIAN_POINT('Ctrl Pts',(-1.88097764062542,1.,3.24413672884902));
#41672=CARTESIAN_POINT('Ctrl Pts',(-1.88102292397987,1.,3.24415531671311));
#41673=CARTESIAN_POINT('Ctrl Pts',(-1.88117508446657,1.,3.24428080352952));
#41674=CARTESIAN_POINT('Ctrl Pts',(-1.88156537699118,1.,3.24480754675942));
#41675=CARTESIAN_POINT('Ctrl Pts',(-1.88242596600422,1.,3.24625654410705));
#41676=CARTESIAN_POINT('Ctrl Pts',(-1.88407708646435,1.,3.24935200512055));
#41677=CARTESIAN_POINT('Ctrl Pts',(-1.88646802523372,1.,3.25408686339298));
#41678=CARTESIAN_POINT('Ctrl Pts',(-1.88934996203508,1.,3.2599988519361));
#41679=CARTESIAN_POINT('Ctrl Pts',(-1.89255393500769,1.,3.2667765388833));
#41680=CARTESIAN_POINT('Ctrl Pts',(-1.89589172903662,1.,3.27407108932908));
#41681=CARTESIAN_POINT('Ctrl Pts',(-1.89918429230425,1.,3.28154737912287));
#41682=CARTESIAN_POINT('Ctrl Pts',(-1.9022897124757,1.,3.28893448600364));
#41683=CARTESIAN_POINT('Ctrl Pts',(-1.9051389186417,1.,3.29608978722258));
#41684=CARTESIAN_POINT('Ctrl Pts',(-1.90773912171424,1.,3.30300595568341));
#41685=CARTESIAN_POINT('Ctrl Pts',(-1.91014297830502,1.,3.30975721158694));
#41686=CARTESIAN_POINT('Ctrl Pts',(-1.91242616234459,1.,3.31646052426395));
#41687=CARTESIAN_POINT('Ctrl Pts',(-1.91466343916612,1.,3.32323403454507));
#41688=CARTESIAN_POINT('Ctrl Pts',(-1.91690081930297,1.,3.33014884257812));
#41689=CARTESIAN_POINT('Ctrl Pts',(-1.91914609610173,1.,3.33721230709948));
#41690=CARTESIAN_POINT('Ctrl Pts',(-1.92138450828378,1.,3.34439448941915));
#41691=CARTESIAN_POINT('Ctrl Pts',(-1.92358838440518,1.,3.35164424847206));
#41692=CARTESIAN_POINT('Ctrl Pts',(-1.92572846125763,1.,3.35890824422976));
#41693=CARTESIAN_POINT('Ctrl Pts',(-1.92778626543803,1.,3.36615168657597));
#41694=CARTESIAN_POINT('Ctrl Pts',(-1.92975993109897,1.,3.37336807068078));
#41695=CARTESIAN_POINT('Ctrl Pts',(-1.93165739093292,1.,3.38056768525577));
#41696=CARTESIAN_POINT('Ctrl Pts',(-1.93349233176794,1.,3.38777076883267));
#41697=CARTESIAN_POINT('Ctrl Pts',(-1.93527929945982,1.,3.39499923640789));
#41698=CARTESIAN_POINT('Ctrl Pts',(-1.93702857723089,1.,3.40226802104093));
#41699=CARTESIAN_POINT('Ctrl Pts',(-1.93874306008132,1.,3.40957978266622));
#41700=CARTESIAN_POINT('Ctrl Pts',(-1.94042111965237,1.,3.41692971994082));
#41701=CARTESIAN_POINT('Ctrl Pts',(-1.94205835913692,1.,3.42430850941497));
#41702=CARTESIAN_POINT('Ctrl Pts',(-1.94364973660285,1.,3.43170586602436));
#41703=CARTESIAN_POINT('Ctrl Pts',(-1.94519168842883,1.,3.43911410197693));
#41704=CARTESIAN_POINT('Ctrl Pts',(-1.94668377715332,1.,3.44653088665685));
#41705=CARTESIAN_POINT('Ctrl Pts',(-1.94812754766524,1.,3.45395731584051));
#41706=CARTESIAN_POINT('Ctrl Pts',(-1.94952575850196,1.,3.46139661060959));
#41707=CARTESIAN_POINT('Ctrl Pts',(-1.95088147859876,1.,3.4688525897419));
#41708=CARTESIAN_POINT('Ctrl Pts',(-1.95219722189878,1.,3.47632820495926));
#41709=CARTESIAN_POINT('Ctrl Pts',(-1.95347412486316,1.,3.48382414832648));
#41710=CARTESIAN_POINT('Ctrl Pts',(-1.95471236969653,1.,3.49133956289154));
#41711=CARTESIAN_POINT('Ctrl Pts',(-1.9559115382367,1.,3.49887263575602));
#41712=CARTESIAN_POINT('Ctrl Pts',(-1.95707099606514,1.,3.50642124159913));
#41713=CARTESIAN_POINT('Ctrl Pts',(-1.95819025316768,1.,3.51398354617772));
#41714=CARTESIAN_POINT('Ctrl Pts',(-1.95926936324436,1.,3.52155867431438));
#41715=CARTESIAN_POINT('Ctrl Pts',(-1.96030879411534,1.,3.52914648844289));
#41716=CARTESIAN_POINT('Ctrl Pts',(-1.96130926212661,1.,3.53674730625759));
#41717=CARTESIAN_POINT('Ctrl Pts',(-1.96227157573058,1.,3.54436163300425));
#41718=CARTESIAN_POINT('Ctrl Pts',(-1.96319648628667,1.,3.55198990600929));
#41719=CARTESIAN_POINT('Ctrl Pts',(-1.96408450906868,1.,3.55963218706201));
#41720=CARTESIAN_POINT('Ctrl Pts',(-1.96493594634643,1.,3.56728820357933));
#41721=CARTESIAN_POINT('Ctrl Pts',(-1.96575096652857,1.,3.57495748601088));
#41722=CARTESIAN_POINT('Ctrl Pts',(-1.9665296668894,1.,3.58263947663884));
#41723=CARTESIAN_POINT('Ctrl Pts',(-1.96727213799507,1.,3.5903336402273));
#41724=CARTESIAN_POINT('Ctrl Pts',(-1.96797854118257,1.,3.59803959819725));
#41725=CARTESIAN_POINT('Ctrl Pts',(-1.96864911885775,1.,3.60575714017676));
#41726=CARTESIAN_POINT('Ctrl Pts',(-1.96928416040712,1.,3.61348615496393));
#41727=CARTESIAN_POINT('Ctrl Pts',(-1.96988398129888,1.,3.62122658401722));
#41728=CARTESIAN_POINT('Ctrl Pts',(-1.97044889850518,1.,3.62897836973397));
#41729=CARTESIAN_POINT('Ctrl Pts',(-1.97097920454698,1.,3.63674139590853));
#41730=CARTESIAN_POINT('Ctrl Pts',(-1.97147515441539,1.,3.64451546724221));
#41731=CARTESIAN_POINT('Ctrl Pts',(-1.97193697240645,1.,3.65230034717364));
#41732=CARTESIAN_POINT('Ctrl Pts',(-1.97236485439317,1.,3.66009578166865));
#41733=CARTESIAN_POINT('Ctrl Pts',(-1.9727589719863,1.,3.66790152751984));
#41734=CARTESIAN_POINT('Ctrl Pts',(-1.97311947678035,1.,3.67571738106175));
#41735=CARTESIAN_POINT('Ctrl Pts',(-1.97344650303631,1.,3.68354319913416));
#41736=CARTESIAN_POINT('Ctrl Pts',(-1.97374016224397,1.,3.69137888597855));
#41737=CARTESIAN_POINT('Ctrl Pts',(-1.97394846382289,1.,3.69765528558292));
#41738=CARTESIAN_POINT('Ctrl Pts',(-1.97408973726149,1.,3.70236698911837));
#41739=CARTESIAN_POINT('Ctrl Pts',(-1.974177276451,1.,3.7055100813194));
#41740=CARTESIAN_POINT('Ctrl Pts',(-1.97421938526992,1.,3.70708211654725));
#41741=CARTESIAN_POINT('Origin',(-1.97421938526992,0.,3.70708211654725));
#41742=CARTESIAN_POINT('',(-1.83867539237861,1.,3.77614523045147));
#41743=CARTESIAN_POINT('Origin',(0.,0.,0.));
#41744=CARTESIAN_POINT('',(-2.03660101169564,1.,3.14877060440425));
#41745=CARTESIAN_POINT('Origin',(0.,1.,0.));
#41746=CARTESIAN_POINT('Ctrl Pts',(-2.03660101169564,1.,3.14877060440425));
#41747=CARTESIAN_POINT('Ctrl Pts',(-2.03660101169564,0.666666666666667,
3.14877060440425));
#41748=CARTESIAN_POINT('Ctrl Pts',(-2.03660101169564,0.333333333333333,
3.14877060440425));
#41749=CARTESIAN_POINT('Ctrl Pts',(-2.03660101169564,-0.333333333333333,
3.14877060440425));
#41750=CARTESIAN_POINT('Ctrl Pts',(-2.03660101169564,-0.666666666666667,
3.14877060440425));
#41751=CARTESIAN_POINT('Ctrl Pts',(-2.03660101169564,-1.,3.14877060440425));
#41752=CARTESIAN_POINT('Ctrl Pts',(-2.40675750623143,-1.,3.44202241512147));
#41753=CARTESIAN_POINT('Ctrl Pts',(-2.40675750623143,1.,3.44202241512147));
#41754=CARTESIAN_POINT('Ctrl Pts',(-2.40537592959345,-1.,3.44127120683402));
#41755=CARTESIAN_POINT('Ctrl Pts',(-2.40537592959345,1.,3.44127120683402));
#41756=CARTESIAN_POINT('Ctrl Pts',(-2.40261515590099,-1.,3.43976627485223));
#41757=CARTESIAN_POINT('Ctrl Pts',(-2.40261515590099,1.,3.43976627485223));
#41758=CARTESIAN_POINT('Ctrl Pts',(-2.39848113411429,-1.,3.43750133066036));
#41759=CARTESIAN_POINT('Ctrl Pts',(-2.39848113411429,1.,3.43750133066036));
#41760=CARTESIAN_POINT('Ctrl Pts',(-2.39298338805823,-1.,3.43446630680436));
#41761=CARTESIAN_POINT('Ctrl Pts',(-2.39298338805823,1.,3.43446630680436));
#41762=CARTESIAN_POINT('Ctrl Pts',(-2.38613505844641,-1.,3.43064732714472));
#41763=CARTESIAN_POINT('Ctrl Pts',(-2.38613505844641,1.,3.43064732714472));
#41764=CARTESIAN_POINT('Ctrl Pts',(-2.37931067029517,-1.,3.42680309755241));
#41765=CARTESIAN_POINT('Ctrl Pts',(-2.37931067029517,1.,3.42680309755241));
#41766=CARTESIAN_POINT('Ctrl Pts',(-2.37251035954351,-1.,3.42293356216595));
#41767=CARTESIAN_POINT('Ctrl Pts',(-2.37251035954351,1.,3.42293356216595));
#41768=CARTESIAN_POINT('Ctrl Pts',(-2.36573431470314,-1.,3.41903866635384));
#41769=CARTESIAN_POINT('Ctrl Pts',(-2.36573431470314,1.,3.41903866635384));
#41770=CARTESIAN_POINT('Ctrl Pts',(-2.35898278606449,-1.,3.4151183675076));
#41771=CARTESIAN_POINT('Ctrl Pts',(-2.35898278606449,1.,3.4151183675076));
#41772=CARTESIAN_POINT('Ctrl Pts',(-2.35225606823649,-1.,3.41117262313464));
#41773=CARTESIAN_POINT('Ctrl Pts',(-2.35225606823649,1.,3.41117262313464));
#41774=CARTESIAN_POINT('Ctrl Pts',(-2.34555447648901,-1.,3.40720137403888));
#41775=CARTESIAN_POINT('Ctrl Pts',(-2.34555447648901,1.,3.40720137403888));
#41776=CARTESIAN_POINT('Ctrl Pts',(-2.33887832342715,-1.,3.40320452776646));
#41777=CARTESIAN_POINT('Ctrl Pts',(-2.33887832342715,1.,3.40320452776646));
#41778=CARTESIAN_POINT('Ctrl Pts',(-2.33222789882601,-1.,3.39918194578115));
#41779=CARTESIAN_POINT('Ctrl Pts',(-2.33222789882601,1.,3.39918194578115));
#41780=CARTESIAN_POINT('Ctrl Pts',(-2.32560343902683,-1.,3.39513342020045));
#41781=CARTESIAN_POINT('Ctrl Pts',(-2.32560343902683,1.,3.39513342020045));
#41782=CARTESIAN_POINT('Ctrl Pts',(-2.31900513925627,-1.,3.39105869475112));
#41783=CARTESIAN_POINT('Ctrl Pts',(-2.31900513925627,1.,3.39105869475112));
#41784=CARTESIAN_POINT('Ctrl Pts',(-2.31243319489505,-1.,3.38695751492659));
#41785=CARTESIAN_POINT('Ctrl Pts',(-2.31243319489505,1.,3.38695751492659));
#41786=CARTESIAN_POINT('Ctrl Pts',(-2.30588783640389,-1.,3.38282967336676));
#41787=CARTESIAN_POINT('Ctrl Pts',(-2.30588783640389,1.,3.38282967336676));
#41788=CARTESIAN_POINT('Ctrl Pts',(-2.29936936127588,-1.,3.37867504959382));
#41789=CARTESIAN_POINT('Ctrl Pts',(-2.29936936127588,1.,3.37867504959382));
#41790=CARTESIAN_POINT('Ctrl Pts',(-2.2928781800731,-1.,3.37449367172707));
#41791=CARTESIAN_POINT('Ctrl Pts',(-2.2928781800731,1.,3.37449367172707));
#41792=CARTESIAN_POINT('Ctrl Pts',(-2.28641481081045,-1.,3.37028570206357));
#41793=CARTESIAN_POINT('Ctrl Pts',(-2.28641481081045,1.,3.37028570206357));
#41794=CARTESIAN_POINT('Ctrl Pts',(-2.27997979457968,-1.,3.36605130712978));
#41795=CARTESIAN_POINT('Ctrl Pts',(-2.27997979457968,1.,3.36605130712978));
#41796=CARTESIAN_POINT('Ctrl Pts',(-2.27357362620902,-1.,3.36179055004369));
#41797=CARTESIAN_POINT('Ctrl Pts',(-2.27357362620902,1.,3.36179055004369));
#41798=CARTESIAN_POINT('Ctrl Pts',(-2.26719668579921,-1.,3.35750328523077));
#41799=CARTESIAN_POINT('Ctrl Pts',(-2.26719668579921,1.,3.35750328523077));
#41800=CARTESIAN_POINT('Ctrl Pts',(-2.26084915222484,-1.,3.35318902552676));
#41801=CARTESIAN_POINT('Ctrl Pts',(-2.26084915222484,1.,3.35318902552676));
#41802=CARTESIAN_POINT('Ctrl Pts',(-2.25453097693524,-1.,3.34884690292342));
#41803=CARTESIAN_POINT('Ctrl Pts',(-2.25453097693524,1.,3.34884690292342));
#41804=CARTESIAN_POINT('Ctrl Pts',(-2.24824207678288,-1.,3.34447596770768));
#41805=CARTESIAN_POINT('Ctrl Pts',(-2.24824207678288,1.,3.34447596770768));
#41806=CARTESIAN_POINT('Ctrl Pts',(-2.24198249391437,-1.,3.34007543738044));
#41807=CARTESIAN_POINT('Ctrl Pts',(-2.24198249391437,1.,3.34007543738044));
#41808=CARTESIAN_POINT('Ctrl Pts',(-2.2357525632881,-1.,3.33564495756478));
#41809=CARTESIAN_POINT('Ctrl Pts',(-2.2357525632881,1.,3.33564495756478));
#41810=CARTESIAN_POINT('Ctrl Pts',(-2.22955308907221,-1.,3.33118487773593));
#41811=CARTESIAN_POINT('Ctrl Pts',(-2.22955308907221,1.,3.33118487773593));
#41812=CARTESIAN_POINT('Ctrl Pts',(-2.22338548312758,-1.,3.32669646722871));
#41813=CARTESIAN_POINT('Ctrl Pts',(-2.22338548312758,1.,3.32669646722871));
#41814=CARTESIAN_POINT('Ctrl Pts',(-2.21725135110889,-1.,3.32218125618955));
#41815=CARTESIAN_POINT('Ctrl Pts',(-2.21725135110889,1.,3.32218125618955));
#41816=CARTESIAN_POINT('Ctrl Pts',(-2.21115211847872,-1.,3.31764044024231));
#41817=CARTESIAN_POINT('Ctrl Pts',(-2.21115211847872,1.,3.31764044024231));
#41818=CARTESIAN_POINT('Ctrl Pts',(-2.20508863150608,-1.,3.3130742460895));
#41819=CARTESIAN_POINT('Ctrl Pts',(-2.20508863150608,1.,3.3130742460895));
#41820=CARTESIAN_POINT('Ctrl Pts',(-2.19906078949924,-1.,3.30848134694596));
#41821=CARTESIAN_POINT('Ctrl Pts',(-2.19906078949924,1.,3.30848134694596));
#41822=CARTESIAN_POINT('Ctrl Pts',(-2.19306710376112,-1.,3.30385816281831));
#41823=CARTESIAN_POINT('Ctrl Pts',(-2.19306710376112,1.,3.30385816281831));
#41824=CARTESIAN_POINT('Ctrl Pts',(-2.18710556500325,-1.,3.29920022557635));
#41825=CARTESIAN_POINT('Ctrl Pts',(-2.18710556500325,1.,3.29920022557635));
#41826=CARTESIAN_POINT('Ctrl Pts',(-2.18117455557062,-1.,3.29450361500484));
#41827=CARTESIAN_POINT('Ctrl Pts',(-2.18117455557062,1.,3.29450361500484));
#41828=CARTESIAN_POINT('Ctrl Pts',(-2.17527380048422,-1.,3.28976645712566));
#41829=CARTESIAN_POINT('Ctrl Pts',(-2.17527380048422,1.,3.28976645712566));
#41830=CARTESIAN_POINT('Ctrl Pts',(-2.16940517773459,-1.,3.2849901997973));
#41831=CARTESIAN_POINT('Ctrl Pts',(-2.16940517773459,1.,3.2849901997973));
#41832=CARTESIAN_POINT('Ctrl Pts',(-2.16357391934434,-1.,3.28018150841414));
#41833=CARTESIAN_POINT('Ctrl Pts',(-2.16357391934434,1.,3.28018150841414));
#41834=CARTESIAN_POINT('Ctrl Pts',(-2.15778690038359,-1.,3.27534954469206));
#41835=CARTESIAN_POINT('Ctrl Pts',(-2.15778690038359,1.,3.27534954469206));
#41836=CARTESIAN_POINT('Ctrl Pts',(-2.15205043199818,-1.,3.27050245897244));
#41837=CARTESIAN_POINT('Ctrl Pts',(-2.15205043199818,1.,3.27050245897244));
#41838=CARTESIAN_POINT('Ctrl Pts',(-2.14636805295663,-1.,3.26564388189764));
#41839=CARTESIAN_POINT('Ctrl Pts',(-2.14636805295663,1.,3.26564388189764));
#41840=CARTESIAN_POINT('Ctrl Pts',(-2.14073870754257,-1.,3.26077002641868));
#41841=CARTESIAN_POINT('Ctrl Pts',(-2.14073870754257,1.,3.26077002641868));
#41842=CARTESIAN_POINT('Ctrl Pts',(-2.13515375878786,-1.,3.25586495065027));
#41843=CARTESIAN_POINT('Ctrl Pts',(-2.13515375878786,1.,3.25586495065027));
#41844=CARTESIAN_POINT('Ctrl Pts',(-2.1296002839681,-1.,3.25090574493994));
#41845=CARTESIAN_POINT('Ctrl Pts',(-2.1296002839681,1.,3.25090574493994));
#41846=CARTESIAN_POINT('Ctrl Pts',(-2.12406646410943,-1.,3.24587102613347));
#41847=CARTESIAN_POINT('Ctrl Pts',(-2.12406646410943,1.,3.24587102613347));
#41848=CARTESIAN_POINT('Ctrl Pts',(-2.11854673326972,-1.,3.24074905517282));
#41849=CARTESIAN_POINT('Ctrl Pts',(-2.11854673326972,1.,3.24074905517282));
#41850=CARTESIAN_POINT('Ctrl Pts',(-2.11304604021784,-1.,3.23554444767115));
#41851=CARTESIAN_POINT('Ctrl Pts',(-2.11304604021784,1.,3.23554444767115));
#41852=CARTESIAN_POINT('Ctrl Pts',(-2.1075869964248,-1.,3.23028945793334));
#41853=CARTESIAN_POINT('Ctrl Pts',(-2.1075869964248,1.,3.23028945793334));
#41854=CARTESIAN_POINT('Ctrl Pts',(-2.10220384298533,-1.,3.22503437553496));
#41855=CARTESIAN_POINT('Ctrl Pts',(-2.10220384298533,1.,3.22503437553496));
#41856=CARTESIAN_POINT('Ctrl Pts',(-2.09692958434933,-1.,3.21982707347067));
#41857=CARTESIAN_POINT('Ctrl Pts',(-2.09692958434933,1.,3.21982707347067));
#41858=CARTESIAN_POINT('Ctrl Pts',(-2.0917841946046,-1.,3.2146942960168));
#41859=CARTESIAN_POINT('Ctrl Pts',(-2.0917841946046,1.,3.2146942960168));
#41860=CARTESIAN_POINT('Ctrl Pts',(-2.08676465517435,-1.,3.20962575845433));
#41861=CARTESIAN_POINT('Ctrl Pts',(-2.08676465517435,1.,3.20962575845433));
#41862=CARTESIAN_POINT('Ctrl Pts',(-2.08182850370816,-1.,3.20454818630635));
#41863=CARTESIAN_POINT('Ctrl Pts',(-2.08182850370816,1.,3.20454818630635));
#41864=CARTESIAN_POINT('Ctrl Pts',(-2.0769044187063,-1.,3.19934132835879));
#41865=CARTESIAN_POINT('Ctrl Pts',(-2.0769044187063,1.,3.19934132835879));
#41866=CARTESIAN_POINT('Ctrl Pts',(-2.07192253497765,-1.,3.19388465568113));
#41867=CARTESIAN_POINT('Ctrl Pts',(-2.07192253497765,1.,3.19388465568113));
#41868=CARTESIAN_POINT('Ctrl Pts',(-2.06684062744065,-1.,3.18809755562297));
#41869=CARTESIAN_POINT('Ctrl Pts',(-2.06684062744065,1.,3.18809755562297));
#41870=CARTESIAN_POINT('Ctrl Pts',(-2.06166849827143,-1.,3.18197692964677));
#41871=CARTESIAN_POINT('Ctrl Pts',(-2.06166849827143,1.,3.18197692964677));
#41872=CARTESIAN_POINT('Ctrl Pts',(-2.05650186773279,-1.,3.17564906975592));
#41873=CARTESIAN_POINT('Ctrl Pts',(-2.05650186773279,1.,3.17564906975592));
#41874=CARTESIAN_POINT('Ctrl Pts',(-2.05151770247452,-1.,3.16936341689859));
#41875=CARTESIAN_POINT('Ctrl Pts',(-2.05151770247452,1.,3.16936341689859));
#41876=CARTESIAN_POINT('Ctrl Pts',(-2.0469333124766,-1.,3.16343165059235));
#41877=CARTESIAN_POINT('Ctrl Pts',(-2.0469333124766,1.,3.16343165059235));
#41878=CARTESIAN_POINT('Ctrl Pts',(-2.04297406404132,-1.,3.15817983946525));
#41879=CARTESIAN_POINT('Ctrl Pts',(-2.04297406404132,1.,3.15817983946525));
#41880=CARTESIAN_POINT('Ctrl Pts',(-2.03984073791432,-1.,3.1538999167466));
#41881=CARTESIAN_POINT('Ctrl Pts',(-2.03984073791432,1.,3.1538999167466));
#41882=CARTESIAN_POINT('Ctrl Pts',(-2.03766932526171,-1.,3.15079010635326));
#41883=CARTESIAN_POINT('Ctrl Pts',(-2.03766932526171,1.,3.15079010635326));
#41884=CARTESIAN_POINT('Ctrl Pts',(-2.03675273048882,-1.,3.14931281967585));
#41885=CARTESIAN_POINT('Ctrl Pts',(-2.03675273048882,1.,3.14931281967585));
#41886=CARTESIAN_POINT('Ctrl Pts',(-2.03653654935384,-1.,3.14878756590499));
#41887=CARTESIAN_POINT('Ctrl Pts',(-2.03653654935384,1.,3.14878756590499));
#41888=CARTESIAN_POINT('Ctrl Pts',(-2.036601737578,-1.,3.14869618937138));
#41889=CARTESIAN_POINT('Ctrl Pts',(-2.036601737578,1.,3.14869618937138));
#41890=CARTESIAN_POINT('Ctrl Pts',(-2.03668666247593,-1.,3.1487152044751));
#41891=CARTESIAN_POINT('Ctrl Pts',(-2.03668666247593,1.,3.1487152044751));
#41892=CARTESIAN_POINT('',(-2.40675750623143,1.,3.44202241512147));
#41893=CARTESIAN_POINT('Ctrl Pts',(-2.40675750623143,1.,3.44202241512147));
#41894=CARTESIAN_POINT('Ctrl Pts',(-2.40537592959345,1.,3.44127120683402));
#41895=CARTESIAN_POINT('Ctrl Pts',(-2.40261515590099,1.,3.43976627485223));
#41896=CARTESIAN_POINT('Ctrl Pts',(-2.39848113411429,1.,3.43750133066036));
#41897=CARTESIAN_POINT('Ctrl Pts',(-2.39298338805823,1.,3.43446630680436));
#41898=CARTESIAN_POINT('Ctrl Pts',(-2.38613505844641,1.,3.43064732714472));
#41899=CARTESIAN_POINT('Ctrl Pts',(-2.37931067029517,1.,3.42680309755241));
#41900=CARTESIAN_POINT('Ctrl Pts',(-2.37251035954351,1.,3.42293356216595));
#41901=CARTESIAN_POINT('Ctrl Pts',(-2.36573431470314,1.,3.41903866635384));
#41902=CARTESIAN_POINT('Ctrl Pts',(-2.35898278606449,1.,3.4151183675076));
#41903=CARTESIAN_POINT('Ctrl Pts',(-2.35225606823649,1.,3.41117262313464));
#41904=CARTESIAN_POINT('Ctrl Pts',(-2.34555447648901,1.,3.40720137403888));
#41905=CARTESIAN_POINT('Ctrl Pts',(-2.33887832342715,1.,3.40320452776646));
#41906=CARTESIAN_POINT('Ctrl Pts',(-2.33222789882601,1.,3.39918194578115));
#41907=CARTESIAN_POINT('Ctrl Pts',(-2.32560343902683,1.,3.39513342020045));
#41908=CARTESIAN_POINT('Ctrl Pts',(-2.31900513925627,1.,3.39105869475112));
#41909=CARTESIAN_POINT('Ctrl Pts',(-2.31243319489505,1.,3.38695751492659));
#41910=CARTESIAN_POINT('Ctrl Pts',(-2.30588783640389,1.,3.38282967336676));
#41911=CARTESIAN_POINT('Ctrl Pts',(-2.29936936127588,1.,3.37867504959382));
#41912=CARTESIAN_POINT('Ctrl Pts',(-2.2928781800731,1.,3.37449367172707));
#41913=CARTESIAN_POINT('Ctrl Pts',(-2.28641481081045,1.,3.37028570206357));
#41914=CARTESIAN_POINT('Ctrl Pts',(-2.27997979457968,1.,3.36605130712978));
#41915=CARTESIAN_POINT('Ctrl Pts',(-2.27357362620902,1.,3.36179055004369));
#41916=CARTESIAN_POINT('Ctrl Pts',(-2.26719668579921,1.,3.35750328523077));
#41917=CARTESIAN_POINT('Ctrl Pts',(-2.26084915222484,1.,3.35318902552676));
#41918=CARTESIAN_POINT('Ctrl Pts',(-2.25453097693524,1.,3.34884690292342));
#41919=CARTESIAN_POINT('Ctrl Pts',(-2.24824207678288,1.,3.34447596770768));
#41920=CARTESIAN_POINT('Ctrl Pts',(-2.24198249391437,1.,3.34007543738044));
#41921=CARTESIAN_POINT('Ctrl Pts',(-2.2357525632881,1.,3.33564495756478));
#41922=CARTESIAN_POINT('Ctrl Pts',(-2.22955308907221,1.,3.33118487773593));
#41923=CARTESIAN_POINT('Ctrl Pts',(-2.22338548312758,1.,3.32669646722871));
#41924=CARTESIAN_POINT('Ctrl Pts',(-2.21725135110889,1.,3.32218125618955));
#41925=CARTESIAN_POINT('Ctrl Pts',(-2.21115211847872,1.,3.31764044024231));
#41926=CARTESIAN_POINT('Ctrl Pts',(-2.20508863150608,1.,3.3130742460895));
#41927=CARTESIAN_POINT('Ctrl Pts',(-2.19906078949924,1.,3.30848134694596));
#41928=CARTESIAN_POINT('Ctrl Pts',(-2.19306710376112,1.,3.30385816281831));
#41929=CARTESIAN_POINT('Ctrl Pts',(-2.18710556500325,1.,3.29920022557635));
#41930=CARTESIAN_POINT('Ctrl Pts',(-2.18117455557062,1.,3.29450361500484));
#41931=CARTESIAN_POINT('Ctrl Pts',(-2.17527380048422,1.,3.28976645712566));
#41932=CARTESIAN_POINT('Ctrl Pts',(-2.16940517773459,1.,3.2849901997973));
#41933=CARTESIAN_POINT('Ctrl Pts',(-2.16357391934434,1.,3.28018150841414));
#41934=CARTESIAN_POINT('Ctrl Pts',(-2.15778690038359,1.,3.27534954469206));
#41935=CARTESIAN_POINT('Ctrl Pts',(-2.15205043199818,1.,3.27050245897244));
#41936=CARTESIAN_POINT('Ctrl Pts',(-2.14636805295663,1.,3.26564388189764));
#41937=CARTESIAN_POINT('Ctrl Pts',(-2.14073870754257,1.,3.26077002641868));
#41938=CARTESIAN_POINT('Ctrl Pts',(-2.13515375878786,1.,3.25586495065027));
#41939=CARTESIAN_POINT('Ctrl Pts',(-2.1296002839681,1.,3.25090574493994));
#41940=CARTESIAN_POINT('Ctrl Pts',(-2.12406646410943,1.,3.24587102613347));
#41941=CARTESIAN_POINT('Ctrl Pts',(-2.11854673326972,1.,3.24074905517282));
#41942=CARTESIAN_POINT('Ctrl Pts',(-2.11304604021784,1.,3.23554444767115));
#41943=CARTESIAN_POINT('Ctrl Pts',(-2.1075869964248,1.,3.23028945793334));
#41944=CARTESIAN_POINT('Ctrl Pts',(-2.10220384298533,1.,3.22503437553496));
#41945=CARTESIAN_POINT('Ctrl Pts',(-2.09692958434933,1.,3.21982707347067));
#41946=CARTESIAN_POINT('Ctrl Pts',(-2.0917841946046,1.,3.2146942960168));
#41947=CARTESIAN_POINT('Ctrl Pts',(-2.08676465517435,1.,3.20962575845433));
#41948=CARTESIAN_POINT('Ctrl Pts',(-2.08182850370816,1.,3.20454818630635));
#41949=CARTESIAN_POINT('Ctrl Pts',(-2.0769044187063,1.,3.19934132835879));
#41950=CARTESIAN_POINT('Ctrl Pts',(-2.07192253497765,1.,3.19388465568113));
#41951=CARTESIAN_POINT('Ctrl Pts',(-2.06684062744065,1.,3.18809755562297));
#41952=CARTESIAN_POINT('Ctrl Pts',(-2.06166849827143,1.,3.18197692964677));
#41953=CARTESIAN_POINT('Ctrl Pts',(-2.05650186773279,1.,3.17564906975592));
#41954=CARTESIAN_POINT('Ctrl Pts',(-2.05151770247452,1.,3.16936341689859));
#41955=CARTESIAN_POINT('Ctrl Pts',(-2.0469333124766,1.,3.16343165059235));
#41956=CARTESIAN_POINT('Ctrl Pts',(-2.04297406404132,1.,3.15817983946525));
#41957=CARTESIAN_POINT('Ctrl Pts',(-2.03984073791432,1.,3.1538999167466));
#41958=CARTESIAN_POINT('Ctrl Pts',(-2.03783225496023,1.,3.15102344775396));
#41959=CARTESIAN_POINT('Ctrl Pts',(-2.03693188810614,1.,3.14959882629936));
#41960=CARTESIAN_POINT('Ctrl Pts',(-2.03663974554941,1.,3.14901193669147));
#41961=CARTESIAN_POINT('Ctrl Pts',(-2.03659701539175,1.,3.1488193908823));
#41962=CARTESIAN_POINT('Ctrl Pts',(-2.03660101169564,1.,3.14877060440425));
#41963=CARTESIAN_POINT('',(-2.40675750623143,0.,3.44202241512147));
#41964=CARTESIAN_POINT('Ctrl Pts',(-2.36523532225181,-1.,2.91001063062876));
#41965=CARTESIAN_POINT('Ctrl Pts',(-2.36523532225181,1.,2.91001063062876));
#41966=CARTESIAN_POINT('Ctrl Pts',(-2.36524348105112,-1.,2.90992398626211));
#41967=CARTESIAN_POINT('Ctrl Pts',(-2.36524348105112,1.,2.90992398626211));
#41968=CARTESIAN_POINT('Ctrl Pts',(-2.36535052956938,-1.,2.90989022548032));
#41969=CARTESIAN_POINT('Ctrl Pts',(-2.36535052956938,1.,2.90989022548032));
#41970=CARTESIAN_POINT('Ctrl Pts',(-2.36578327194741,-1.,2.91025813830041));
#41971=CARTESIAN_POINT('Ctrl Pts',(-2.36578327194741,1.,2.91025813830041));
#41972=CARTESIAN_POINT('Ctrl Pts',(-2.36690501170627,-1.,2.9115863784204));
#41973=CARTESIAN_POINT('Ctrl Pts',(-2.36690501170627,1.,2.9115863784204));
#41974=CARTESIAN_POINT('Ctrl Pts',(-2.36919161373173,-1.,2.9146124988314));
#41975=CARTESIAN_POINT('Ctrl Pts',(-2.36919161373173,1.,2.9146124988314));
#41976=CARTESIAN_POINT('Ctrl Pts',(-2.37229381109821,-1.,2.91891503791411));
#41977=CARTESIAN_POINT('Ctrl Pts',(-2.37229381109821,1.,2.91891503791411));
#41978=CARTESIAN_POINT('Ctrl Pts',(-2.3760651052403,-1.,2.92430340582608));
#41979=CARTESIAN_POINT('Ctrl Pts',(-2.3760651052403,1.,2.92430340582608));
#41980=CARTESIAN_POINT('Ctrl Pts',(-2.38028989582073,-1.,2.93049643640206));
#41981=CARTESIAN_POINT('Ctrl Pts',(-2.38028989582073,1.,2.93049643640206));
#41982=CARTESIAN_POINT('Ctrl Pts',(-2.38472771516311,-1.,2.93717903280391));
#41983=CARTESIAN_POINT('Ctrl Pts',(-2.38472771516311,1.,2.93717903280391));
#41984=CARTESIAN_POINT('Ctrl Pts',(-2.38914929090759,-1.,2.94404820669076));
#41985=CARTESIAN_POINT('Ctrl Pts',(-2.38914929090759,1.,2.94404820669076));
#41986=CARTESIAN_POINT('Ctrl Pts',(-2.39337207631667,-1.,2.95085857128439));
#41987=CARTESIAN_POINT('Ctrl Pts',(-2.39337207631667,1.,2.95085857128439));
#41988=CARTESIAN_POINT('Ctrl Pts',(-2.39730553974517,-1.,2.95748006482942));
#41989=CARTESIAN_POINT('Ctrl Pts',(-2.39730553974517,1.,2.95748006482942));
#41990=CARTESIAN_POINT('Ctrl Pts',(-2.4009556571164,-1.,2.96390432240312));
#41991=CARTESIAN_POINT('Ctrl Pts',(-2.4009556571164,1.,2.96390432240312));
#41992=CARTESIAN_POINT('Ctrl Pts',(-2.40438604734919,-1.,2.9701964131236));
#41993=CARTESIAN_POINT('Ctrl Pts',(-2.40438604734919,1.,2.9701964131236));
#41994=CARTESIAN_POINT('Ctrl Pts',(-2.40768975073713,-1.,2.97646002822422));
#41995=CARTESIAN_POINT('Ctrl Pts',(-2.40768975073713,1.,2.97646002822422));
#41996=CARTESIAN_POINT('Ctrl Pts',(-2.41095909342571,-1.,2.98280015815107));
#41997=CARTESIAN_POINT('Ctrl Pts',(-2.41095909342571,1.,2.98280015815107));
#41998=CARTESIAN_POINT('Ctrl Pts',(-2.41425064199586,-1.,2.98927983005796));
#41999=CARTESIAN_POINT('Ctrl Pts',(-2.41425064199586,1.,2.98927983005796));
#42000=CARTESIAN_POINT('Ctrl Pts',(-2.41757324500514,-1.,2.99590509293503));
#42001=CARTESIAN_POINT('Ctrl Pts',(-2.41757324500514,1.,2.99590509293503));
#42002=CARTESIAN_POINT('Ctrl Pts',(-2.42090763946779,-1.,3.00264868585996));
#42003=CARTESIAN_POINT('Ctrl Pts',(-2.42090763946779,1.,3.00264868585996));
#42004=CARTESIAN_POINT('Ctrl Pts',(-2.42421849439613,-1.,3.00946442616658));
#42005=CARTESIAN_POINT('Ctrl Pts',(-2.42421849439613,1.,3.00946442616658));
#42006=CARTESIAN_POINT('Ctrl Pts',(-2.42746856264168,-1.,3.01630420830504));
#42007=CARTESIAN_POINT('Ctrl Pts',(-2.42746856264168,1.,3.01630420830504));
#42008=CARTESIAN_POINT('Ctrl Pts',(-2.43063415586637,-1.,3.02313656036004));
#42009=CARTESIAN_POINT('Ctrl Pts',(-2.43063415586637,1.,3.02313656036004));
#42010=CARTESIAN_POINT('Ctrl Pts',(-2.43371241361488,-1.,3.02995534946978));
#42011=CARTESIAN_POINT('Ctrl Pts',(-2.43371241361488,1.,3.02995534946978));
#42012=CARTESIAN_POINT('Ctrl Pts',(-2.43671278042414,-1.,3.03676949672821));
#42013=CARTESIAN_POINT('Ctrl Pts',(-2.43671278042414,1.,3.03676949672821));
#42014=CARTESIAN_POINT('Ctrl Pts',(-2.43965194061857,-1.,3.04359685040555));
#42015=CARTESIAN_POINT('Ctrl Pts',(-2.43965194061857,1.,3.04359685040555));
#42016=CARTESIAN_POINT('Ctrl Pts',(-2.44254768923105,-1.,3.05045678021504));
#42017=CARTESIAN_POINT('Ctrl Pts',(-2.44254768923105,1.,3.05045678021504));
#42018=CARTESIAN_POINT('Ctrl Pts',(-2.44541251892556,-1.,3.05736242671506));
#42019=CARTESIAN_POINT('Ctrl Pts',(-2.44541251892556,1.,3.05736242671506));
#42020=CARTESIAN_POINT('Ctrl Pts',(-2.44824970516544,-1.,3.06431596421405));
#42021=CARTESIAN_POINT('Ctrl Pts',(-2.44824970516544,1.,3.06431596421405));
#42022=CARTESIAN_POINT('Ctrl Pts',(-2.45105688854422,-1.,3.07131290521297));
#42023=CARTESIAN_POINT('Ctrl Pts',(-2.45105688854422,1.,3.07131290521297));
#42024=CARTESIAN_POINT('Ctrl Pts',(-2.4538282678779,-1.,3.07834472886139));
#42025=CARTESIAN_POINT('Ctrl Pts',(-2.4538282678779,1.,3.07834472886139));
#42026=CARTESIAN_POINT('Ctrl Pts',(-2.45655725437039,-1.,3.08540206545315));
#42027=CARTESIAN_POINT('Ctrl Pts',(-2.45655725437039,1.,3.08540206545315));
#42028=CARTESIAN_POINT('Ctrl Pts',(-2.4592391256388,-1.,3.09247787931887));
#42029=CARTESIAN_POINT('Ctrl Pts',(-2.4592391256388,1.,3.09247787931887));
#42030=CARTESIAN_POINT('Ctrl Pts',(-2.46187308501884,-1.,3.09956993697052));
#42031=CARTESIAN_POINT('Ctrl Pts',(-2.46187308501884,1.,3.09956993697052));
#42032=CARTESIAN_POINT('Ctrl Pts',(-2.46446082979646,-1.,3.1066790790198));
#42033=CARTESIAN_POINT('Ctrl Pts',(-2.46446082979646,1.,3.1066790790198));
#42034=CARTESIAN_POINT('Ctrl Pts',(-2.46700558843506,-1.,3.11380805536122));
#42035=CARTESIAN_POINT('Ctrl Pts',(-2.46700558843506,1.,3.11380805536122));
#42036=CARTESIAN_POINT('Ctrl Pts',(-2.46951098947469,-1.,3.12096015766983));
#42037=CARTESIAN_POINT('Ctrl Pts',(-2.46951098947469,1.,3.12096015766983));
#42038=CARTESIAN_POINT('Ctrl Pts',(-2.47197997765871,-1.,3.12813790805952));
#42039=CARTESIAN_POINT('Ctrl Pts',(-2.47197997765871,1.,3.12813790805952));
#42040=CARTESIAN_POINT('Ctrl Pts',(-2.47441378371932,-1.,3.13534181229295));
#42041=CARTESIAN_POINT('Ctrl Pts',(-2.47441378371932,1.,3.13534181229295));
#42042=CARTESIAN_POINT('Ctrl Pts',(-2.47681245356109,-1.,3.1425709954655));
#42043=CARTESIAN_POINT('Ctrl Pts',(-2.47681245356109,1.,3.1425709954655));
#42044=CARTESIAN_POINT('Ctrl Pts',(-2.47917529057029,-1.,3.14982373241352));
#42045=CARTESIAN_POINT('Ctrl Pts',(-2.47917529057029,1.,3.14982373241352));
#42046=CARTESIAN_POINT('Ctrl Pts',(-2.48150133566571,-1.,3.15709802322739));
#42047=CARTESIAN_POINT('Ctrl Pts',(-2.48150133566571,1.,3.15709802322739));
#42048=CARTESIAN_POINT('Ctrl Pts',(-2.48378981792725,-1.,3.16439213290161));
#42049=CARTESIAN_POINT('Ctrl Pts',(-2.48378981792725,1.,3.16439213290161));
#42050=CARTESIAN_POINT('Ctrl Pts',(-2.48604065348587,-1.,3.17170518863313));
#42051=CARTESIAN_POINT('Ctrl Pts',(-2.48604065348587,1.,3.17170518863313));
#42052=CARTESIAN_POINT('Ctrl Pts',(-2.48825428288201,-1.,3.17903698136622));
#42053=CARTESIAN_POINT('Ctrl Pts',(-2.48825428288201,1.,3.17903698136622));
#42054=CARTESIAN_POINT('Ctrl Pts',(-2.49043146334059,-1.,3.18638771282266));
#42055=CARTESIAN_POINT('Ctrl Pts',(-2.49043146334059,1.,3.18638771282266));
#42056=CARTESIAN_POINT('Ctrl Pts',(-2.49257307239848,-1.,3.19375775555798));
#42057=CARTESIAN_POINT('Ctrl Pts',(-2.49257307239848,1.,3.19375775555798));
#42058=CARTESIAN_POINT('Ctrl Pts',(-2.49467992057755,-1.,3.20114742397588));
#42059=CARTESIAN_POINT('Ctrl Pts',(-2.49467992057755,1.,3.20114742397588));
#42060=CARTESIAN_POINT('Ctrl Pts',(-2.4967525264737,-1.,3.20855669849836));
#42061=CARTESIAN_POINT('Ctrl Pts',(-2.4967525264737,1.,3.20855669849836));
#42062=CARTESIAN_POINT('Ctrl Pts',(-2.4987911459939,-1.,3.21598526261286));
#42063=CARTESIAN_POINT('Ctrl Pts',(-2.4987911459939,1.,3.21598526261286));
#42064=CARTESIAN_POINT('Ctrl Pts',(-2.50079587201957,-1.,3.22343262620503));
#42065=CARTESIAN_POINT('Ctrl Pts',(-2.50079587201957,1.,3.22343262620503));
#42066=CARTESIAN_POINT('Ctrl Pts',(-2.50276671338111,-1.,3.23089822320646));
#42067=CARTESIAN_POINT('Ctrl Pts',(-2.50276671338111,1.,3.23089822320646));
#42068=CARTESIAN_POINT('Ctrl Pts',(-2.5047036758003,-1.,3.23838151080319));
#42069=CARTESIAN_POINT('Ctrl Pts',(-2.5047036758003,1.,3.23838151080319));
#42070=CARTESIAN_POINT('Ctrl Pts',(-2.506606859405,-1.,3.24588208983849));
#42071=CARTESIAN_POINT('Ctrl Pts',(-2.506606859405,1.,3.24588208983849));
#42072=CARTESIAN_POINT('Ctrl Pts',(-2.50847647070723,-1.,3.25339971460982));
#42073=CARTESIAN_POINT('Ctrl Pts',(-2.50847647070723,1.,3.25339971460982));
#42074=CARTESIAN_POINT('Ctrl Pts',(-2.51031277813486,-1.,3.26093423001434));
#42075=CARTESIAN_POINT('Ctrl Pts',(-2.51031277813486,1.,3.26093423001434));
#42076=CARTESIAN_POINT('Ctrl Pts',(-2.51211608411423,-1.,3.26848552888115));
#42077=CARTESIAN_POINT('Ctrl Pts',(-2.51211608411423,1.,3.26848552888115));
#42078=CARTESIAN_POINT('Ctrl Pts',(-2.513886692704,-1.,3.27605350473142));
#42079=CARTESIAN_POINT('Ctrl Pts',(-2.513886692704,1.,3.27605350473142));
#42080=CARTESIAN_POINT('Ctrl Pts',(-2.51562487464514,-1.,3.28363799702982));
#42081=CARTESIAN_POINT('Ctrl Pts',(-2.51562487464514,1.,3.28363799702982));
#42082=CARTESIAN_POINT('Ctrl Pts',(-2.51733085123797,-1.,3.2912387729927));
#42083=CARTESIAN_POINT('Ctrl Pts',(-2.51733085123797,1.,3.2912387729927));
#42084=CARTESIAN_POINT('Ctrl Pts',(-2.51900480701069,-1.,3.29885556388352));
#42085=CARTESIAN_POINT('Ctrl Pts',(-2.51900480701069,1.,3.29885556388352));
#42086=CARTESIAN_POINT('Ctrl Pts',(-2.52064689568511,-1.,3.30648808815442));
#42087=CARTESIAN_POINT('Ctrl Pts',(-2.52064689568511,1.,3.30648808815442));
#42088=CARTESIAN_POINT('Ctrl Pts',(-2.52225724871313,-1.,3.31413607874645));
#42089=CARTESIAN_POINT('Ctrl Pts',(-2.52225724871313,1.,3.31413607874645));
#42090=CARTESIAN_POINT('Ctrl Pts',(-2.5238359839626,-1.,3.32179931078699));
#42091=CARTESIAN_POINT('Ctrl Pts',(-2.5238359839626,1.,3.32179931078699));
#42092=CARTESIAN_POINT('Ctrl Pts',(-2.52538321164634,-1.,3.32947762187533));
#42093=CARTESIAN_POINT('Ctrl Pts',(-2.52538321164634,1.,3.32947762187533));
#42094=CARTESIAN_POINT('Ctrl Pts',(-2.52689902690158,-1.,3.33717089999103));
#42095=CARTESIAN_POINT('Ctrl Pts',(-2.52689902690158,1.,3.33717089999103));
#42096=CARTESIAN_POINT('Ctrl Pts',(-2.52808660915689,-1.,3.34333744115511));
#42097=CARTESIAN_POINT('Ctrl Pts',(-2.52808660915689,1.,3.34333744115511));
#42098=CARTESIAN_POINT('Ctrl Pts',(-2.52896321610703,-1.,3.34796903576663));
#42099=CARTESIAN_POINT('Ctrl Pts',(-2.52896321610703,1.,3.34796903576663));
#42100=CARTESIAN_POINT('Ctrl Pts',(-2.5295413654909,-1.,3.35105973714071));
#42101=CARTESIAN_POINT('Ctrl Pts',(-2.5295413654909,1.,3.35105973714071));
#42102=CARTESIAN_POINT('Ctrl Pts',(-2.52982887637028,-1.,3.35260583073571));
#42103=CARTESIAN_POINT('Ctrl Pts',(-2.52982887637028,1.,3.35260583073571));
#42104=CARTESIAN_POINT('',(-2.36531447826073,1.,2.90994629141676));
#42105=CARTESIAN_POINT('Ctrl Pts',(-2.36531447826073,-1.,2.90994629141676));
#42106=CARTESIAN_POINT('Ctrl Pts',(-2.36531447826073,-0.666666666666667,
2.90994629141676));
#42107=CARTESIAN_POINT('Ctrl Pts',(-2.36531447826073,-0.333333333333333,
2.90994629141676));
#42108=CARTESIAN_POINT('Ctrl Pts',(-2.36531447826073,0.333333333333333,
2.90994629141676));
#42109=CARTESIAN_POINT('Ctrl Pts',(-2.36531447826073,0.666666666666667,
2.90994629141676));
#42110=CARTESIAN_POINT('Ctrl Pts',(-2.36531447826073,1.,2.90994629141676));
#42111=CARTESIAN_POINT('',(-2.52982887637028,1.,3.35260583073571));
#42112=CARTESIAN_POINT('',(-2.52982887637028,0.,3.35260583073571));
#42113=CARTESIAN_POINT('Ctrl Pts',(-2.36531447826073,1.,2.90994629141676));
#42114=CARTESIAN_POINT('Ctrl Pts',(-2.36536211188453,1.,2.90995756655606));
#42115=CARTESIAN_POINT('Ctrl Pts',(-2.36553202948613,1.,2.91005770527719));
#42116=CARTESIAN_POINT('Ctrl Pts',(-2.36599991765749,1.,2.91051690822156));
#42117=CARTESIAN_POINT('Ctrl Pts',(-2.36707658451664,1.,2.91181344022549));
#42118=CARTESIAN_POINT('Ctrl Pts',(-2.36919161373173,1.,2.9146124988314));
#42119=CARTESIAN_POINT('Ctrl Pts',(-2.37229381109821,1.,2.91891503791411));
#42120=CARTESIAN_POINT('Ctrl Pts',(-2.3760651052403,1.,2.92430340582608));
#42121=CARTESIAN_POINT('Ctrl Pts',(-2.38028989582073,1.,2.93049643640206));
#42122=CARTESIAN_POINT('Ctrl Pts',(-2.38472771516311,1.,2.93717903280391));
#42123=CARTESIAN_POINT('Ctrl Pts',(-2.38914929090759,1.,2.94404820669076));
#42124=CARTESIAN_POINT('Ctrl Pts',(-2.39337207631667,1.,2.95085857128439));
#42125=CARTESIAN_POINT('Ctrl Pts',(-2.39730553974517,1.,2.95748006482942));
#42126=CARTESIAN_POINT('Ctrl Pts',(-2.4009556571164,1.,2.96390432240312));
#42127=CARTESIAN_POINT('Ctrl Pts',(-2.40438604734919,1.,2.9701964131236));
#42128=CARTESIAN_POINT('Ctrl Pts',(-2.40768975073713,1.,2.97646002822422));
#42129=CARTESIAN_POINT('Ctrl Pts',(-2.41095909342571,1.,2.98280015815107));
#42130=CARTESIAN_POINT('Ctrl Pts',(-2.41425064199586,1.,2.98927983005796));
#42131=CARTESIAN_POINT('Ctrl Pts',(-2.41757324500514,1.,2.99590509293503));
#42132=CARTESIAN_POINT('Ctrl Pts',(-2.42090763946779,1.,3.00264868585996));
#42133=CARTESIAN_POINT('Ctrl Pts',(-2.42421849439613,1.,3.00946442616658));
#42134=CARTESIAN_POINT('Ctrl Pts',(-2.42746856264168,1.,3.01630420830504));
#42135=CARTESIAN_POINT('Ctrl Pts',(-2.43063415586637,1.,3.02313656036004));
#42136=CARTESIAN_POINT('Ctrl Pts',(-2.43371241361488,1.,3.02995534946978));
#42137=CARTESIAN_POINT('Ctrl Pts',(-2.43671278042414,1.,3.03676949672821));
#42138=CARTESIAN_POINT('Ctrl Pts',(-2.43965194061857,1.,3.04359685040555));
#42139=CARTESIAN_POINT('Ctrl Pts',(-2.44254768923105,1.,3.05045678021504));
#42140=CARTESIAN_POINT('Ctrl Pts',(-2.44541251892556,1.,3.05736242671506));
#42141=CARTESIAN_POINT('Ctrl Pts',(-2.44824970516544,1.,3.06431596421405));
#42142=CARTESIAN_POINT('Ctrl Pts',(-2.45105688854422,1.,3.07131290521297));
#42143=CARTESIAN_POINT('Ctrl Pts',(-2.4538282678779,1.,3.07834472886139));
#42144=CARTESIAN_POINT('Ctrl Pts',(-2.45655725437039,1.,3.08540206545315));
#42145=CARTESIAN_POINT('Ctrl Pts',(-2.4592391256388,1.,3.09247787931887));
#42146=CARTESIAN_POINT('Ctrl Pts',(-2.46187308501884,1.,3.09956993697052));
#42147=CARTESIAN_POINT('Ctrl Pts',(-2.46446082979646,1.,3.1066790790198));
#42148=CARTESIAN_POINT('Ctrl Pts',(-2.46700558843506,1.,3.11380805536122));
#42149=CARTESIAN_POINT('Ctrl Pts',(-2.46951098947469,1.,3.12096015766983));
#42150=CARTESIAN_POINT('Ctrl Pts',(-2.47197997765871,1.,3.12813790805952));
#42151=CARTESIAN_POINT('Ctrl Pts',(-2.47441378371932,1.,3.13534181229295));
#42152=CARTESIAN_POINT('Ctrl Pts',(-2.47681245356109,1.,3.1425709954655));
#42153=CARTESIAN_POINT('Ctrl Pts',(-2.47917529057029,1.,3.14982373241352));
#42154=CARTESIAN_POINT('Ctrl Pts',(-2.48150133566571,1.,3.15709802322739));
#42155=CARTESIAN_POINT('Ctrl Pts',(-2.48378981792725,1.,3.16439213290161));
#42156=CARTESIAN_POINT('Ctrl Pts',(-2.48604065348587,1.,3.17170518863313));
#42157=CARTESIAN_POINT('Ctrl Pts',(-2.48825428288201,1.,3.17903698136622));
#42158=CARTESIAN_POINT('Ctrl Pts',(-2.49043146334059,1.,3.18638771282266));
#42159=CARTESIAN_POINT('Ctrl Pts',(-2.49257307239848,1.,3.19375775555798));
#42160=CARTESIAN_POINT('Ctrl Pts',(-2.49467992057755,1.,3.20114742397588));
#42161=CARTESIAN_POINT('Ctrl Pts',(-2.4967525264737,1.,3.20855669849836));
#42162=CARTESIAN_POINT('Ctrl Pts',(-2.4987911459939,1.,3.21598526261286));
#42163=CARTESIAN_POINT('Ctrl Pts',(-2.50079587201957,1.,3.22343262620503));
#42164=CARTESIAN_POINT('Ctrl Pts',(-2.50276671338111,1.,3.23089822320646));
#42165=CARTESIAN_POINT('Ctrl Pts',(-2.5047036758003,1.,3.23838151080319));
#42166=CARTESIAN_POINT('Ctrl Pts',(-2.506606859405,1.,3.24588208983849));
#42167=CARTESIAN_POINT('Ctrl Pts',(-2.50847647070723,1.,3.25339971460982));
#42168=CARTESIAN_POINT('Ctrl Pts',(-2.51031277813486,1.,3.26093423001434));
#42169=CARTESIAN_POINT('Ctrl Pts',(-2.51211608411423,1.,3.26848552888115));
#42170=CARTESIAN_POINT('Ctrl Pts',(-2.513886692704,1.,3.27605350473142));
#42171=CARTESIAN_POINT('Ctrl Pts',(-2.51562487464514,1.,3.28363799702982));
#42172=CARTESIAN_POINT('Ctrl Pts',(-2.51733085123797,1.,3.2912387729927));
#42173=CARTESIAN_POINT('Ctrl Pts',(-2.51900480701069,1.,3.29885556388352));
#42174=CARTESIAN_POINT('Ctrl Pts',(-2.52064689568511,1.,3.30648808815442));
#42175=CARTESIAN_POINT('Ctrl Pts',(-2.52225724871313,1.,3.31413607874645));
#42176=CARTESIAN_POINT('Ctrl Pts',(-2.5238359839626,1.,3.32179931078699));
#42177=CARTESIAN_POINT('Ctrl Pts',(-2.52538321164634,1.,3.32947762187533));
#42178=CARTESIAN_POINT('Ctrl Pts',(-2.52689902690158,1.,3.33717089999103));
#42179=CARTESIAN_POINT('Ctrl Pts',(-2.52808660915689,1.,3.34333744115511));
#42180=CARTESIAN_POINT('Ctrl Pts',(-2.52896321610703,1.,3.34796903576663));
#42181=CARTESIAN_POINT('Ctrl Pts',(-2.5295413654909,1.,3.35105973714071));
#42182=CARTESIAN_POINT('Ctrl Pts',(-2.52982887637028,1.,3.35260583073571));
#42183=CARTESIAN_POINT('Origin',(-2.52982887637028,0.,3.35260583073571));
#42184=CARTESIAN_POINT('',(-2.40675750623143,1.,3.44202241512147));
#42185=CARTESIAN_POINT('Origin',(0.,0.,0.));
#42186=CARTESIAN_POINT('',(-2.50410331873042,1.,2.79140942341378));
#42187=CARTESIAN_POINT('Origin',(0.,1.,0.));
#42188=CARTESIAN_POINT('Ctrl Pts',(-2.50410331873042,1.,2.79140942341378));
#42189=CARTESIAN_POINT('Ctrl Pts',(-2.50410331873042,0.666666666666667,
2.79140942341378));
#42190=CARTESIAN_POINT('Ctrl Pts',(-2.50410331873043,0.333333333333333,
2.79140942341378));
#42191=CARTESIAN_POINT('Ctrl Pts',(-2.50410331873043,-0.333333333333333,
2.79140942341378));
#42192=CARTESIAN_POINT('Ctrl Pts',(-2.50410331873043,-0.666666666666667,
2.79140942341378));
#42193=CARTESIAN_POINT('Ctrl Pts',(-2.50410331873043,-1.,2.79140942341378));
#42194=CARTESIAN_POINT('Ctrl Pts',(-2.91557726271063,-1.,3.02314558451372));
#42195=CARTESIAN_POINT('Ctrl Pts',(-2.91557726271063,1.,3.02314558451372));
#42196=CARTESIAN_POINT('Ctrl Pts',(-2.91409518070707,-1.,3.02261975104912));
#42197=CARTESIAN_POINT('Ctrl Pts',(-2.91409518070707,1.,3.02261975104912));
#42198=CARTESIAN_POINT('Ctrl Pts',(-2.91113297349052,-1.,3.02156522743299));
#42199=CARTESIAN_POINT('Ctrl Pts',(-2.91113297349052,1.,3.02156522743299));
#42200=CARTESIAN_POINT('Ctrl Pts',(-2.90669553303902,-1.,3.01997487194926));
#42201=CARTESIAN_POINT('Ctrl Pts',(-2.90669553303902,1.,3.01997487194926));
#42202=CARTESIAN_POINT('Ctrl Pts',(-2.90079069102661,-1.,3.01783725123646));
#42203=CARTESIAN_POINT('Ctrl Pts',(-2.90079069102661,1.,3.01783725123646));
#42204=CARTESIAN_POINT('Ctrl Pts',(-2.8934292556764,-1.,3.01513660433291));
#42205=CARTESIAN_POINT('Ctrl Pts',(-2.8934292556764,1.,3.01513660433291));
#42206=CARTESIAN_POINT('Ctrl Pts',(-2.88608751706796,-1.,3.01240727309568));
#42207=CARTESIAN_POINT('Ctrl Pts',(-2.88608751706796,1.,3.01240727309568));
#42208=CARTESIAN_POINT('Ctrl Pts',(-2.87876560072799,-1.,3.0096491810855));
#42209=CARTESIAN_POINT('Ctrl Pts',(-2.87876560072799,1.,3.0096491810855));
#42210=CARTESIAN_POINT('Ctrl Pts',(-2.87146368430104,-1.,3.00686224485374));
#42211=CARTESIAN_POINT('Ctrl Pts',(-2.87146368430104,1.,3.00686224485374));
#42212=CARTESIAN_POINT('Ctrl Pts',(-2.86418200833065,-1.,3.00404638316245));
#42213=CARTESIAN_POINT('Ctrl Pts',(-2.86418200833065,1.,3.00404638316245));
#42214=CARTESIAN_POINT('Ctrl Pts',(-2.85692085715129,-1.,3.0012015079552));
#42215=CARTESIAN_POINT('Ctrl Pts',(-2.85692085715129,1.,3.0012015079552));
#42216=CARTESIAN_POINT('Ctrl Pts',(-2.84968053289104,-1.,2.99832751144566));
#42217=CARTESIAN_POINT('Ctrl Pts',(-2.84968053289104,1.,2.99832751144566));
#42218=CARTESIAN_POINT('Ctrl Pts',(-2.84246132984334,-1.,2.995424253416));
#42219=CARTESIAN_POINT('Ctrl Pts',(-2.84246132984334,1.,2.995424253416));
#42220=CARTESIAN_POINT('Ctrl Pts',(-2.83526351254383,-1.,2.99249155170479));
#42221=CARTESIAN_POINT('Ctrl Pts',(-2.83526351254383,1.,2.99249155170479));
#42222=CARTESIAN_POINT('Ctrl Pts',(-2.82808728190402,-1.,2.98952916401699));
#42223=CARTESIAN_POINT('Ctrl Pts',(-2.82808728190402,1.,2.98952916401699));
#42224=CARTESIAN_POINT('Ctrl Pts',(-2.82093279065704,-1.,2.98653680669434));
#42225=CARTESIAN_POINT('Ctrl Pts',(-2.82093279065704,1.,2.98653680669434));
#42226=CARTESIAN_POINT('Ctrl Pts',(-2.81380019196454,-1.,2.9835141977994));
#42227=CARTESIAN_POINT('Ctrl Pts',(-2.81380019196454,1.,2.9835141977994));
#42228=CARTESIAN_POINT('Ctrl Pts',(-2.80668968101162,-1.,2.98046109647299));
#42229=CARTESIAN_POINT('Ctrl Pts',(-2.80668968101162,1.,2.98046109647299));
#42230=CARTESIAN_POINT('Ctrl Pts',(-2.79960153278186,-1.,2.97737733718242));
#42231=CARTESIAN_POINT('Ctrl Pts',(-2.79960153278186,1.,2.97737733718242));
#42232=CARTESIAN_POINT('Ctrl Pts',(-2.79253615718147,-1.,2.97426288347475));
#42233=CARTESIAN_POINT('Ctrl Pts',(-2.79253615718147,1.,2.97426288347475));
#42234=CARTESIAN_POINT('Ctrl Pts',(-2.78549409123657,-1.,2.97111781461349));
#42235=CARTESIAN_POINT('Ctrl Pts',(-2.78549409123657,1.,2.97111781461349));
#42236=CARTESIAN_POINT('Ctrl Pts',(-2.77847589542767,-1.,2.9679422104295));
#42237=CARTESIAN_POINT('Ctrl Pts',(-2.77847589542767,1.,2.9679422104295));
#42238=CARTESIAN_POINT('Ctrl Pts',(-2.77148206836464,-1.,2.96473605585548));
#42239=CARTESIAN_POINT('Ctrl Pts',(-2.77148206836464,1.,2.96473605585548));
#42240=CARTESIAN_POINT('Ctrl Pts',(-2.76451296269571,-1.,2.96149914764832));
#42241=CARTESIAN_POINT('Ctrl Pts',(-2.76451296269571,1.,2.96149914764832));
#42242=CARTESIAN_POINT('Ctrl Pts',(-2.75756867888393,-1.,2.9582309766594));
#42243=CARTESIAN_POINT('Ctrl Pts',(-2.75756867888393,1.,2.9582309766594));
#42244=CARTESIAN_POINT('Ctrl Pts',(-2.75064903318996,-1.,2.95493069316211));
#42245=CARTESIAN_POINT('Ctrl Pts',(-2.75064903318996,1.,2.95493069316211));
#42246=CARTESIAN_POINT('Ctrl Pts',(-2.7437537949221,-1.,2.95159737214305));
#42247=CARTESIAN_POINT('Ctrl Pts',(-2.7437537949221,1.,2.95159737214305));
#42248=CARTESIAN_POINT('Ctrl Pts',(-2.73688288329825,-1.,2.94823023414381));
#42249=CARTESIAN_POINT('Ctrl Pts',(-2.73688288329825,1.,2.94823023414381));
#42250=CARTESIAN_POINT('Ctrl Pts',(-2.73003657371613,-1.,2.94482887675139));
#42251=CARTESIAN_POINT('Ctrl Pts',(-2.73003657371613,1.,2.94482887675139));
#42252=CARTESIAN_POINT('Ctrl Pts',(-2.72321571511322,-1.,2.94139351933882));
#42253=CARTESIAN_POINT('Ctrl Pts',(-2.72321571511322,1.,2.94139351933882));
#42254=CARTESIAN_POINT('Ctrl Pts',(-2.71642190053575,-1.,2.93792519474955));
#42255=CARTESIAN_POINT('Ctrl Pts',(-2.71642190053575,1.,2.93792519474955));
#42256=CARTESIAN_POINT('Ctrl Pts',(-2.70965695523776,-1.,2.93442516311168));
#42257=CARTESIAN_POINT('Ctrl Pts',(-2.70965695523776,1.,2.93442516311168));
#42258=CARTESIAN_POINT('Ctrl Pts',(-2.70292247416881,-1.,2.93089438233746));
#42259=CARTESIAN_POINT('Ctrl Pts',(-2.70292247416881,1.,2.93089438233746));
#42260=CARTESIAN_POINT('Ctrl Pts',(-2.69621932864302,-1.,2.92733294395268));
#42261=CARTESIAN_POINT('Ctrl Pts',(-2.69621932864302,1.,2.92733294395268));
#42262=CARTESIAN_POINT('Ctrl Pts',(-2.68954721165342,-1.,2.92373955325876));
#42263=CARTESIAN_POINT('Ctrl Pts',(-2.68954721165342,1.,2.92373955325876));
#42264=CARTESIAN_POINT('Ctrl Pts',(-2.68290409279689,-1.,2.92011090722152));
#42265=CARTESIAN_POINT('Ctrl Pts',(-2.68290409279689,1.,2.92011090722152));
#42266=CARTESIAN_POINT('Ctrl Pts',(-2.67628728855309,-1.,2.91644290704281));
#42267=CARTESIAN_POINT('Ctrl Pts',(-2.67628728855309,1.,2.91644290704281));
#42268=CARTESIAN_POINT('Ctrl Pts',(-2.66969458792627,-1.,2.91273193382876));
#42269=CARTESIAN_POINT('Ctrl Pts',(-2.66969458792627,1.,2.91273193382876));
#42270=CARTESIAN_POINT('Ctrl Pts',(-2.66312542616809,-1.,2.90897617968921));
#42271=CARTESIAN_POINT('Ctrl Pts',(-2.66312542616809,1.,2.90897617968921));
#42272=CARTESIAN_POINT('Ctrl Pts',(-2.65658188464287,-1.,2.90517678087467));
#42273=CARTESIAN_POINT('Ctrl Pts',(-2.65658188464287,1.,2.90517678087467));
#42274=CARTESIAN_POINT('Ctrl Pts',(-2.65007017365576,-1.,2.90133950224879));
#42275=CARTESIAN_POINT('Ctrl Pts',(-2.65007017365576,1.,2.90133950224879));
#42276=CARTESIAN_POINT('Ctrl Pts',(-2.64359851684146,-1.,2.89747231723361));
#42277=CARTESIAN_POINT('Ctrl Pts',(-2.64359851684146,1.,2.89747231723361));
#42278=CARTESIAN_POINT('Ctrl Pts',(-2.63717442263944,-1.,2.89358228854557));
#42279=CARTESIAN_POINT('Ctrl Pts',(-2.63717442263944,1.,2.89358228854557));
#42280=CARTESIAN_POINT('Ctrl Pts',(-2.63080195420771,-1.,2.88967244854243));
#42281=CARTESIAN_POINT('Ctrl Pts',(-2.63080195420771,1.,2.88967244854243));
#42282=CARTESIAN_POINT('Ctrl Pts',(-2.62447947640253,-1.,2.88573922195049));
#42283=CARTESIAN_POINT('Ctrl Pts',(-2.62447947640253,1.,2.88573922195049));
#42284=CARTESIAN_POINT('Ctrl Pts',(-2.61819596473087,-1.,2.88176821427502));
#42285=CARTESIAN_POINT('Ctrl Pts',(-2.61819596473087,1.,2.88176821427502));
#42286=CARTESIAN_POINT('Ctrl Pts',(-2.61193507170928,-1.,2.87773881947885));
#42287=CARTESIAN_POINT('Ctrl Pts',(-2.61193507170928,1.,2.87773881947885));
#42288=CARTESIAN_POINT('Ctrl Pts',(-2.6056817788128,-1.,2.87363176656475));
#42289=CARTESIAN_POINT('Ctrl Pts',(-2.6056817788128,1.,2.87363176656475));
#42290=CARTESIAN_POINT('Ctrl Pts',(-2.59942875223202,-1.,2.86943633170712));
#42291=CARTESIAN_POINT('Ctrl Pts',(-2.59942875223202,1.,2.86943633170712));
#42292=CARTESIAN_POINT('Ctrl Pts',(-2.59318160184921,-1.,2.86515629953528));
#42293=CARTESIAN_POINT('Ctrl Pts',(-2.59318160184921,1.,2.86515629953528));
#42294=CARTESIAN_POINT('Ctrl Pts',(-2.5869677064356,-1.,2.86081999003668));
#42295=CARTESIAN_POINT('Ctrl Pts',(-2.5869677064356,1.,2.86081999003668));
#42296=CARTESIAN_POINT('Ctrl Pts',(-2.58082875254407,-1.,2.85647171715147));
#42297=CARTESIAN_POINT('Ctrl Pts',(-2.58082875254407,1.,2.85647171715147));
#42298=CARTESIAN_POINT('Ctrl Pts',(-2.57480482727128,-1.,2.85215360144483));
#42299=CARTESIAN_POINT('Ctrl Pts',(-2.57480482727128,1.,2.85215360144483));
#42300=CARTESIAN_POINT('Ctrl Pts',(-2.56891984251743,-1.,2.84788893329091));
#42301=CARTESIAN_POINT('Ctrl Pts',(-2.56891984251743,1.,2.84788893329091));
#42302=CARTESIAN_POINT('Ctrl Pts',(-2.56316920798489,-1.,2.84366802680211));
#42303=CARTESIAN_POINT('Ctrl Pts',(-2.56316920798489,1.,2.84366802680211));
#42304=CARTESIAN_POINT('Ctrl Pts',(-2.55749952145165,-1.,2.83942515220699));
#42305=CARTESIAN_POINT('Ctrl Pts',(-2.55749952145165,1.,2.83942515220699));
#42306=CARTESIAN_POINT('Ctrl Pts',(-2.55182152806964,-1.,2.83505269592412));
#42307=CARTESIAN_POINT('Ctrl Pts',(-2.55182152806964,1.,2.83505269592412));
#42308=CARTESIAN_POINT('Ctrl Pts',(-2.54604736792542,-1.,2.83044254225794));
#42309=CARTESIAN_POINT('Ctrl Pts',(-2.54604736792542,1.,2.83044254225794));
#42310=CARTESIAN_POINT('Ctrl Pts',(-2.54012272520141,-1.,2.82552167649157));
#42311=CARTESIAN_POINT('Ctrl Pts',(-2.54012272520141,1.,2.82552167649157));
#42312=CARTESIAN_POINT('Ctrl Pts',(-2.53405679667463,-1.,2.82028550483744));
#42313=CARTESIAN_POINT('Ctrl Pts',(-2.53405679667463,1.,2.82028550483744));
#42314=CARTESIAN_POINT('Ctrl Pts',(-2.52796388055457,-1.,2.8148437904867));
#42315=CARTESIAN_POINT('Ctrl Pts',(-2.52796388055457,1.,2.8148437904867));
#42316=CARTESIAN_POINT('Ctrl Pts',(-2.52205778589922,-1.,2.80941521967234));
#42317=CARTESIAN_POINT('Ctrl Pts',(-2.52205778589922,1.,2.80941521967234));
#42318=CARTESIAN_POINT('Ctrl Pts',(-2.51660190466067,-1.,2.80427363984939));
#42319=CARTESIAN_POINT('Ctrl Pts',(-2.51660190466067,1.,2.80427363984939));
#42320=CARTESIAN_POINT('Ctrl Pts',(-2.51186983687947,-1.,2.79970585014308));
#42321=CARTESIAN_POINT('Ctrl Pts',(-2.51186983687947,1.,2.79970585014308));
#42322=CARTESIAN_POINT('Ctrl Pts',(-2.50810555977564,-1.,2.7959687805717));
#42323=CARTESIAN_POINT('Ctrl Pts',(-2.50810555977564,1.,2.7959687805717));
#42324=CARTESIAN_POINT('Ctrl Pts',(-2.50547439929077,-1.,2.79323694088143));
#42325=CARTESIAN_POINT('Ctrl Pts',(-2.50547439929077,1.,2.79323694088143));
#42326=CARTESIAN_POINT('Ctrl Pts',(-2.50433799076945,-1.,2.79192122906739));
#42327=CARTESIAN_POINT('Ctrl Pts',(-2.50433799076945,1.,2.79192122906739));
#42328=CARTESIAN_POINT('Ctrl Pts',(-2.50404230339032,-1.,2.79143626022225));
#42329=CARTESIAN_POINT('Ctrl Pts',(-2.50404230339032,1.,2.79143626022225));
#42330=CARTESIAN_POINT('Ctrl Pts',(-2.50409239460011,-1.,2.79133581100044));
#42331=CARTESIAN_POINT('Ctrl Pts',(-2.50409239460011,1.,2.79133581100044));
#42332=CARTESIAN_POINT('Ctrl Pts',(-2.50417924854921,-1.,2.79134130681569));
#42333=CARTESIAN_POINT('Ctrl Pts',(-2.50417924854921,1.,2.79134130681569));
#42334=CARTESIAN_POINT('',(-2.91557726271063,1.,3.02314558451372));
#42335=CARTESIAN_POINT('Ctrl Pts',(-2.91557726271063,1.,3.02314558451372));
#42336=CARTESIAN_POINT('Ctrl Pts',(-2.91409518070707,1.,3.02261975104912));
#42337=CARTESIAN_POINT('Ctrl Pts',(-2.91113297349052,1.,3.02156522743299));
#42338=CARTESIAN_POINT('Ctrl Pts',(-2.90669553303902,1.,3.01997487194926));
#42339=CARTESIAN_POINT('Ctrl Pts',(-2.90079069102661,1.,3.01783725123646));
#42340=CARTESIAN_POINT('Ctrl Pts',(-2.8934292556764,1.,3.01513660433291));
#42341=CARTESIAN_POINT('Ctrl Pts',(-2.88608751706796,1.,3.01240727309568));
#42342=CARTESIAN_POINT('Ctrl Pts',(-2.87876560072799,1.,3.0096491810855));
#42343=CARTESIAN_POINT('Ctrl Pts',(-2.87146368430104,1.,3.00686224485374));
#42344=CARTESIAN_POINT('Ctrl Pts',(-2.86418200833065,1.,3.00404638316245));
#42345=CARTESIAN_POINT('Ctrl Pts',(-2.85692085715129,1.,3.0012015079552));
#42346=CARTESIAN_POINT('Ctrl Pts',(-2.84968053289104,1.,2.99832751144566));
#42347=CARTESIAN_POINT('Ctrl Pts',(-2.84246132984334,1.,2.995424253416));
#42348=CARTESIAN_POINT('Ctrl Pts',(-2.83526351254383,1.,2.99249155170479));
#42349=CARTESIAN_POINT('Ctrl Pts',(-2.82808728190402,1.,2.98952916401699));
#42350=CARTESIAN_POINT('Ctrl Pts',(-2.82093279065704,1.,2.98653680669434));
#42351=CARTESIAN_POINT('Ctrl Pts',(-2.81380019196454,1.,2.9835141977994));
#42352=CARTESIAN_POINT('Ctrl Pts',(-2.80668968101162,1.,2.98046109647299));
#42353=CARTESIAN_POINT('Ctrl Pts',(-2.79960153278186,1.,2.97737733718242));
#42354=CARTESIAN_POINT('Ctrl Pts',(-2.79253615718147,1.,2.97426288347475));
#42355=CARTESIAN_POINT('Ctrl Pts',(-2.78549409123657,1.,2.97111781461349));
#42356=CARTESIAN_POINT('Ctrl Pts',(-2.77847589542767,1.,2.9679422104295));
#42357=CARTESIAN_POINT('Ctrl Pts',(-2.77148206836464,1.,2.96473605585548));
#42358=CARTESIAN_POINT('Ctrl Pts',(-2.76451296269571,1.,2.96149914764832));
#42359=CARTESIAN_POINT('Ctrl Pts',(-2.75756867888393,1.,2.9582309766594));
#42360=CARTESIAN_POINT('Ctrl Pts',(-2.75064903318996,1.,2.95493069316211));
#42361=CARTESIAN_POINT('Ctrl Pts',(-2.7437537949221,1.,2.95159737214305));
#42362=CARTESIAN_POINT('Ctrl Pts',(-2.73688288329825,1.,2.94823023414381));
#42363=CARTESIAN_POINT('Ctrl Pts',(-2.73003657371613,1.,2.94482887675139));
#42364=CARTESIAN_POINT('Ctrl Pts',(-2.72321571511322,1.,2.94139351933882));
#42365=CARTESIAN_POINT('Ctrl Pts',(-2.71642190053575,1.,2.93792519474955));
#42366=CARTESIAN_POINT('Ctrl Pts',(-2.70965695523776,1.,2.93442516311168));
#42367=CARTESIAN_POINT('Ctrl Pts',(-2.70292247416881,1.,2.93089438233746));
#42368=CARTESIAN_POINT('Ctrl Pts',(-2.69621932864302,1.,2.92733294395268));
#42369=CARTESIAN_POINT('Ctrl Pts',(-2.68954721165342,1.,2.92373955325876));
#42370=CARTESIAN_POINT('Ctrl Pts',(-2.68290409279689,1.,2.92011090722152));
#42371=CARTESIAN_POINT('Ctrl Pts',(-2.67628728855309,1.,2.91644290704281));
#42372=CARTESIAN_POINT('Ctrl Pts',(-2.66969458792627,1.,2.91273193382876));
#42373=CARTESIAN_POINT('Ctrl Pts',(-2.66312542616809,1.,2.90897617968921));
#42374=CARTESIAN_POINT('Ctrl Pts',(-2.65658188464287,1.,2.90517678087467));
#42375=CARTESIAN_POINT('Ctrl Pts',(-2.65007017365576,1.,2.90133950224879));
#42376=CARTESIAN_POINT('Ctrl Pts',(-2.64359851684146,1.,2.89747231723361));
#42377=CARTESIAN_POINT('Ctrl Pts',(-2.63717442263944,1.,2.89358228854557));
#42378=CARTESIAN_POINT('Ctrl Pts',(-2.63080195420771,1.,2.88967244854243));
#42379=CARTESIAN_POINT('Ctrl Pts',(-2.62447947640253,1.,2.88573922195049));
#42380=CARTESIAN_POINT('Ctrl Pts',(-2.61819596473087,1.,2.88176821427502));
#42381=CARTESIAN_POINT('Ctrl Pts',(-2.61193507170928,1.,2.87773881947885));
#42382=CARTESIAN_POINT('Ctrl Pts',(-2.6056817788128,1.,2.87363176656475));
#42383=CARTESIAN_POINT('Ctrl Pts',(-2.59942875223202,1.,2.86943633170712));
#42384=CARTESIAN_POINT('Ctrl Pts',(-2.59318160184921,1.,2.86515629953528));
#42385=CARTESIAN_POINT('Ctrl Pts',(-2.5869677064356,1.,2.86081999003668));
#42386=CARTESIAN_POINT('Ctrl Pts',(-2.58082875254407,1.,2.85647171715147));
#42387=CARTESIAN_POINT('Ctrl Pts',(-2.57480482727128,1.,2.85215360144483));
#42388=CARTESIAN_POINT('Ctrl Pts',(-2.56891984251743,1.,2.84788893329091));
#42389=CARTESIAN_POINT('Ctrl Pts',(-2.56316920798489,1.,2.84366802680211));
#42390=CARTESIAN_POINT('Ctrl Pts',(-2.55749952145165,1.,2.83942515220699));
#42391=CARTESIAN_POINT('Ctrl Pts',(-2.55182152806964,1.,2.83505269592412));
#42392=CARTESIAN_POINT('Ctrl Pts',(-2.54604736792542,1.,2.83044254225794));
#42393=CARTESIAN_POINT('Ctrl Pts',(-2.54012272520141,1.,2.82552167649157));
#42394=CARTESIAN_POINT('Ctrl Pts',(-2.53405679667463,1.,2.82028550483744));
#42395=CARTESIAN_POINT('Ctrl Pts',(-2.52796388055457,1.,2.8148437904867));
#42396=CARTESIAN_POINT('Ctrl Pts',(-2.52205778589922,1.,2.80941521967234));
#42397=CARTESIAN_POINT('Ctrl Pts',(-2.51660190466067,1.,2.80427363984939));
#42398=CARTESIAN_POINT('Ctrl Pts',(-2.51186983687947,1.,2.79970585014308));
#42399=CARTESIAN_POINT('Ctrl Pts',(-2.50810555977564,1.,2.7959687805717));
#42400=CARTESIAN_POINT('Ctrl Pts',(-2.50567182569153,1.,2.79344192164204));
#42401=CARTESIAN_POINT('Ctrl Pts',(-2.50455968395235,1.,2.79217568804874));
#42402=CARTESIAN_POINT('Ctrl Pts',(-2.50417932839343,1.,2.79164172519039));
#42403=CARTESIAN_POINT('Ctrl Pts',(-2.50410700351427,1.,2.79145823440899));
#42404=CARTESIAN_POINT('Ctrl Pts',(-2.50410331873043,1.,2.79140942341378));
#42405=CARTESIAN_POINT('',(-2.91557726271063,0.,3.02314558451372));
#42406=CARTESIAN_POINT('Ctrl Pts',(-2.79134130681569,-1.,2.50417924854921));
#42407=CARTESIAN_POINT('Ctrl Pts',(-2.79134130681569,1.,2.50417924854921));
#42408=CARTESIAN_POINT('Ctrl Pts',(-2.7913358110015,-1.,2.50409239460108));
#42409=CARTESIAN_POINT('Ctrl Pts',(-2.7913358110015,1.,2.50409239460108));
#42410=CARTESIAN_POINT('Ctrl Pts',(-2.79143626022503,-1.,2.50404230339286));
#42411=CARTESIAN_POINT('Ctrl Pts',(-2.79143626022503,1.,2.50404230339286));
#42412=CARTESIAN_POINT('Ctrl Pts',(-2.79192122907148,-1.,2.5043379907732));
#42413=CARTESIAN_POINT('Ctrl Pts',(-2.79192122907148,1.,2.5043379907732));
#42414=CARTESIAN_POINT('Ctrl Pts',(-2.7932369408851,-1.,2.50547439929414));
#42415=CARTESIAN_POINT('Ctrl Pts',(-2.7932369408851,1.,2.50547439929414));
#42416=CARTESIAN_POINT('Ctrl Pts',(-2.79596878057287,-1.,2.50810555977671));
#42417=CARTESIAN_POINT('Ctrl Pts',(-2.79596878057287,1.,2.50810555977671));
#42418=CARTESIAN_POINT('Ctrl Pts',(-2.79970585014168,-1.,2.51186983687818));
#42419=CARTESIAN_POINT('Ctrl Pts',(-2.79970585014168,1.,2.51186983687818));
#42420=CARTESIAN_POINT('Ctrl Pts',(-2.80427363984653,-1.,2.51660190465805));
#42421=CARTESIAN_POINT('Ctrl Pts',(-2.80427363984653,1.,2.51660190465805));
#42422=CARTESIAN_POINT('Ctrl Pts',(-2.80941521966941,-1.,2.52205778589653));
#42423=CARTESIAN_POINT('Ctrl Pts',(-2.80941521966941,1.,2.52205778589653));
#42424=CARTESIAN_POINT('Ctrl Pts',(-2.81484379048475,-1.,2.52796388055278));
#42425=CARTESIAN_POINT('Ctrl Pts',(-2.81484379048475,1.,2.52796388055278));
#42426=CARTESIAN_POINT('Ctrl Pts',(-2.82028550483689,-1.,2.53405679667412));
#42427=CARTESIAN_POINT('Ctrl Pts',(-2.82028550483689,1.,2.53405679667412));
#42428=CARTESIAN_POINT('Ctrl Pts',(-2.8255216764922,-1.,2.54012272520199));
#42429=CARTESIAN_POINT('Ctrl Pts',(-2.8255216764922,1.,2.54012272520199));
#42430=CARTESIAN_POINT('Ctrl Pts',(-2.83044254225917,-1.,2.54604736792655));
#42431=CARTESIAN_POINT('Ctrl Pts',(-2.83044254225917,1.,2.54604736792655));
#42432=CARTESIAN_POINT('Ctrl Pts',(-2.83505269592536,-1.,2.55182152807077));
#42433=CARTESIAN_POINT('Ctrl Pts',(-2.83505269592536,1.,2.55182152807077));
#42434=CARTESIAN_POINT('Ctrl Pts',(-2.83942515220782,-1.,2.55749952145241));
#42435=CARTESIAN_POINT('Ctrl Pts',(-2.83942515220782,1.,2.55749952145241));
#42436=CARTESIAN_POINT('Ctrl Pts',(-2.84366802680237,-1.,2.56316920798513));
#42437=CARTESIAN_POINT('Ctrl Pts',(-2.84366802680237,1.,2.56316920798513));
#42438=CARTESIAN_POINT('Ctrl Pts',(-2.84788893329067,-1.,2.56891984251721));
#42439=CARTESIAN_POINT('Ctrl Pts',(-2.84788893329067,1.,2.56891984251721));
#42440=CARTESIAN_POINT('Ctrl Pts',(-2.85215360144431,-1.,2.57480482727081));
#42441=CARTESIAN_POINT('Ctrl Pts',(-2.85215360144431,1.,2.57480482727081));
#42442=CARTESIAN_POINT('Ctrl Pts',(-2.85647171715092,-1.,2.58082875254357));
#42443=CARTESIAN_POINT('Ctrl Pts',(-2.85647171715092,1.,2.58082875254357));
#42444=CARTESIAN_POINT('Ctrl Pts',(-2.86081999003629,-1.,2.58696770643524));
#42445=CARTESIAN_POINT('Ctrl Pts',(-2.86081999003629,1.,2.58696770643524));
#42446=CARTESIAN_POINT('Ctrl Pts',(-2.86515629953513,-1.,2.59318160184908));
#42447=CARTESIAN_POINT('Ctrl Pts',(-2.86515629953513,1.,2.59318160184908));
#42448=CARTESIAN_POINT('Ctrl Pts',(-2.86943633170722,-1.,2.5994287522321));
#42449=CARTESIAN_POINT('Ctrl Pts',(-2.86943633170722,1.,2.5994287522321));
#42450=CARTESIAN_POINT('Ctrl Pts',(-2.87363176656501,-1.,2.60568177881303));
#42451=CARTESIAN_POINT('Ctrl Pts',(-2.87363176656501,1.,2.60568177881303));
#42452=CARTESIAN_POINT('Ctrl Pts',(-2.87773881947916,-1.,2.61193507170955));
#42453=CARTESIAN_POINT('Ctrl Pts',(-2.87773881947916,1.,2.61193507170955));
#42454=CARTESIAN_POINT('Ctrl Pts',(-2.88176821427525,-1.,2.61819596473108));
#42455=CARTESIAN_POINT('Ctrl Pts',(-2.88176821427525,1.,2.61819596473108));
#42456=CARTESIAN_POINT('Ctrl Pts',(-2.88573922195059,-1.,2.62447947640262));
#42457=CARTESIAN_POINT('Ctrl Pts',(-2.88573922195059,1.,2.62447947640262));
#42458=CARTESIAN_POINT('Ctrl Pts',(-2.88967244854239,-1.,2.63080195420767));
#42459=CARTESIAN_POINT('Ctrl Pts',(-2.88967244854239,1.,2.63080195420767));
#42460=CARTESIAN_POINT('Ctrl Pts',(-2.89358228854544,-1.,2.63717442263932));
#42461=CARTESIAN_POINT('Ctrl Pts',(-2.89358228854544,1.,2.63717442263932));
#42462=CARTESIAN_POINT('Ctrl Pts',(-2.89747231723345,-1.,2.64359851684131));
#42463=CARTESIAN_POINT('Ctrl Pts',(-2.89747231723345,1.,2.64359851684131));
#42464=CARTESIAN_POINT('Ctrl Pts',(-2.90133950224867,-1.,2.65007017365564));
#42465=CARTESIAN_POINT('Ctrl Pts',(-2.90133950224867,1.,2.65007017365564));
#42466=CARTESIAN_POINT('Ctrl Pts',(-2.90517678087461,-1.,2.65658188464282));
#42467=CARTESIAN_POINT('Ctrl Pts',(-2.90517678087461,1.,2.65658188464282));
#42468=CARTESIAN_POINT('Ctrl Pts',(-2.90897617968923,-1.,2.6631254261681));
#42469=CARTESIAN_POINT('Ctrl Pts',(-2.90897617968923,1.,2.6631254261681));
#42470=CARTESIAN_POINT('Ctrl Pts',(-2.91273193382882,-1.,2.66969458792631));
#42471=CARTESIAN_POINT('Ctrl Pts',(-2.91273193382882,1.,2.66969458792631));
#42472=CARTESIAN_POINT('Ctrl Pts',(-2.91644290704285,-1.,2.67628728855312));
#42473=CARTESIAN_POINT('Ctrl Pts',(-2.91644290704285,1.,2.67628728855312));
#42474=CARTESIAN_POINT('Ctrl Pts',(-2.92011090722152,-1.,2.68290409279688));
#42475=CARTESIAN_POINT('Ctrl Pts',(-2.92011090722152,1.,2.68290409279688));
#42476=CARTESIAN_POINT('Ctrl Pts',(-2.92373955325875,-1.,2.68954721165339));
#42477=CARTESIAN_POINT('Ctrl Pts',(-2.92373955325875,1.,2.68954721165339));
#42478=CARTESIAN_POINT('Ctrl Pts',(-2.92733294395267,-1.,2.69621932864301));
#42479=CARTESIAN_POINT('Ctrl Pts',(-2.92733294395267,1.,2.69621932864301));
#42480=CARTESIAN_POINT('Ctrl Pts',(-2.9308943823375,-1.,2.70292247416885));
#42481=CARTESIAN_POINT('Ctrl Pts',(-2.9308943823375,1.,2.70292247416885));
#42482=CARTESIAN_POINT('Ctrl Pts',(-2.93442516311179,-1.,2.70965695523787));
#42483=CARTESIAN_POINT('Ctrl Pts',(-2.93442516311179,1.,2.70965695523787));
#42484=CARTESIAN_POINT('Ctrl Pts',(-2.93792519474972,-1.,2.71642190053592));
#42485=CARTESIAN_POINT('Ctrl Pts',(-2.93792519474972,1.,2.71642190053592));
#42486=CARTESIAN_POINT('Ctrl Pts',(-2.94139351933897,-1.,2.72321571511337));
#42487=CARTESIAN_POINT('Ctrl Pts',(-2.94139351933897,1.,2.72321571511337));
#42488=CARTESIAN_POINT('Ctrl Pts',(-2.94482887675143,-1.,2.73003657371617));
#42489=CARTESIAN_POINT('Ctrl Pts',(-2.94482887675143,1.,2.73003657371617));
#42490=CARTESIAN_POINT('Ctrl Pts',(-2.94823023414364,-1.,2.73688288329808));
#42491=CARTESIAN_POINT('Ctrl Pts',(-2.94823023414364,1.,2.73688288329808));
#42492=CARTESIAN_POINT('Ctrl Pts',(-2.95159737214266,-1.,2.74375379492172));
#42493=CARTESIAN_POINT('Ctrl Pts',(-2.95159737214266,1.,2.74375379492172));
#42494=CARTESIAN_POINT('Ctrl Pts',(-2.95493069316161,-1.,2.75064903318947));
#42495=CARTESIAN_POINT('Ctrl Pts',(-2.95493069316161,1.,2.75064903318947));
#42496=CARTESIAN_POINT('Ctrl Pts',(-2.95823097665896,-1.,2.7575686788835));
#42497=CARTESIAN_POINT('Ctrl Pts',(-2.95823097665896,1.,2.7575686788835));
#42498=CARTESIAN_POINT('Ctrl Pts',(-2.96149914764818,-1.,2.76451296269557));
#42499=CARTESIAN_POINT('Ctrl Pts',(-2.96149914764818,1.,2.76451296269557));
#42500=CARTESIAN_POINT('Ctrl Pts',(-2.96473605585583,-1.,2.77148206836498));
#42501=CARTESIAN_POINT('Ctrl Pts',(-2.96473605585583,1.,2.77148206836498));
#42502=CARTESIAN_POINT('Ctrl Pts',(-2.96794221043036,-1.,2.7784758954285));
#42503=CARTESIAN_POINT('Ctrl Pts',(-2.96794221043036,1.,2.7784758954285));
#42504=CARTESIAN_POINT('Ctrl Pts',(-2.97111781461465,-1.,2.78549409123769));
#42505=CARTESIAN_POINT('Ctrl Pts',(-2.97111781461465,1.,2.78549409123769));
#42506=CARTESIAN_POINT('Ctrl Pts',(-2.9742628834758,-1.,2.79253615718248));
#42507=CARTESIAN_POINT('Ctrl Pts',(-2.9742628834758,1.,2.79253615718248));
#42508=CARTESIAN_POINT('Ctrl Pts',(-2.97737733718287,-1.,2.7996015327823));
#42509=CARTESIAN_POINT('Ctrl Pts',(-2.97737733718287,1.,2.7996015327823));
#42510=CARTESIAN_POINT('Ctrl Pts',(-2.98046109647241,-1.,2.80668968101106));
#42511=CARTESIAN_POINT('Ctrl Pts',(-2.98046109647241,1.,2.80668968101106));
#42512=CARTESIAN_POINT('Ctrl Pts',(-2.98351419779767,-1.,2.81380019196286));
#42513=CARTESIAN_POINT('Ctrl Pts',(-2.98351419779767,1.,2.81380019196286));
#42514=CARTESIAN_POINT('Ctrl Pts',(-2.9865368066918,-1.,2.82093279065457));
#42515=CARTESIAN_POINT('Ctrl Pts',(-2.9865368066918,1.,2.82093279065457));
#42516=CARTESIAN_POINT('Ctrl Pts',(-2.98952916401446,-1.,2.82808728190157));
#42517=CARTESIAN_POINT('Ctrl Pts',(-2.98952916401446,1.,2.82808728190157));
#42518=CARTESIAN_POINT('Ctrl Pts',(-2.9924915517034,-1.,2.83526351254248));
#42519=CARTESIAN_POINT('Ctrl Pts',(-2.9924915517034,1.,2.83526351254248));
#42520=CARTESIAN_POINT('Ctrl Pts',(-2.99542425341685,-1.,2.84246132984415));
#42521=CARTESIAN_POINT('Ctrl Pts',(-2.99542425341685,1.,2.84246132984415));
#42522=CARTESIAN_POINT('Ctrl Pts',(-2.99832751144925,-1.,2.84968053289451));
#42523=CARTESIAN_POINT('Ctrl Pts',(-2.99832751144925,1.,2.84968053289451));
#42524=CARTESIAN_POINT('Ctrl Pts',(-3.00120150796095,-1.,2.85692085715686));
#42525=CARTESIAN_POINT('Ctrl Pts',(-3.00120150796095,1.,2.85692085715686));
#42526=CARTESIAN_POINT('Ctrl Pts',(-3.00404638316867,-1.,2.86418200833667));
#42527=CARTESIAN_POINT('Ctrl Pts',(-3.00404638316867,1.,2.86418200833667));
#42528=CARTESIAN_POINT('Ctrl Pts',(-3.00686224485784,-1.,2.87146368430502));
#42529=CARTESIAN_POINT('Ctrl Pts',(-3.00686224485784,1.,2.87146368430502));
#42530=CARTESIAN_POINT('Ctrl Pts',(-3.00964918108476,-1.,2.87876560072727));
#42531=CARTESIAN_POINT('Ctrl Pts',(-3.00964918108476,1.,2.87876560072727));
#42532=CARTESIAN_POINT('Ctrl Pts',(-3.01240727308829,-1.,2.8860875170608));
#42533=CARTESIAN_POINT('Ctrl Pts',(-3.01240727308829,1.,2.8860875170608));
#42534=CARTESIAN_POINT('Ctrl Pts',(-3.01513660431928,-1.,2.89342925566321));
#42535=CARTESIAN_POINT('Ctrl Pts',(-3.01513660431928,1.,2.89342925566321));
#42536=CARTESIAN_POINT('Ctrl Pts',(-3.01783725121981,-1.,2.9007906910105));
#42537=CARTESIAN_POINT('Ctrl Pts',(-3.01783725121981,1.,2.9007906910105));
#42538=CARTESIAN_POINT('Ctrl Pts',(-3.01997487193503,-1.,2.90669553302526));
#42539=CARTESIAN_POINT('Ctrl Pts',(-3.01997487193503,1.,2.90669553302526));
#42540=CARTESIAN_POINT('Ctrl Pts',(-3.02156522742431,-1.,2.91113297348212));
#42541=CARTESIAN_POINT('Ctrl Pts',(-3.02156522742431,1.,2.91113297348212));
#42542=CARTESIAN_POINT('Ctrl Pts',(-3.02261975104593,-1.,2.91409518070399));
#42543=CARTESIAN_POINT('Ctrl Pts',(-3.02261975104593,1.,2.91409518070399));
#42544=CARTESIAN_POINT('Ctrl Pts',(-3.02314558451372,-1.,2.91557726271063));
#42545=CARTESIAN_POINT('Ctrl Pts',(-3.02314558451372,1.,2.91557726271063));
#42546=CARTESIAN_POINT('',(-2.79140942341258,1.,2.50410331873176));
#42547=CARTESIAN_POINT('Ctrl Pts',(-2.79140942341258,-1.,2.50410331873176));
#42548=CARTESIAN_POINT('Ctrl Pts',(-2.79140942341258,-0.666666666666667,
2.50410331873176));
#42549=CARTESIAN_POINT('Ctrl Pts',(-2.79140942341258,-0.333333333333333,
2.50410331873176));
#42550=CARTESIAN_POINT('Ctrl Pts',(-2.79140942341258,0.333333333333333,
2.50410331873176));
#42551=CARTESIAN_POINT('Ctrl Pts',(-2.79140942341258,0.666666666666667,
2.50410331873176));
#42552=CARTESIAN_POINT('Ctrl Pts',(-2.79140942341258,1.,2.50410331873176));
#42553=CARTESIAN_POINT('',(-3.02314558451372,1.,2.91557726271063));
#42554=CARTESIAN_POINT('',(-3.02314558451372,0.,2.91557726271063));
#42555=CARTESIAN_POINT('Ctrl Pts',(-2.79140942341258,1.,2.50410331873176));
#42556=CARTESIAN_POINT('Ctrl Pts',(-2.79145823440781,1.,2.50410700351493));
#42557=CARTESIAN_POINT('Ctrl Pts',(-2.79164172518905,1.,2.50417932839313));
#42558=CARTESIAN_POINT('Ctrl Pts',(-2.79217568804755,1.,2.50455968395146));
#42559=CARTESIAN_POINT('Ctrl Pts',(-2.79344192164147,1.,2.50567182569081));
#42560=CARTESIAN_POINT('Ctrl Pts',(-2.79596878057287,1.,2.50810555977671));
#42561=CARTESIAN_POINT('Ctrl Pts',(-2.79970585014168,1.,2.51186983687818));
#42562=CARTESIAN_POINT('Ctrl Pts',(-2.80427363984653,1.,2.51660190465805));
#42563=CARTESIAN_POINT('Ctrl Pts',(-2.80941521966941,1.,2.52205778589653));
#42564=CARTESIAN_POINT('Ctrl Pts',(-2.81484379048475,1.,2.52796388055278));
#42565=CARTESIAN_POINT('Ctrl Pts',(-2.82028550483689,1.,2.53405679667412));
#42566=CARTESIAN_POINT('Ctrl Pts',(-2.8255216764922,1.,2.54012272520199));
#42567=CARTESIAN_POINT('Ctrl Pts',(-2.83044254225917,1.,2.54604736792655));
#42568=CARTESIAN_POINT('Ctrl Pts',(-2.83505269592536,1.,2.55182152807077));
#42569=CARTESIAN_POINT('Ctrl Pts',(-2.83942515220782,1.,2.55749952145241));
#42570=CARTESIAN_POINT('Ctrl Pts',(-2.84366802680237,1.,2.56316920798513));
#42571=CARTESIAN_POINT('Ctrl Pts',(-2.84788893329067,1.,2.56891984251721));
#42572=CARTESIAN_POINT('Ctrl Pts',(-2.85215360144431,1.,2.57480482727081));
#42573=CARTESIAN_POINT('Ctrl Pts',(-2.85647171715092,1.,2.58082875254357));
#42574=CARTESIAN_POINT('Ctrl Pts',(-2.86081999003629,1.,2.58696770643524));
#42575=CARTESIAN_POINT('Ctrl Pts',(-2.86515629953513,1.,2.59318160184908));
#42576=CARTESIAN_POINT('Ctrl Pts',(-2.86943633170722,1.,2.5994287522321));
#42577=CARTESIAN_POINT('Ctrl Pts',(-2.87363176656501,1.,2.60568177881303));
#42578=CARTESIAN_POINT('Ctrl Pts',(-2.87773881947916,1.,2.61193507170955));
#42579=CARTESIAN_POINT('Ctrl Pts',(-2.88176821427525,1.,2.61819596473108));
#42580=CARTESIAN_POINT('Ctrl Pts',(-2.88573922195059,1.,2.62447947640262));
#42581=CARTESIAN_POINT('Ctrl Pts',(-2.88967244854239,1.,2.63080195420767));
#42582=CARTESIAN_POINT('Ctrl Pts',(-2.89358228854544,1.,2.63717442263932));
#42583=CARTESIAN_POINT('Ctrl Pts',(-2.89747231723345,1.,2.64359851684131));
#42584=CARTESIAN_POINT('Ctrl Pts',(-2.90133950224867,1.,2.65007017365564));
#42585=CARTESIAN_POINT('Ctrl Pts',(-2.90517678087461,1.,2.65658188464282));
#42586=CARTESIAN_POINT('Ctrl Pts',(-2.90897617968923,1.,2.6631254261681));
#42587=CARTESIAN_POINT('Ctrl Pts',(-2.91273193382882,1.,2.66969458792631));
#42588=CARTESIAN_POINT('Ctrl Pts',(-2.91644290704285,1.,2.67628728855312));
#42589=CARTESIAN_POINT('Ctrl Pts',(-2.92011090722152,1.,2.68290409279688));
#42590=CARTESIAN_POINT('Ctrl Pts',(-2.92373955325875,1.,2.68954721165339));
#42591=CARTESIAN_POINT('Ctrl Pts',(-2.92733294395267,1.,2.69621932864301));
#42592=CARTESIAN_POINT('Ctrl Pts',(-2.9308943823375,1.,2.70292247416885));
#42593=CARTESIAN_POINT('Ctrl Pts',(-2.93442516311179,1.,2.70965695523787));
#42594=CARTESIAN_POINT('Ctrl Pts',(-2.93792519474972,1.,2.71642190053592));
#42595=CARTESIAN_POINT('Ctrl Pts',(-2.94139351933897,1.,2.72321571511337));
#42596=CARTESIAN_POINT('Ctrl Pts',(-2.94482887675143,1.,2.73003657371617));
#42597=CARTESIAN_POINT('Ctrl Pts',(-2.94823023414364,1.,2.73688288329808));
#42598=CARTESIAN_POINT('Ctrl Pts',(-2.95159737214266,1.,2.74375379492172));
#42599=CARTESIAN_POINT('Ctrl Pts',(-2.95493069316161,1.,2.75064903318947));
#42600=CARTESIAN_POINT('Ctrl Pts',(-2.95823097665896,1.,2.7575686788835));
#42601=CARTESIAN_POINT('Ctrl Pts',(-2.96149914764818,1.,2.76451296269557));
#42602=CARTESIAN_POINT('Ctrl Pts',(-2.96473605585583,1.,2.77148206836498));
#42603=CARTESIAN_POINT('Ctrl Pts',(-2.96794221043036,1.,2.7784758954285));
#42604=CARTESIAN_POINT('Ctrl Pts',(-2.97111781461465,1.,2.78549409123769));
#42605=CARTESIAN_POINT('Ctrl Pts',(-2.9742628834758,1.,2.79253615718248));
#42606=CARTESIAN_POINT('Ctrl Pts',(-2.97737733718287,1.,2.7996015327823));
#42607=CARTESIAN_POINT('Ctrl Pts',(-2.98046109647241,1.,2.80668968101106));
#42608=CARTESIAN_POINT('Ctrl Pts',(-2.98351419779767,1.,2.81380019196286));
#42609=CARTESIAN_POINT('Ctrl Pts',(-2.9865368066918,1.,2.82093279065457));
#42610=CARTESIAN_POINT('Ctrl Pts',(-2.98952916401446,1.,2.82808728190157));
#42611=CARTESIAN_POINT('Ctrl Pts',(-2.9924915517034,1.,2.83526351254248));
#42612=CARTESIAN_POINT('Ctrl Pts',(-2.99542425341685,1.,2.84246132984415));
#42613=CARTESIAN_POINT('Ctrl Pts',(-2.99832751144925,1.,2.84968053289451));
#42614=CARTESIAN_POINT('Ctrl Pts',(-3.00120150796095,1.,2.85692085715686));
#42615=CARTESIAN_POINT('Ctrl Pts',(-3.00404638316867,1.,2.86418200833667));
#42616=CARTESIAN_POINT('Ctrl Pts',(-3.00686224485784,1.,2.87146368430502));
#42617=CARTESIAN_POINT('Ctrl Pts',(-3.00964918108476,1.,2.87876560072727));
#42618=CARTESIAN_POINT('Ctrl Pts',(-3.01240727308829,1.,2.8860875170608));
#42619=CARTESIAN_POINT('Ctrl Pts',(-3.01513660431928,1.,2.89342925566321));
#42620=CARTESIAN_POINT('Ctrl Pts',(-3.01783725121981,1.,2.9007906910105));
#42621=CARTESIAN_POINT('Ctrl Pts',(-3.01997487193503,1.,2.90669553302526));
#42622=CARTESIAN_POINT('Ctrl Pts',(-3.02156522742431,1.,2.91113297348212));
#42623=CARTESIAN_POINT('Ctrl Pts',(-3.02261975104593,1.,2.91409518070399));
#42624=CARTESIAN_POINT('Ctrl Pts',(-3.02314558451372,1.,2.91557726271063));
#42625=CARTESIAN_POINT('Origin',(-3.02314558451372,0.,2.91557726271063));
#42626=CARTESIAN_POINT('',(-2.91557726271063,1.,3.02314558451372));
#42627=CARTESIAN_POINT('Origin',(0.,0.,0.));
#42628=CARTESIAN_POINT('',(-2.90994629141562,1.,2.36531447826213));
#42629=CARTESIAN_POINT('Origin',(0.,1.,0.));
#42630=CARTESIAN_POINT('Ctrl Pts',(-2.90994629141562,1.,2.36531447826213));
#42631=CARTESIAN_POINT('Ctrl Pts',(-2.90994629141562,0.666666666666667,
2.36531447826213));
#42632=CARTESIAN_POINT('Ctrl Pts',(-2.90994629141562,0.333333333333333,
2.36531447826213));
#42633=CARTESIAN_POINT('Ctrl Pts',(-2.90994629141562,-0.333333333333333,
2.36531447826213));
#42634=CARTESIAN_POINT('Ctrl Pts',(-2.90994629141562,-0.666666666666667,
2.36531447826213));
#42635=CARTESIAN_POINT('Ctrl Pts',(-2.90994629141562,-1.,2.36531447826213));
#42636=CARTESIAN_POINT('Ctrl Pts',(-3.35260583073571,-1.,2.52982887637028));
#42637=CARTESIAN_POINT('Ctrl Pts',(-3.35260583073571,1.,2.52982887637028));
#42638=CARTESIAN_POINT('Ctrl Pts',(-3.35105973714426,-1.,2.52954136549357));
#42639=CARTESIAN_POINT('Ctrl Pts',(-3.35105973714426,1.,2.52954136549357));
#42640=CARTESIAN_POINT('Ctrl Pts',(-3.34796903577628,-1.,2.5289632161143));
#42641=CARTESIAN_POINT('Ctrl Pts',(-3.34796903577628,1.,2.5289632161143));
#42642=CARTESIAN_POINT('Ctrl Pts',(-3.34333744117093,-1.,2.52808660916879));
#42643=CARTESIAN_POINT('Ctrl Pts',(-3.34333744117093,1.,2.52808660916879));
#42644=CARTESIAN_POINT('Ctrl Pts',(-3.33717090000955,-1.,2.52689902691551));
#42645=CARTESIAN_POINT('Ctrl Pts',(-3.33717090000955,1.,2.52689902691551));
#42646=CARTESIAN_POINT('Ctrl Pts',(-3.32947762189049,-1.,2.52538321165774));
#42647=CARTESIAN_POINT('Ctrl Pts',(-3.32947762189049,1.,2.52538321165774));
#42648=CARTESIAN_POINT('Ctrl Pts',(-3.32179931079521,-1.,2.52383598396878));
#42649=CARTESIAN_POINT('Ctrl Pts',(-3.32179931079521,1.,2.52383598396878));
#42650=CARTESIAN_POINT('Ctrl Pts',(-3.31413607874727,-1.,2.52225724871375));
#42651=CARTESIAN_POINT('Ctrl Pts',(-3.31413607874727,1.,2.52225724871375));
#42652=CARTESIAN_POINT('Ctrl Pts',(-3.30648808814986,-1.,2.52064689568167));
#42653=CARTESIAN_POINT('Ctrl Pts',(-3.30648808814986,1.,2.52064689568167));
#42654=CARTESIAN_POINT('Ctrl Pts',(-3.29885556387661,-1.,2.51900480700548));
#42655=CARTESIAN_POINT('Ctrl Pts',(-3.29885556387661,1.,2.51900480700548));
#42656=CARTESIAN_POINT('Ctrl Pts',(-3.2912387729863,-1.,2.51733085123316));
#42657=CARTESIAN_POINT('Ctrl Pts',(-3.2912387729863,1.,2.51733085123316));
#42658=CARTESIAN_POINT('Ctrl Pts',(-3.28363799702583,-1.,2.51562487464215));
#42659=CARTESIAN_POINT('Ctrl Pts',(-3.28363799702583,1.,2.51562487464215));
#42660=CARTESIAN_POINT('Ctrl Pts',(-3.27605350473048,-1.,2.51388669270329));
#42661=CARTESIAN_POINT('Ctrl Pts',(-3.27605350473048,1.,2.51388669270329));
#42662=CARTESIAN_POINT('Ctrl Pts',(-3.26848552888271,-1.,2.51211608411539));
#42663=CARTESIAN_POINT('Ctrl Pts',(-3.26848552888271,1.,2.51211608411539));
#42664=CARTESIAN_POINT('Ctrl Pts',(-3.26093423001716,-1.,2.51031277813697));
#42665=CARTESIAN_POINT('Ctrl Pts',(-3.26093423001716,1.,2.51031277813697));
#42666=CARTESIAN_POINT('Ctrl Pts',(-3.25339971461265,-1.,2.50847647070936));
#42667=CARTESIAN_POINT('Ctrl Pts',(-3.25339971461265,1.,2.50847647070936));
#42668=CARTESIAN_POINT('Ctrl Pts',(-3.24588208984042,-1.,2.50660685940645));
#42669=CARTESIAN_POINT('Ctrl Pts',(-3.24588208984042,1.,2.50660685940645));
#42670=CARTESIAN_POINT('Ctrl Pts',(-3.23838151080383,-1.,2.50470367580078));
#42671=CARTESIAN_POINT('Ctrl Pts',(-3.23838151080383,1.,2.50470367580078));
#42672=CARTESIAN_POINT('Ctrl Pts',(-3.23089822320596,-1.,2.50276671338074));
#42673=CARTESIAN_POINT('Ctrl Pts',(-3.23089822320596,1.,2.50276671338074));
#42674=CARTESIAN_POINT('Ctrl Pts',(-3.22343262620387,-1.,2.5007958720187));
#42675=CARTESIAN_POINT('Ctrl Pts',(-3.22343262620387,1.,2.5007958720187));
#42676=CARTESIAN_POINT('Ctrl Pts',(-3.21598526261157,-1.,2.49879114599293));
#42677=CARTESIAN_POINT('Ctrl Pts',(-3.21598526261157,1.,2.49879114599293));
#42678=CARTESIAN_POINT('Ctrl Pts',(-3.2085566984974,-1.,2.49675252647298));
#42679=CARTESIAN_POINT('Ctrl Pts',(-3.2085566984974,1.,2.49675252647298));
#42680=CARTESIAN_POINT('Ctrl Pts',(-3.20114742397549,-1.,2.49467992057726));
#42681=CARTESIAN_POINT('Ctrl Pts',(-3.20114742397549,1.,2.49467992057726));
#42682=CARTESIAN_POINT('Ctrl Pts',(-3.19375775555814,-1.,2.4925730723986));
#42683=CARTESIAN_POINT('Ctrl Pts',(-3.19375775555814,1.,2.4925730723986));
#42684=CARTESIAN_POINT('Ctrl Pts',(-3.18638771282315,-1.,2.49043146334095));
#42685=CARTESIAN_POINT('Ctrl Pts',(-3.18638771282315,1.,2.49043146334095));
#42686=CARTESIAN_POINT('Ctrl Pts',(-3.17903698136679,-1.,2.48825428288243));
#42687=CARTESIAN_POINT('Ctrl Pts',(-3.17903698136679,1.,2.48825428288243));
#42688=CARTESIAN_POINT('Ctrl Pts',(-3.17170518863357,-1.,2.48604065348619));
#42689=CARTESIAN_POINT('Ctrl Pts',(-3.17170518863357,1.,2.48604065348619));
#42690=CARTESIAN_POINT('Ctrl Pts',(-3.16439213290181,-1.,2.48378981792739));
#42691=CARTESIAN_POINT('Ctrl Pts',(-3.16439213290181,1.,2.48378981792739));
#42692=CARTESIAN_POINT('Ctrl Pts',(-3.15709802322735,-1.,2.48150133566568));
#42693=CARTESIAN_POINT('Ctrl Pts',(-3.15709802322735,1.,2.48150133566568));
#42694=CARTESIAN_POINT('Ctrl Pts',(-3.14982373241335,-1.,2.47917529057016));
#42695=CARTESIAN_POINT('Ctrl Pts',(-3.14982373241335,1.,2.47917529057016));
#42696=CARTESIAN_POINT('Ctrl Pts',(-3.14257099546531,-1.,2.47681245356095));
#42697=CARTESIAN_POINT('Ctrl Pts',(-3.14257099546531,1.,2.47681245356095));
#42698=CARTESIAN_POINT('Ctrl Pts',(-3.13534181229282,-1.,2.47441378371923));
#42699=CARTESIAN_POINT('Ctrl Pts',(-3.13534181229282,1.,2.47441378371923));
#42700=CARTESIAN_POINT('Ctrl Pts',(-3.12813790805948,-1.,2.47197997765868));
#42701=CARTESIAN_POINT('Ctrl Pts',(-3.12813790805948,1.,2.47197997765868));
#42702=CARTESIAN_POINT('Ctrl Pts',(-3.12096015766984,-1.,2.4695109894747));
#42703=CARTESIAN_POINT('Ctrl Pts',(-3.12096015766984,1.,2.4695109894747));
#42704=CARTESIAN_POINT('Ctrl Pts',(-3.11380805536124,-1.,2.46700558843507));
#42705=CARTESIAN_POINT('Ctrl Pts',(-3.11380805536124,1.,2.46700558843507));
#42706=CARTESIAN_POINT('Ctrl Pts',(-3.10667907901981,-1.,2.46446082979645));
#42707=CARTESIAN_POINT('Ctrl Pts',(-3.10667907901981,1.,2.46446082979645));
#42708=CARTESIAN_POINT('Ctrl Pts',(-3.09956993697048,-1.,2.4618730850188));
#42709=CARTESIAN_POINT('Ctrl Pts',(-3.09956993697048,1.,2.4618730850188));
#42710=CARTESIAN_POINT('Ctrl Pts',(-3.09247787931881,-1.,2.45923912563875));
#42711=CARTESIAN_POINT('Ctrl Pts',(-3.09247787931881,1.,2.45923912563875));
#42712=CARTESIAN_POINT('Ctrl Pts',(-3.08540206545313,-1.,2.45655725437037));
#42713=CARTESIAN_POINT('Ctrl Pts',(-3.08540206545313,1.,2.45655725437037));
#42714=CARTESIAN_POINT('Ctrl Pts',(-3.07834472886145,-1.,2.45382826787795));
#42715=CARTESIAN_POINT('Ctrl Pts',(-3.07834472886145,1.,2.45382826787795));
#42716=CARTESIAN_POINT('Ctrl Pts',(-3.0713129052131,-1.,2.45105688854432));
#42717=CARTESIAN_POINT('Ctrl Pts',(-3.0713129052131,1.,2.45105688854432));
#42718=CARTESIAN_POINT('Ctrl Pts',(-3.06431596421422,-1.,2.44824970516558));
#42719=CARTESIAN_POINT('Ctrl Pts',(-3.06431596421422,1.,2.44824970516558));
#42720=CARTESIAN_POINT('Ctrl Pts',(-3.05736242671521,-1.,2.44541251892568));
#42721=CARTESIAN_POINT('Ctrl Pts',(-3.05736242671521,1.,2.44541251892568));
#42722=CARTESIAN_POINT('Ctrl Pts',(-3.05045678021509,-1.,2.44254768923109));
#42723=CARTESIAN_POINT('Ctrl Pts',(-3.05045678021509,1.,2.44254768923109));
#42724=CARTESIAN_POINT('Ctrl Pts',(-3.04359685040545,-1.,2.43965194061849));
#42725=CARTESIAN_POINT('Ctrl Pts',(-3.04359685040545,1.,2.43965194061849));
#42726=CARTESIAN_POINT('Ctrl Pts',(-3.03676949672797,-1.,2.43671278042394));
#42727=CARTESIAN_POINT('Ctrl Pts',(-3.03676949672797,1.,2.43671278042394));
#42728=CARTESIAN_POINT('Ctrl Pts',(-3.02995534946946,-1.,2.43371241361462));
#42729=CARTESIAN_POINT('Ctrl Pts',(-3.02995534946946,1.,2.43371241361462));
#42730=CARTESIAN_POINT('Ctrl Pts',(-3.02313656035977,-1.,2.43063415586615));
#42731=CARTESIAN_POINT('Ctrl Pts',(-3.02313656035977,1.,2.43063415586615));
#42732=CARTESIAN_POINT('Ctrl Pts',(-3.01630420830494,-1.,2.4274685626416));
#42733=CARTESIAN_POINT('Ctrl Pts',(-3.01630420830494,1.,2.4274685626416));
#42734=CARTESIAN_POINT('Ctrl Pts',(-3.00946442616674,-1.,2.42421849439625));
#42735=CARTESIAN_POINT('Ctrl Pts',(-3.00946442616674,1.,2.42421849439625));
#42736=CARTESIAN_POINT('Ctrl Pts',(-3.00264868586038,-1.,2.42090763946812));
#42737=CARTESIAN_POINT('Ctrl Pts',(-3.00264868586038,1.,2.42090763946812));
#42738=CARTESIAN_POINT('Ctrl Pts',(-2.99590509293561,-1.,2.4175732450056));
#42739=CARTESIAN_POINT('Ctrl Pts',(-2.99590509293561,1.,2.4175732450056));
#42740=CARTESIAN_POINT('Ctrl Pts',(-2.98927983005851,-1.,2.4142506419963));
#42741=CARTESIAN_POINT('Ctrl Pts',(-2.98927983005851,1.,2.4142506419963));
#42742=CARTESIAN_POINT('Ctrl Pts',(-2.98280015815132,-1.,2.41095909342591));
#42743=CARTESIAN_POINT('Ctrl Pts',(-2.98280015815132,1.,2.41095909342591));
#42744=CARTESIAN_POINT('Ctrl Pts',(-2.97646002822395,-1.,2.40768975073691));
#42745=CARTESIAN_POINT('Ctrl Pts',(-2.97646002822395,1.,2.40768975073691));
#42746=CARTESIAN_POINT('Ctrl Pts',(-2.97019641312272,-1.,2.40438604734848));
#42747=CARTESIAN_POINT('Ctrl Pts',(-2.97019641312272,1.,2.40438604734848));
#42748=CARTESIAN_POINT('Ctrl Pts',(-2.96390432240181,-1.,2.40095565711535));
#42749=CARTESIAN_POINT('Ctrl Pts',(-2.96390432240181,1.,2.40095565711535));
#42750=CARTESIAN_POINT('Ctrl Pts',(-2.95748006482811,-1.,2.39730553974412));
#42751=CARTESIAN_POINT('Ctrl Pts',(-2.95748006482811,1.,2.39730553974412));
#42752=CARTESIAN_POINT('Ctrl Pts',(-2.95085857128372,-1.,2.39337207631613));
#42753=CARTESIAN_POINT('Ctrl Pts',(-2.95085857128372,1.,2.39337207631613));
#42754=CARTESIAN_POINT('Ctrl Pts',(-2.94404820669135,-1.,2.38914929090806));
#42755=CARTESIAN_POINT('Ctrl Pts',(-2.94404820669135,1.,2.38914929090806));
#42756=CARTESIAN_POINT('Ctrl Pts',(-2.93717903280599,-1.,2.38472771516476));
#42757=CARTESIAN_POINT('Ctrl Pts',(-2.93717903280599,1.,2.38472771516476));
#42758=CARTESIAN_POINT('Ctrl Pts',(-2.93049643640517,-1.,2.3802898958232));
#42759=CARTESIAN_POINT('Ctrl Pts',(-2.93049643640517,1.,2.3802898958232));
#42760=CARTESIAN_POINT('Ctrl Pts',(-2.92430340582912,-1.,2.37606510524271));
#42761=CARTESIAN_POINT('Ctrl Pts',(-2.92430340582912,1.,2.37606510524271));
#42762=CARTESIAN_POINT('Ctrl Pts',(-2.9189150379156,-1.,2.37229381109939));
#42763=CARTESIAN_POINT('Ctrl Pts',(-2.9189150379156,1.,2.37229381109939));
#42764=CARTESIAN_POINT('Ctrl Pts',(-2.91461249883016,-1.,2.36919161373074));
#42765=CARTESIAN_POINT('Ctrl Pts',(-2.91461249883016,1.,2.36919161373074));
#42766=CARTESIAN_POINT('Ctrl Pts',(-2.9115863784165,-1.,2.36690501170317));
#42767=CARTESIAN_POINT('Ctrl Pts',(-2.9115863784165,1.,2.36690501170317));
#42768=CARTESIAN_POINT('Ctrl Pts',(-2.91025813829606,-1.,2.36578327194396));
#42769=CARTESIAN_POINT('Ctrl Pts',(-2.91025813829606,1.,2.36578327194396));
#42770=CARTESIAN_POINT('Ctrl Pts',(-2.90989022547738,-1.,2.36535052956704));
#42771=CARTESIAN_POINT('Ctrl Pts',(-2.90989022547738,1.,2.36535052956704));
#42772=CARTESIAN_POINT('Ctrl Pts',(-2.90992398626098,-1.,2.36524348105023));
#42773=CARTESIAN_POINT('Ctrl Pts',(-2.90992398626098,1.,2.36524348105023));
#42774=CARTESIAN_POINT('Ctrl Pts',(-2.91001063062876,-1.,2.36523532225181));
#42775=CARTESIAN_POINT('Ctrl Pts',(-2.91001063062876,1.,2.36523532225181));
#42776=CARTESIAN_POINT('',(-3.35260583073571,1.,2.52982887637028));
#42777=CARTESIAN_POINT('Ctrl Pts',(-3.35260583073571,1.,2.52982887637028));
#42778=CARTESIAN_POINT('Ctrl Pts',(-3.35105973714426,1.,2.52954136549357));
#42779=CARTESIAN_POINT('Ctrl Pts',(-3.34796903577628,1.,2.5289632161143));
#42780=CARTESIAN_POINT('Ctrl Pts',(-3.34333744117093,1.,2.52808660916879));
#42781=CARTESIAN_POINT('Ctrl Pts',(-3.33717090000955,1.,2.52689902691551));
#42782=CARTESIAN_POINT('Ctrl Pts',(-3.32947762189049,1.,2.52538321165774));
#42783=CARTESIAN_POINT('Ctrl Pts',(-3.32179931079521,1.,2.52383598396878));
#42784=CARTESIAN_POINT('Ctrl Pts',(-3.31413607874727,1.,2.52225724871375));
#42785=CARTESIAN_POINT('Ctrl Pts',(-3.30648808814986,1.,2.52064689568167));
#42786=CARTESIAN_POINT('Ctrl Pts',(-3.29885556387661,1.,2.51900480700548));
#42787=CARTESIAN_POINT('Ctrl Pts',(-3.2912387729863,1.,2.51733085123316));
#42788=CARTESIAN_POINT('Ctrl Pts',(-3.28363799702583,1.,2.51562487464215));
#42789=CARTESIAN_POINT('Ctrl Pts',(-3.27605350473048,1.,2.51388669270329));
#42790=CARTESIAN_POINT('Ctrl Pts',(-3.26848552888271,1.,2.51211608411539));
#42791=CARTESIAN_POINT('Ctrl Pts',(-3.26093423001716,1.,2.51031277813697));
#42792=CARTESIAN_POINT('Ctrl Pts',(-3.25339971461265,1.,2.50847647070936));
#42793=CARTESIAN_POINT('Ctrl Pts',(-3.24588208984042,1.,2.50660685940645));
#42794=CARTESIAN_POINT('Ctrl Pts',(-3.23838151080383,1.,2.50470367580078));
#42795=CARTESIAN_POINT('Ctrl Pts',(-3.23089822320596,1.,2.50276671338074));
#42796=CARTESIAN_POINT('Ctrl Pts',(-3.22343262620387,1.,2.5007958720187));
#42797=CARTESIAN_POINT('Ctrl Pts',(-3.21598526261157,1.,2.49879114599293));
#42798=CARTESIAN_POINT('Ctrl Pts',(-3.2085566984974,1.,2.49675252647298));
#42799=CARTESIAN_POINT('Ctrl Pts',(-3.20114742397549,1.,2.49467992057726));
#42800=CARTESIAN_POINT('Ctrl Pts',(-3.19375775555814,1.,2.4925730723986));
#42801=CARTESIAN_POINT('Ctrl Pts',(-3.18638771282315,1.,2.49043146334095));
#42802=CARTESIAN_POINT('Ctrl Pts',(-3.17903698136679,1.,2.48825428288243));
#42803=CARTESIAN_POINT('Ctrl Pts',(-3.17170518863357,1.,2.48604065348619));
#42804=CARTESIAN_POINT('Ctrl Pts',(-3.16439213290181,1.,2.48378981792739));
#42805=CARTESIAN_POINT('Ctrl Pts',(-3.15709802322735,1.,2.48150133566568));
#42806=CARTESIAN_POINT('Ctrl Pts',(-3.14982373241335,1.,2.47917529057016));
#42807=CARTESIAN_POINT('Ctrl Pts',(-3.14257099546531,1.,2.47681245356095));
#42808=CARTESIAN_POINT('Ctrl Pts',(-3.13534181229282,1.,2.47441378371923));
#42809=CARTESIAN_POINT('Ctrl Pts',(-3.12813790805948,1.,2.47197997765868));
#42810=CARTESIAN_POINT('Ctrl Pts',(-3.12096015766984,1.,2.4695109894747));
#42811=CARTESIAN_POINT('Ctrl Pts',(-3.11380805536124,1.,2.46700558843507));
#42812=CARTESIAN_POINT('Ctrl Pts',(-3.10667907901981,1.,2.46446082979645));
#42813=CARTESIAN_POINT('Ctrl Pts',(-3.09956993697048,1.,2.4618730850188));
#42814=CARTESIAN_POINT('Ctrl Pts',(-3.09247787931881,1.,2.45923912563875));
#42815=CARTESIAN_POINT('Ctrl Pts',(-3.08540206545313,1.,2.45655725437037));
#42816=CARTESIAN_POINT('Ctrl Pts',(-3.07834472886145,1.,2.45382826787795));
#42817=CARTESIAN_POINT('Ctrl Pts',(-3.0713129052131,1.,2.45105688854432));
#42818=CARTESIAN_POINT('Ctrl Pts',(-3.06431596421422,1.,2.44824970516558));
#42819=CARTESIAN_POINT('Ctrl Pts',(-3.05736242671521,1.,2.44541251892568));
#42820=CARTESIAN_POINT('Ctrl Pts',(-3.05045678021509,1.,2.44254768923109));
#42821=CARTESIAN_POINT('Ctrl Pts',(-3.04359685040545,1.,2.43965194061849));
#42822=CARTESIAN_POINT('Ctrl Pts',(-3.03676949672797,1.,2.43671278042394));
#42823=CARTESIAN_POINT('Ctrl Pts',(-3.02995534946946,1.,2.43371241361462));
#42824=CARTESIAN_POINT('Ctrl Pts',(-3.02313656035977,1.,2.43063415586615));
#42825=CARTESIAN_POINT('Ctrl Pts',(-3.01630420830494,1.,2.4274685626416));
#42826=CARTESIAN_POINT('Ctrl Pts',(-3.00946442616674,1.,2.42421849439625));
#42827=CARTESIAN_POINT('Ctrl Pts',(-3.00264868586038,1.,2.42090763946812));
#42828=CARTESIAN_POINT('Ctrl Pts',(-2.99590509293561,1.,2.4175732450056));
#42829=CARTESIAN_POINT('Ctrl Pts',(-2.98927983005851,1.,2.4142506419963));
#42830=CARTESIAN_POINT('Ctrl Pts',(-2.98280015815132,1.,2.41095909342591));
#42831=CARTESIAN_POINT('Ctrl Pts',(-2.97646002822395,1.,2.40768975073691));
#42832=CARTESIAN_POINT('Ctrl Pts',(-2.97019641312272,1.,2.40438604734848));
#42833=CARTESIAN_POINT('Ctrl Pts',(-2.96390432240181,1.,2.40095565711535));
#42834=CARTESIAN_POINT('Ctrl Pts',(-2.95748006482811,1.,2.39730553974412));
#42835=CARTESIAN_POINT('Ctrl Pts',(-2.95085857128372,1.,2.39337207631613));
#42836=CARTESIAN_POINT('Ctrl Pts',(-2.94404820669135,1.,2.38914929090806));
#42837=CARTESIAN_POINT('Ctrl Pts',(-2.93717903280599,1.,2.38472771516476));
#42838=CARTESIAN_POINT('Ctrl Pts',(-2.93049643640517,1.,2.3802898958232));
#42839=CARTESIAN_POINT('Ctrl Pts',(-2.92430340582912,1.,2.37606510524271));
#42840=CARTESIAN_POINT('Ctrl Pts',(-2.9189150379156,1.,2.37229381109939));
#42841=CARTESIAN_POINT('Ctrl Pts',(-2.91461249883016,1.,2.36919161373074));
#42842=CARTESIAN_POINT('Ctrl Pts',(-2.91181344022628,1.,2.36707658451709));
#42843=CARTESIAN_POINT('Ctrl Pts',(-2.91051690822262,1.,2.36599991765853));
#42844=CARTESIAN_POINT('Ctrl Pts',(-2.9100577052777,1.,2.36553202948741));
#42845=CARTESIAN_POINT('Ctrl Pts',(-2.90995756655559,1.,2.3653621118858));
#42846=CARTESIAN_POINT('Ctrl Pts',(-2.90994629141563,1.,2.36531447826213));
#42847=CARTESIAN_POINT('',(-3.35260583073571,0.,2.52982887637028));
#42848=CARTESIAN_POINT('Ctrl Pts',(-3.1487152044751,-1.,2.03668666247593));
#42849=CARTESIAN_POINT('Ctrl Pts',(-3.1487152044751,1.,2.03668666247593));
#42850=CARTESIAN_POINT('Ctrl Pts',(-3.14869618937258,-1.,2.03660173757879));
#42851=CARTESIAN_POINT('Ctrl Pts',(-3.14869618937258,1.,2.03660173757879));
#42852=CARTESIAN_POINT('Ctrl Pts',(-3.14878756590812,-1.,2.03653654935592));
#42853=CARTESIAN_POINT('Ctrl Pts',(-3.14878756590812,1.,2.03653654935592));
#42854=CARTESIAN_POINT('Ctrl Pts',(-3.14931281968048,-1.,2.03675273049189));
#42855=CARTESIAN_POINT('Ctrl Pts',(-3.14931281968048,1.,2.03675273049189));
#42856=CARTESIAN_POINT('Ctrl Pts',(-3.15079010635742,-1.,2.03766932526445));
#42857=CARTESIAN_POINT('Ctrl Pts',(-3.15079010635742,1.,2.03766932526445));
#42858=CARTESIAN_POINT('Ctrl Pts',(-3.15389991674792,-1.,2.03984073791519));
#42859=CARTESIAN_POINT('Ctrl Pts',(-3.15389991674792,1.,2.03984073791519));
#42860=CARTESIAN_POINT('Ctrl Pts',(-3.15817983946367,-1.,2.04297406404027));
#42861=CARTESIAN_POINT('Ctrl Pts',(-3.15817983946367,1.,2.04297406404027));
#42862=CARTESIAN_POINT('Ctrl Pts',(-3.16343165058912,-1.,2.04693331247446));
#42863=CARTESIAN_POINT('Ctrl Pts',(-3.16343165058912,1.,2.04693331247446));
#42864=CARTESIAN_POINT('Ctrl Pts',(-3.16936341689527,-1.,2.05151770247233));
#42865=CARTESIAN_POINT('Ctrl Pts',(-3.16936341689527,1.,2.05151770247233));
#42866=CARTESIAN_POINT('Ctrl Pts',(-3.17564906975371,-1.,2.05650186773132));
#42867=CARTESIAN_POINT('Ctrl Pts',(-3.17564906975371,1.,2.05650186773132));
#42868=CARTESIAN_POINT('Ctrl Pts',(-3.18197692964614,-1.,2.06166849827101));
#42869=CARTESIAN_POINT('Ctrl Pts',(-3.18197692964614,1.,2.06166849827101));
#42870=CARTESIAN_POINT('Ctrl Pts',(-3.18809755562368,-1.,2.06684062744112));
#42871=CARTESIAN_POINT('Ctrl Pts',(-3.18809755562368,1.,2.06684062744112));
#42872=CARTESIAN_POINT('Ctrl Pts',(-3.19388465568252,-1.,2.07192253497857));
#42873=CARTESIAN_POINT('Ctrl Pts',(-3.19388465568252,1.,2.07192253497857));
#42874=CARTESIAN_POINT('Ctrl Pts',(-3.19934132836019,-1.,2.07690441870722));
#42875=CARTESIAN_POINT('Ctrl Pts',(-3.19934132836019,1.,2.07690441870722));
#42876=CARTESIAN_POINT('Ctrl Pts',(-3.2045481863073,-1.,2.08182850370878));
#42877=CARTESIAN_POINT('Ctrl Pts',(-3.2045481863073,1.,2.08182850370878));
#42878=CARTESIAN_POINT('Ctrl Pts',(-3.20962575845463,-1.,2.08676465517455));
#42879=CARTESIAN_POINT('Ctrl Pts',(-3.20962575845463,1.,2.08676465517455));
#42880=CARTESIAN_POINT('Ctrl Pts',(-3.21469429601654,-1.,2.09178419460443));
#42881=CARTESIAN_POINT('Ctrl Pts',(-3.21469429601654,1.,2.09178419460443));
#42882=CARTESIAN_POINT('Ctrl Pts',(-3.21982707347009,-1.,2.09692958434895));
#42883=CARTESIAN_POINT('Ctrl Pts',(-3.21982707347009,1.,2.09692958434895));
#42884=CARTESIAN_POINT('Ctrl Pts',(-3.22503437553434,-1.,2.10220384298492));
#42885=CARTESIAN_POINT('Ctrl Pts',(-3.22503437553434,1.,2.10220384298492));
#42886=CARTESIAN_POINT('Ctrl Pts',(-3.23028945793289,-1.,2.10758699642451));
#42887=CARTESIAN_POINT('Ctrl Pts',(-3.23028945793289,1.,2.10758699642451));
#42888=CARTESIAN_POINT('Ctrl Pts',(-3.23554444767099,-1.,2.11304604021773));
#42889=CARTESIAN_POINT('Ctrl Pts',(-3.23554444767099,1.,2.11304604021773));
#42890=CARTESIAN_POINT('Ctrl Pts',(-3.24074905517293,-1.,2.11854673326979));
#42891=CARTESIAN_POINT('Ctrl Pts',(-3.24074905517293,1.,2.11854673326979));
#42892=CARTESIAN_POINT('Ctrl Pts',(-3.24587102613376,-1.,2.12406646410962));
#42893=CARTESIAN_POINT('Ctrl Pts',(-3.24587102613376,1.,2.12406646410962));
#42894=CARTESIAN_POINT('Ctrl Pts',(-3.25090574494028,-1.,2.12960028396832));
#42895=CARTESIAN_POINT('Ctrl Pts',(-3.25090574494028,1.,2.12960028396832));
#42896=CARTESIAN_POINT('Ctrl Pts',(-3.25586495065054,-1.,2.13515375878803));
#42897=CARTESIAN_POINT('Ctrl Pts',(-3.25586495065054,1.,2.13515375878803));
#42898=CARTESIAN_POINT('Ctrl Pts',(-3.26077002641879,-1.,2.14073870754264));
#42899=CARTESIAN_POINT('Ctrl Pts',(-3.26077002641879,1.,2.14073870754264));
#42900=CARTESIAN_POINT('Ctrl Pts',(-3.26564388189759,-1.,2.1463680529566));
#42901=CARTESIAN_POINT('Ctrl Pts',(-3.26564388189759,1.,2.1463680529566));
#42902=CARTESIAN_POINT('Ctrl Pts',(-3.27050245897228,-1.,2.15205043199808));
#42903=CARTESIAN_POINT('Ctrl Pts',(-3.27050245897228,1.,2.15205043199808));
#42904=CARTESIAN_POINT('Ctrl Pts',(-3.27534954469187,-1.,2.15778690038347));
#42905=CARTESIAN_POINT('Ctrl Pts',(-3.27534954469187,1.,2.15778690038347));
#42906=CARTESIAN_POINT('Ctrl Pts',(-3.280181508414,-1.,2.16357391934425));
#42907=CARTESIAN_POINT('Ctrl Pts',(-3.280181508414,1.,2.16357391934425));
#42908=CARTESIAN_POINT('Ctrl Pts',(-3.28499019979724,-1.,2.16940517773455));
#42909=CARTESIAN_POINT('Ctrl Pts',(-3.28499019979724,1.,2.16940517773455));
#42910=CARTESIAN_POINT('Ctrl Pts',(-3.28976645712568,-1.,2.17527380048423));
#42911=CARTESIAN_POINT('Ctrl Pts',(-3.28976645712568,1.,2.17527380048423));
#42912=CARTESIAN_POINT('Ctrl Pts',(-3.2945036150049,-1.,2.18117455557065));
#42913=CARTESIAN_POINT('Ctrl Pts',(-3.2945036150049,1.,2.18117455557065));
#42914=CARTESIAN_POINT('Ctrl Pts',(-3.29920022557639,-1.,2.18710556500327));
#42915=CARTESIAN_POINT('Ctrl Pts',(-3.29920022557639,1.,2.18710556500327));
#42916=CARTESIAN_POINT('Ctrl Pts',(-3.30385816281831,-1.,2.19306710376111));
#42917=CARTESIAN_POINT('Ctrl Pts',(-3.30385816281831,1.,2.19306710376111));
#42918=CARTESIAN_POINT('Ctrl Pts',(-3.30848134694595,-1.,2.19906078949923));
#42919=CARTESIAN_POINT('Ctrl Pts',(-3.30848134694595,1.,2.19906078949923));
#42920=CARTESIAN_POINT('Ctrl Pts',(-3.31307424608949,-1.,2.20508863150607));
#42921=CARTESIAN_POINT('Ctrl Pts',(-3.31307424608949,1.,2.20508863150607));
#42922=CARTESIAN_POINT('Ctrl Pts',(-3.31764044024235,-1.,2.21115211847875));
#42923=CARTESIAN_POINT('Ctrl Pts',(-3.31764044024235,1.,2.21115211847875));
#42924=CARTESIAN_POINT('Ctrl Pts',(-3.32218125618968,-1.,2.21725135110898));
#42925=CARTESIAN_POINT('Ctrl Pts',(-3.32218125618968,1.,2.21725135110898));
#42926=CARTESIAN_POINT('Ctrl Pts',(-3.3266964672289,-1.,2.22338548312772));
#42927=CARTESIAN_POINT('Ctrl Pts',(-3.3266964672289,1.,2.22338548312772));
#42928=CARTESIAN_POINT('Ctrl Pts',(-3.33118487773611,-1.,2.22955308907233));
#42929=CARTESIAN_POINT('Ctrl Pts',(-3.33118487773611,1.,2.22955308907233));
#42930=CARTESIAN_POINT('Ctrl Pts',(-3.33564495756482,-1.,2.23575256328812));
#42931=CARTESIAN_POINT('Ctrl Pts',(-3.33564495756482,1.,2.23575256328812));
#42932=CARTESIAN_POINT('Ctrl Pts',(-3.34007543738025,-1.,2.24198249391422));
#42933=CARTESIAN_POINT('Ctrl Pts',(-3.34007543738025,1.,2.24198249391422));
#42934=CARTESIAN_POINT('Ctrl Pts',(-3.34447596770723,-1.,2.24824207678256));
#42935=CARTESIAN_POINT('Ctrl Pts',(-3.34447596770723,1.,2.24824207678256));
#42936=CARTESIAN_POINT('Ctrl Pts',(-3.34884690292285,-1.,2.25453097693483));
#42937=CARTESIAN_POINT('Ctrl Pts',(-3.34884690292285,1.,2.25453097693483));
#42938=CARTESIAN_POINT('Ctrl Pts',(-3.35318902552626,-1.,2.26084915222449));
#42939=CARTESIAN_POINT('Ctrl Pts',(-3.35318902552626,1.,2.26084915222449));
#42940=CARTESIAN_POINT('Ctrl Pts',(-3.35750328523061,-1.,2.2671966857991));
#42941=CARTESIAN_POINT('Ctrl Pts',(-3.35750328523061,1.,2.2671966857991));
#42942=CARTESIAN_POINT('Ctrl Pts',(-3.36179055004409,-1.,2.2735736262093));
#42943=CARTESIAN_POINT('Ctrl Pts',(-3.36179055004409,1.,2.2735736262093));
#42944=CARTESIAN_POINT('Ctrl Pts',(-3.36605130713076,-1.,2.27997979458037));
#42945=CARTESIAN_POINT('Ctrl Pts',(-3.36605130713076,1.,2.27997979458037));
#42946=CARTESIAN_POINT('Ctrl Pts',(-3.37028570206488,-1.,2.28641481081137));
#42947=CARTESIAN_POINT('Ctrl Pts',(-3.37028570206488,1.,2.28641481081137));
#42948=CARTESIAN_POINT('Ctrl Pts',(-3.37449367172826,-1.,2.29287818007393));
#42949=CARTESIAN_POINT('Ctrl Pts',(-3.37449367172826,1.,2.29287818007393));
#42950=CARTESIAN_POINT('Ctrl Pts',(-3.37867504959433,-1.,2.29936936127624));
#42951=CARTESIAN_POINT('Ctrl Pts',(-3.37867504959433,1.,2.29936936127624));
#42952=CARTESIAN_POINT('Ctrl Pts',(-3.3828296733661,-1.,2.30588783640343));
#42953=CARTESIAN_POINT('Ctrl Pts',(-3.3828296733661,1.,2.30588783640343));
#42954=CARTESIAN_POINT('Ctrl Pts',(-3.38695751492462,-1.,2.31243319489367));
#42955=CARTESIAN_POINT('Ctrl Pts',(-3.38695751492462,1.,2.31243319489367));
#42956=CARTESIAN_POINT('Ctrl Pts',(-3.39105869474822,-1.,2.31900513925424));
#42957=CARTESIAN_POINT('Ctrl Pts',(-3.39105869474822,1.,2.31900513925424));
#42958=CARTESIAN_POINT('Ctrl Pts',(-3.39513342019756,-1.,2.3256034390248));
#42959=CARTESIAN_POINT('Ctrl Pts',(-3.39513342019756,1.,2.3256034390248));
#42960=CARTESIAN_POINT('Ctrl Pts',(-3.39918194577956,-1.,2.33222789882489));
#42961=CARTESIAN_POINT('Ctrl Pts',(-3.39918194577956,1.,2.33222789882489));
#42962=CARTESIAN_POINT('Ctrl Pts',(-3.40320452776743,-1.,2.33887832342782));
#42963=CARTESIAN_POINT('Ctrl Pts',(-3.40320452776743,1.,2.33887832342782));
#42964=CARTESIAN_POINT('Ctrl Pts',(-3.40720137404297,-1.,2.34555447649188));
#42965=CARTESIAN_POINT('Ctrl Pts',(-3.40720137404297,1.,2.34555447649188));
#42966=CARTESIAN_POINT('Ctrl Pts',(-3.41117262314119,-1.,2.35225606824109));
#42967=CARTESIAN_POINT('Ctrl Pts',(-3.41117262314119,1.,2.35225606824109));
#42968=CARTESIAN_POINT('Ctrl Pts',(-3.41511836751469,-1.,2.35898278606946));
#42969=CARTESIAN_POINT('Ctrl Pts',(-3.41511836751469,1.,2.35898278606946));
#42970=CARTESIAN_POINT('Ctrl Pts',(-3.41903866635852,-1.,2.36573431470642));
#42971=CARTESIAN_POINT('Ctrl Pts',(-3.41903866635852,1.,2.36573431470642));
#42972=CARTESIAN_POINT('Ctrl Pts',(-3.42293356216511,-1.,2.37251035954292));
#42973=CARTESIAN_POINT('Ctrl Pts',(-3.42293356216511,1.,2.37251035954292));
#42974=CARTESIAN_POINT('Ctrl Pts',(-3.42680309754399,-1.,2.37931067028926));
#42975=CARTESIAN_POINT('Ctrl Pts',(-3.42680309754399,1.,2.37931067028926));
#42976=CARTESIAN_POINT('Ctrl Pts',(-3.4306473271292,-1.,2.38613505843552));
#42977=CARTESIAN_POINT('Ctrl Pts',(-3.4306473271292,1.,2.38613505843552));
#42978=CARTESIAN_POINT('Ctrl Pts',(-3.4344663067854,-1.,2.39298338804493));
#42979=CARTESIAN_POINT('Ctrl Pts',(-3.4344663067854,1.,2.39298338804493));
#42980=CARTESIAN_POINT('Ctrl Pts',(-3.43750133064416,-1.,2.39848113410292));
#42981=CARTESIAN_POINT('Ctrl Pts',(-3.43750133064416,1.,2.39848113410292));
#42982=CARTESIAN_POINT('Ctrl Pts',(-3.43976627484234,-1.,2.40261515589405));
#42983=CARTESIAN_POINT('Ctrl Pts',(-3.43976627484234,1.,2.40261515589405));
#42984=CARTESIAN_POINT('Ctrl Pts',(-3.44127120683039,-1.,2.4053759295909));
#42985=CARTESIAN_POINT('Ctrl Pts',(-3.44127120683039,1.,2.4053759295909));
#42986=CARTESIAN_POINT('Ctrl Pts',(-3.44202241512147,-1.,2.40675750623143));
#42987=CARTESIAN_POINT('Ctrl Pts',(-3.44202241512147,1.,2.40675750623143));
#42988=CARTESIAN_POINT('',(-3.14877060440327,1.,2.03660101169715));
#42989=CARTESIAN_POINT('Ctrl Pts',(-3.14877060440327,-1.,2.03660101169715));
#42990=CARTESIAN_POINT('Ctrl Pts',(-3.14877060440327,-0.666666666666667,
2.03660101169715));
#42991=CARTESIAN_POINT('Ctrl Pts',(-3.14877060440327,-0.333333333333333,
2.03660101169715));
#42992=CARTESIAN_POINT('Ctrl Pts',(-3.14877060440327,0.333333333333333,
2.03660101169715));
#42993=CARTESIAN_POINT('Ctrl Pts',(-3.14877060440327,0.666666666666667,
2.03660101169715));
#42994=CARTESIAN_POINT('Ctrl Pts',(-3.14877060440327,1.,2.03660101169715));
#42995=CARTESIAN_POINT('',(-3.44202241512147,1.,2.40675750623143));
#42996=CARTESIAN_POINT('',(-3.44202241512147,0.,2.40675750623143));
#42997=CARTESIAN_POINT('Ctrl Pts',(-3.14877060440327,1.,2.03660101169715));
#42998=CARTESIAN_POINT('Ctrl Pts',(-3.14881939088124,1.,2.03659701539259));
#42999=CARTESIAN_POINT('Ctrl Pts',(-3.1490119366901,1.,2.03663974554932));
#43000=CARTESIAN_POINT('Ctrl Pts',(-3.14959882629805,1.,2.03693188810544));
#43001=CARTESIAN_POINT('Ctrl Pts',(-3.15102344775328,1.,2.03783225495961));
#43002=CARTESIAN_POINT('Ctrl Pts',(-3.15389991674792,1.,2.03984073791519));
#43003=CARTESIAN_POINT('Ctrl Pts',(-3.15817983946367,1.,2.04297406404027));
#43004=CARTESIAN_POINT('Ctrl Pts',(-3.16343165058912,1.,2.04693331247446));
#43005=CARTESIAN_POINT('Ctrl Pts',(-3.16936341689527,1.,2.05151770247233));
#43006=CARTESIAN_POINT('Ctrl Pts',(-3.17564906975371,1.,2.05650186773132));
#43007=CARTESIAN_POINT('Ctrl Pts',(-3.18197692964614,1.,2.06166849827101));
#43008=CARTESIAN_POINT('Ctrl Pts',(-3.18809755562368,1.,2.06684062744112));
#43009=CARTESIAN_POINT('Ctrl Pts',(-3.19388465568252,1.,2.07192253497857));
#43010=CARTESIAN_POINT('Ctrl Pts',(-3.19934132836019,1.,2.07690441870722));
#43011=CARTESIAN_POINT('Ctrl Pts',(-3.2045481863073,1.,2.08182850370878));
#43012=CARTESIAN_POINT('Ctrl Pts',(-3.20962575845463,1.,2.08676465517455));
#43013=CARTESIAN_POINT('Ctrl Pts',(-3.21469429601654,1.,2.09178419460443));
#43014=CARTESIAN_POINT('Ctrl Pts',(-3.21982707347009,1.,2.09692958434895));
#43015=CARTESIAN_POINT('Ctrl Pts',(-3.22503437553434,1.,2.10220384298492));
#43016=CARTESIAN_POINT('Ctrl Pts',(-3.23028945793289,1.,2.10758699642451));
#43017=CARTESIAN_POINT('Ctrl Pts',(-3.23554444767099,1.,2.11304604021773));
#43018=CARTESIAN_POINT('Ctrl Pts',(-3.24074905517293,1.,2.11854673326979));
#43019=CARTESIAN_POINT('Ctrl Pts',(-3.24587102613376,1.,2.12406646410962));
#43020=CARTESIAN_POINT('Ctrl Pts',(-3.25090574494028,1.,2.12960028396832));
#43021=CARTESIAN_POINT('Ctrl Pts',(-3.25586495065054,1.,2.13515375878803));
#43022=CARTESIAN_POINT('Ctrl Pts',(-3.26077002641879,1.,2.14073870754264));
#43023=CARTESIAN_POINT('Ctrl Pts',(-3.26564388189759,1.,2.1463680529566));
#43024=CARTESIAN_POINT('Ctrl Pts',(-3.27050245897228,1.,2.15205043199808));
#43025=CARTESIAN_POINT('Ctrl Pts',(-3.27534954469187,1.,2.15778690038347));
#43026=CARTESIAN_POINT('Ctrl Pts',(-3.280181508414,1.,2.16357391934425));
#43027=CARTESIAN_POINT('Ctrl Pts',(-3.28499019979724,1.,2.16940517773455));
#43028=CARTESIAN_POINT('Ctrl Pts',(-3.28976645712568,1.,2.17527380048423));
#43029=CARTESIAN_POINT('Ctrl Pts',(-3.2945036150049,1.,2.18117455557065));
#43030=CARTESIAN_POINT('Ctrl Pts',(-3.29920022557639,1.,2.18710556500327));
#43031=CARTESIAN_POINT('Ctrl Pts',(-3.30385816281831,1.,2.19306710376111));
#43032=CARTESIAN_POINT('Ctrl Pts',(-3.30848134694595,1.,2.19906078949923));
#43033=CARTESIAN_POINT('Ctrl Pts',(-3.31307424608949,1.,2.20508863150607));
#43034=CARTESIAN_POINT('Ctrl Pts',(-3.31764044024235,1.,2.21115211847875));
#43035=CARTESIAN_POINT('Ctrl Pts',(-3.32218125618968,1.,2.21725135110898));
#43036=CARTESIAN_POINT('Ctrl Pts',(-3.3266964672289,1.,2.22338548312772));
#43037=CARTESIAN_POINT('Ctrl Pts',(-3.33118487773611,1.,2.22955308907233));
#43038=CARTESIAN_POINT('Ctrl Pts',(-3.33564495756482,1.,2.23575256328812));
#43039=CARTESIAN_POINT('Ctrl Pts',(-3.34007543738025,1.,2.24198249391422));
#43040=CARTESIAN_POINT('Ctrl Pts',(-3.34447596770723,1.,2.24824207678256));
#43041=CARTESIAN_POINT('Ctrl Pts',(-3.34884690292285,1.,2.25453097693483));
#43042=CARTESIAN_POINT('Ctrl Pts',(-3.35318902552626,1.,2.26084915222449));
#43043=CARTESIAN_POINT('Ctrl Pts',(-3.35750328523061,1.,2.2671966857991));
#43044=CARTESIAN_POINT('Ctrl Pts',(-3.36179055004409,1.,2.2735736262093));
#43045=CARTESIAN_POINT('Ctrl Pts',(-3.36605130713076,1.,2.27997979458037));
#43046=CARTESIAN_POINT('Ctrl Pts',(-3.37028570206488,1.,2.28641481081137));
#43047=CARTESIAN_POINT('Ctrl Pts',(-3.37449367172826,1.,2.29287818007393));
#43048=CARTESIAN_POINT('Ctrl Pts',(-3.37867504959433,1.,2.29936936127624));
#43049=CARTESIAN_POINT('Ctrl Pts',(-3.3828296733661,1.,2.30588783640343));
#43050=CARTESIAN_POINT('Ctrl Pts',(-3.38695751492462,1.,2.31243319489367));
#43051=CARTESIAN_POINT('Ctrl Pts',(-3.39105869474822,1.,2.31900513925424));
#43052=CARTESIAN_POINT('Ctrl Pts',(-3.39513342019756,1.,2.3256034390248));
#43053=CARTESIAN_POINT('Ctrl Pts',(-3.39918194577956,1.,2.33222789882489));
#43054=CARTESIAN_POINT('Ctrl Pts',(-3.40320452776743,1.,2.33887832342782));
#43055=CARTESIAN_POINT('Ctrl Pts',(-3.40720137404297,1.,2.34555447649188));
#43056=CARTESIAN_POINT('Ctrl Pts',(-3.41117262314119,1.,2.35225606824109));
#43057=CARTESIAN_POINT('Ctrl Pts',(-3.41511836751469,1.,2.35898278606946));
#43058=CARTESIAN_POINT('Ctrl Pts',(-3.41903866635852,1.,2.36573431470642));
#43059=CARTESIAN_POINT('Ctrl Pts',(-3.42293356216511,1.,2.37251035954292));
#43060=CARTESIAN_POINT('Ctrl Pts',(-3.42680309754399,1.,2.37931067028926));
#43061=CARTESIAN_POINT('Ctrl Pts',(-3.4306473271292,1.,2.38613505843552));
#43062=CARTESIAN_POINT('Ctrl Pts',(-3.4344663067854,1.,2.39298338804493));
#43063=CARTESIAN_POINT('Ctrl Pts',(-3.43750133064416,1.,2.39848113410292));
#43064=CARTESIAN_POINT('Ctrl Pts',(-3.43976627484234,1.,2.40261515589405));
#43065=CARTESIAN_POINT('Ctrl Pts',(-3.44127120683039,1.,2.4053759295909));
#43066=CARTESIAN_POINT('Ctrl Pts',(-3.44202241512147,1.,2.40675750623143));
#43067=CARTESIAN_POINT('Origin',(-3.44202241512147,0.,2.40675750623143));
#43068=CARTESIAN_POINT('',(-3.35260583073571,1.,2.52982887637028));
#43069=CARTESIAN_POINT('Origin',(0.,0.,0.));
#43070=CARTESIAN_POINT('',(-3.24413672884812,1.,1.88097764062697));
#43071=CARTESIAN_POINT('Origin',(0.,1.,0.));
#43072=CARTESIAN_POINT('Ctrl Pts',(-3.24413672884812,1.,1.88097764062697));
#43073=CARTESIAN_POINT('Ctrl Pts',(-3.24413672884812,0.666666666666667,
1.88097764062697));
#43074=CARTESIAN_POINT('Ctrl Pts',(-3.24413672884812,0.333333333333333,
1.88097764062697));
#43075=CARTESIAN_POINT('Ctrl Pts',(-3.24413672884812,-0.333333333333333,
1.88097764062697));
#43076=CARTESIAN_POINT('Ctrl Pts',(-3.24413672884812,-0.666666666666667,
1.88097764062697));
#43077=CARTESIAN_POINT('Ctrl Pts',(-3.24413672884812,-1.,1.88097764062697));
#43078=CARTESIAN_POINT('Ctrl Pts',(-3.70708211654725,-1.,1.97421938526992));
#43079=CARTESIAN_POINT('Ctrl Pts',(-3.70708211654725,1.,1.97421938526992));
#43080=CARTESIAN_POINT('Ctrl Pts',(-3.70551008132332,-1.,1.97417727645308));
#43081=CARTESIAN_POINT('Ctrl Pts',(-3.70551008132332,1.,1.97417727645308));
#43082=CARTESIAN_POINT('Ctrl Pts',(-3.70236698912904,-1.,1.97408973726715));
#43083=CARTESIAN_POINT('Ctrl Pts',(-3.70236698912904,1.,1.97408973726715));
#43084=CARTESIAN_POINT('Ctrl Pts',(-3.6976552856004,-1.,1.97394846383216));
#43085=CARTESIAN_POINT('Ctrl Pts',(-3.6976552856004,1.,1.97394846383216));
#43086=CARTESIAN_POINT('Ctrl Pts',(-3.69137888599902,-1.,1.97374016225483));
#43087=CARTESIAN_POINT('Ctrl Pts',(-3.69137888599902,1.,1.97374016225483));
#43088=CARTESIAN_POINT('Ctrl Pts',(-3.68354319915092,-1.,1.97344650304519));
#43089=CARTESIAN_POINT('Ctrl Pts',(-3.68354319915092,1.,1.97344650304519));
#43090=CARTESIAN_POINT('Ctrl Pts',(-3.67571738107084,-1.,1.97311947678516));
#43091=CARTESIAN_POINT('Ctrl Pts',(-3.67571738107084,1.,1.97311947678516));
#43092=CARTESIAN_POINT('Ctrl Pts',(-3.66790152752075,-1.,1.97275897198678));
#43093=CARTESIAN_POINT('Ctrl Pts',(-3.66790152752075,1.,1.97275897198678));
#43094=CARTESIAN_POINT('Ctrl Pts',(-3.6600957816636,-1.,1.9723648543905));
#43095=CARTESIAN_POINT('Ctrl Pts',(-3.6600957816636,1.,1.9723648543905));
#43096=CARTESIAN_POINT('Ctrl Pts',(-3.652300347166,-1.,1.9719369724024));
#43097=CARTESIAN_POINT('Ctrl Pts',(-3.652300347166,1.,1.9719369724024));
#43098=CARTESIAN_POINT('Ctrl Pts',(-3.64451546723514,-1.,1.97147515441164));
#43099=CARTESIAN_POINT('Ctrl Pts',(-3.64451546723514,1.,1.97147515441164));
#43100=CARTESIAN_POINT('Ctrl Pts',(-3.63674139590412,-1.,1.97097920454464));
#43101=CARTESIAN_POINT('Ctrl Pts',(-3.63674139590412,1.,1.97097920454464));
#43102=CARTESIAN_POINT('Ctrl Pts',(-3.62897836973293,-1.,1.97044889850463));
#43103=CARTESIAN_POINT('Ctrl Pts',(-3.62897836973293,1.,1.97044889850463));
#43104=CARTESIAN_POINT('Ctrl Pts',(-3.62122658401893,-1.,1.96988398129978));
#43105=CARTESIAN_POINT('Ctrl Pts',(-3.62122658401893,1.,1.96988398129978));
#43106=CARTESIAN_POINT('Ctrl Pts',(-3.61348615496704,-1.,1.96928416040877));
#43107=CARTESIAN_POINT('Ctrl Pts',(-3.61348615496704,1.,1.96928416040877));
#43108=CARTESIAN_POINT('Ctrl Pts',(-3.60575714017989,-1.,1.9686491188594));
#43109=CARTESIAN_POINT('Ctrl Pts',(-3.60575714017989,1.,1.9686491188594));
#43110=CARTESIAN_POINT('Ctrl Pts',(-3.59803959819938,-1.,1.96797854118369));
#43111=CARTESIAN_POINT('Ctrl Pts',(-3.59803959819938,1.,1.96797854118369));
#43112=CARTESIAN_POINT('Ctrl Pts',(-3.59033364022801,-1.,1.96727213799544));
#43113=CARTESIAN_POINT('Ctrl Pts',(-3.59033364022801,1.,1.96727213799544));
#43114=CARTESIAN_POINT('Ctrl Pts',(-3.58263947663829,-1.,1.96652966688911));
#43115=CARTESIAN_POINT('Ctrl Pts',(-3.58263947663829,1.,1.96652966688911));
#43116=CARTESIAN_POINT('Ctrl Pts',(-3.57495748600959,-1.,1.96575096652789));
#43117=CARTESIAN_POINT('Ctrl Pts',(-3.57495748600959,1.,1.96575096652789));
#43118=CARTESIAN_POINT('Ctrl Pts',(-3.56728820357791,-1.,1.96493594634567));
#43119=CARTESIAN_POINT('Ctrl Pts',(-3.56728820357791,1.,1.96493594634567));
#43120=CARTESIAN_POINT('Ctrl Pts',(-3.55963218706096,-1.,1.96408450906812));
#43121=CARTESIAN_POINT('Ctrl Pts',(-3.55963218706096,1.,1.96408450906812));
#43122=CARTESIAN_POINT('Ctrl Pts',(-3.55198990600886,-1.,1.96319648628644));
#43123=CARTESIAN_POINT('Ctrl Pts',(-3.55198990600886,1.,1.96319648628644));
#43124=CARTESIAN_POINT('Ctrl Pts',(-3.54436163300443,-1.,1.96227157573067));
#43125=CARTESIAN_POINT('Ctrl Pts',(-3.54436163300443,1.,1.96227157573067));
#43126=CARTESIAN_POINT('Ctrl Pts',(-3.53674730625813,-1.,1.96130926212689));
#43127=CARTESIAN_POINT('Ctrl Pts',(-3.53674730625813,1.,1.96130926212689));
#43128=CARTESIAN_POINT('Ctrl Pts',(-3.52914648844351,-1.,1.96030879411566));
#43129=CARTESIAN_POINT('Ctrl Pts',(-3.52914648844351,1.,1.96030879411566));
#43130=CARTESIAN_POINT('Ctrl Pts',(-3.52155867431486,-1.,1.95926936324461));
#43131=CARTESIAN_POINT('Ctrl Pts',(-3.52155867431486,1.,1.95926936324461));
#43132=CARTESIAN_POINT('Ctrl Pts',(-3.51398354617794,-1.,1.95819025316779));
#43133=CARTESIAN_POINT('Ctrl Pts',(-3.51398354617794,1.,1.95819025316779));
#43134=CARTESIAN_POINT('Ctrl Pts',(-3.50642124159909,-1.,1.95707099606511));
#43135=CARTESIAN_POINT('Ctrl Pts',(-3.50642124159909,1.,1.95707099606511));
#43136=CARTESIAN_POINT('Ctrl Pts',(-3.49887263575583,-1.,1.95591153823661));
#43137=CARTESIAN_POINT('Ctrl Pts',(-3.49887263575583,1.,1.95591153823661));
#43138=CARTESIAN_POINT('Ctrl Pts',(-3.49133956289133,-1.,1.95471236969643));
#43139=CARTESIAN_POINT('Ctrl Pts',(-3.49133956289133,1.,1.95471236969643));
#43140=CARTESIAN_POINT('Ctrl Pts',(-3.48382414832634,-1.,1.95347412486308));
#43141=CARTESIAN_POINT('Ctrl Pts',(-3.48382414832634,1.,1.95347412486308));
#43142=CARTESIAN_POINT('Ctrl Pts',(-3.47632820495921,-1.,1.95219722189876));
#43143=CARTESIAN_POINT('Ctrl Pts',(-3.47632820495921,1.,1.95219722189876));
#43144=CARTESIAN_POINT('Ctrl Pts',(-3.46885258974191,-1.,1.95088147859876));
#43145=CARTESIAN_POINT('Ctrl Pts',(-3.46885258974191,1.,1.95088147859876));
#43146=CARTESIAN_POINT('Ctrl Pts',(-3.46139661060962,-1.,1.94952575850197));
#43147=CARTESIAN_POINT('Ctrl Pts',(-3.46139661060962,1.,1.94952575850197));
#43148=CARTESIAN_POINT('Ctrl Pts',(-3.45395731584051,-1.,1.94812754766524));
#43149=CARTESIAN_POINT('Ctrl Pts',(-3.45395731584051,1.,1.94812754766524));
#43150=CARTESIAN_POINT('Ctrl Pts',(-3.44653088665681,-1.,1.94668377715329));
#43151=CARTESIAN_POINT('Ctrl Pts',(-3.44653088665681,1.,1.94668377715329));
#43152=CARTESIAN_POINT('Ctrl Pts',(-3.43911410197687,-1.,1.94519168842879));
#43153=CARTESIAN_POINT('Ctrl Pts',(-3.43911410197687,1.,1.94519168842879));
#43154=CARTESIAN_POINT('Ctrl Pts',(-3.43170586602434,-1.,1.94364973660284));
#43155=CARTESIAN_POINT('Ctrl Pts',(-3.43170586602434,1.,1.94364973660284));
#43156=CARTESIAN_POINT('Ctrl Pts',(-3.42430850941503,-1.,1.94205835913696));
#43157=CARTESIAN_POINT('Ctrl Pts',(-3.42430850941503,1.,1.94205835913696));
#43158=CARTESIAN_POINT('Ctrl Pts',(-3.41692971994096,-1.,1.94042111965246));
#43159=CARTESIAN_POINT('Ctrl Pts',(-3.41692971994096,1.,1.94042111965246));
#43160=CARTESIAN_POINT('Ctrl Pts',(-3.40957978266642,-1.,1.93874306008143));
#43161=CARTESIAN_POINT('Ctrl Pts',(-3.40957978266642,1.,1.93874306008143));
#43162=CARTESIAN_POINT('Ctrl Pts',(-3.40226802104109,-1.,1.93702857723098));
#43163=CARTESIAN_POINT('Ctrl Pts',(-3.40226802104109,1.,1.93702857723098));
#43164=CARTESIAN_POINT('Ctrl Pts',(-3.39499923640795,-1.,1.93527929945985));
#43165=CARTESIAN_POINT('Ctrl Pts',(-3.39499923640795,1.,1.93527929945985));
#43166=CARTESIAN_POINT('Ctrl Pts',(-3.38777076883256,-1.,1.93349233176788));
#43167=CARTESIAN_POINT('Ctrl Pts',(-3.38777076883256,1.,1.93349233176788));
#43168=CARTESIAN_POINT('Ctrl Pts',(-3.3805676852555,-1.,1.93165739093276));
#43169=CARTESIAN_POINT('Ctrl Pts',(-3.3805676852555,1.,1.93165739093276));
#43170=CARTESIAN_POINT('Ctrl Pts',(-3.37336807068043,-1.,1.92975993109877));
#43171=CARTESIAN_POINT('Ctrl Pts',(-3.37336807068043,1.,1.92975993109877));
#43172=CARTESIAN_POINT('Ctrl Pts',(-3.36615168657567,-1.,1.92778626543786));
#43173=CARTESIAN_POINT('Ctrl Pts',(-3.36615168657567,1.,1.92778626543786));
#43174=CARTESIAN_POINT('Ctrl Pts',(-3.35890824422965,-1.,1.92572846125756));
#43175=CARTESIAN_POINT('Ctrl Pts',(-3.35890824422965,1.,1.92572846125756));
#43176=CARTESIAN_POINT('Ctrl Pts',(-3.35164424847223,-1.,1.92358838440528));
#43177=CARTESIAN_POINT('Ctrl Pts',(-3.35164424847223,1.,1.92358838440528));
#43178=CARTESIAN_POINT('Ctrl Pts',(-3.34439448941961,-1.,1.92138450828404));
#43179=CARTESIAN_POINT('Ctrl Pts',(-3.34439448941961,1.,1.92138450828404));
#43180=CARTESIAN_POINT('Ctrl Pts',(-3.33721230710012,-1.,1.9191460961021));
#43181=CARTESIAN_POINT('Ctrl Pts',(-3.33721230710012,1.,1.9191460961021));
#43182=CARTESIAN_POINT('Ctrl Pts',(-3.33014884257873,-1.,1.91690081930331));
#43183=CARTESIAN_POINT('Ctrl Pts',(-3.33014884257873,1.,1.91690081930331));
#43184=CARTESIAN_POINT('Ctrl Pts',(-3.32323403454535,-1.,1.91466343916628));
#43185=CARTESIAN_POINT('Ctrl Pts',(-3.32323403454535,1.,1.91466343916628));
#43186=CARTESIAN_POINT('Ctrl Pts',(-3.31646052426364,-1.,1.91242616234442));
#43187=CARTESIAN_POINT('Ctrl Pts',(-3.31646052426364,1.,1.91242616234442));
#43188=CARTESIAN_POINT('Ctrl Pts',(-3.30975721158596,-1.,1.91014297830446));
#43189=CARTESIAN_POINT('Ctrl Pts',(-3.30975721158596,1.,1.91014297830446));
#43190=CARTESIAN_POINT('Ctrl Pts',(-3.30300595568195,-1.,1.90773912171341));
#43191=CARTESIAN_POINT('Ctrl Pts',(-3.30300595568195,1.,1.90773912171341));
#43192=CARTESIAN_POINT('Ctrl Pts',(-3.29608978722113,-1.,1.90513891864087));
#43193=CARTESIAN_POINT('Ctrl Pts',(-3.29608978722113,1.,1.90513891864087));
#43194=CARTESIAN_POINT('Ctrl Pts',(-3.2889344860029,-1.,1.90228971247527));
#43195=CARTESIAN_POINT('Ctrl Pts',(-3.2889344860029,1.,1.90228971247527));
#43196=CARTESIAN_POINT('Ctrl Pts',(-3.28154737912352,-1.,1.89918429230462));
#43197=CARTESIAN_POINT('Ctrl Pts',(-3.28154737912352,1.,1.89918429230462));
#43198=CARTESIAN_POINT('Ctrl Pts',(-3.27407108933139,-1.,1.89589172903793));
#43199=CARTESIAN_POINT('Ctrl Pts',(-3.27407108933139,1.,1.89589172903793));
#43200=CARTESIAN_POINT('Ctrl Pts',(-3.26677653888676,-1.,1.89255393500965));
#43201=CARTESIAN_POINT('Ctrl Pts',(-3.26677653888676,1.,1.89255393500965));
#43202=CARTESIAN_POINT('Ctrl Pts',(-3.25999885193947,-1.,1.88934996203698));
#43203=CARTESIAN_POINT('Ctrl Pts',(-3.25999885193947,1.,1.88934996203698));
#43204=CARTESIAN_POINT('Ctrl Pts',(-3.25408686339463,-1.,1.88646802523466));
#43205=CARTESIAN_POINT('Ctrl Pts',(-3.25408686339463,1.,1.88646802523466));
#43206=CARTESIAN_POINT('Ctrl Pts',(-3.24935200511918,-1.,1.88407708646357));
#43207=CARTESIAN_POINT('Ctrl Pts',(-3.24935200511918,1.,1.88407708646357));
#43208=CARTESIAN_POINT('Ctrl Pts',(-3.24600543790443,-1.,1.88229202582941));
#43209=CARTESIAN_POINT('Ctrl Pts',(-3.24600543790443,1.,1.88229202582941));
#43210=CARTESIAN_POINT('Ctrl Pts',(-3.24451807186481,-1.,1.88139187908074));
#43211=CARTESIAN_POINT('Ctrl Pts',(-3.24451807186481,1.,1.88139187908074));
#43212=CARTESIAN_POINT('Ctrl Pts',(-3.24408699284121,-1.,1.88102201872555));
#43213=CARTESIAN_POINT('Ctrl Pts',(-3.24408699284121,1.,1.88102201872555));
#43214=CARTESIAN_POINT('Ctrl Pts',(-3.24410359189609,-1.,1.88091100680349));
#43215=CARTESIAN_POINT('Ctrl Pts',(-3.24410359189609,1.,1.88091100680349));
#43216=CARTESIAN_POINT('Ctrl Pts',(-3.24418789321065,-1.,1.8808893942881));
#43217=CARTESIAN_POINT('Ctrl Pts',(-3.24418789321065,1.,1.8808893942881));
#43218=CARTESIAN_POINT('',(-3.70708211654725,1.,1.97421938526992));
#43219=CARTESIAN_POINT('Ctrl Pts',(-3.70708211654725,1.,1.97421938526992));
#43220=CARTESIAN_POINT('Ctrl Pts',(-3.70551008132332,1.,1.97417727645308));
#43221=CARTESIAN_POINT('Ctrl Pts',(-3.70236698912904,1.,1.97408973726715));
#43222=CARTESIAN_POINT('Ctrl Pts',(-3.6976552856004,1.,1.97394846383216));
#43223=CARTESIAN_POINT('Ctrl Pts',(-3.69137888599902,1.,1.97374016225483));
#43224=CARTESIAN_POINT('Ctrl Pts',(-3.68354319915092,1.,1.97344650304519));
#43225=CARTESIAN_POINT('Ctrl Pts',(-3.67571738107084,1.,1.97311947678516));
#43226=CARTESIAN_POINT('Ctrl Pts',(-3.66790152752075,1.,1.97275897198678));
#43227=CARTESIAN_POINT('Ctrl Pts',(-3.6600957816636,1.,1.9723648543905));
#43228=CARTESIAN_POINT('Ctrl Pts',(-3.652300347166,1.,1.9719369724024));
#43229=CARTESIAN_POINT('Ctrl Pts',(-3.64451546723514,1.,1.97147515441164));
#43230=CARTESIAN_POINT('Ctrl Pts',(-3.63674139590412,1.,1.97097920454464));
#43231=CARTESIAN_POINT('Ctrl Pts',(-3.62897836973293,1.,1.97044889850463));
#43232=CARTESIAN_POINT('Ctrl Pts',(-3.62122658401893,1.,1.96988398129978));
#43233=CARTESIAN_POINT('Ctrl Pts',(-3.61348615496704,1.,1.96928416040877));
#43234=CARTESIAN_POINT('Ctrl Pts',(-3.60575714017989,1.,1.9686491188594));
#43235=CARTESIAN_POINT('Ctrl Pts',(-3.59803959819938,1.,1.96797854118369));
#43236=CARTESIAN_POINT('Ctrl Pts',(-3.59033364022801,1.,1.96727213799544));
#43237=CARTESIAN_POINT('Ctrl Pts',(-3.58263947663829,1.,1.96652966688911));
#43238=CARTESIAN_POINT('Ctrl Pts',(-3.57495748600959,1.,1.96575096652789));
#43239=CARTESIAN_POINT('Ctrl Pts',(-3.56728820357791,1.,1.96493594634567));
#43240=CARTESIAN_POINT('Ctrl Pts',(-3.55963218706096,1.,1.96408450906812));
#43241=CARTESIAN_POINT('Ctrl Pts',(-3.55198990600886,1.,1.96319648628644));
#43242=CARTESIAN_POINT('Ctrl Pts',(-3.54436163300443,1.,1.96227157573067));
#43243=CARTESIAN_POINT('Ctrl Pts',(-3.53674730625813,1.,1.96130926212689));
#43244=CARTESIAN_POINT('Ctrl Pts',(-3.52914648844351,1.,1.96030879411566));
#43245=CARTESIAN_POINT('Ctrl Pts',(-3.52155867431486,1.,1.95926936324461));
#43246=CARTESIAN_POINT('Ctrl Pts',(-3.51398354617794,1.,1.95819025316779));
#43247=CARTESIAN_POINT('Ctrl Pts',(-3.50642124159909,1.,1.95707099606511));
#43248=CARTESIAN_POINT('Ctrl Pts',(-3.49887263575583,1.,1.95591153823661));
#43249=CARTESIAN_POINT('Ctrl Pts',(-3.49133956289133,1.,1.95471236969643));
#43250=CARTESIAN_POINT('Ctrl Pts',(-3.48382414832634,1.,1.95347412486308));
#43251=CARTESIAN_POINT('Ctrl Pts',(-3.47632820495921,1.,1.95219722189876));
#43252=CARTESIAN_POINT('Ctrl Pts',(-3.46885258974191,1.,1.95088147859876));
#43253=CARTESIAN_POINT('Ctrl Pts',(-3.46139661060962,1.,1.94952575850197));
#43254=CARTESIAN_POINT('Ctrl Pts',(-3.45395731584051,1.,1.94812754766524));
#43255=CARTESIAN_POINT('Ctrl Pts',(-3.44653088665681,1.,1.94668377715329));
#43256=CARTESIAN_POINT('Ctrl Pts',(-3.43911410197687,1.,1.94519168842879));
#43257=CARTESIAN_POINT('Ctrl Pts',(-3.43170586602434,1.,1.94364973660284));
#43258=CARTESIAN_POINT('Ctrl Pts',(-3.42430850941503,1.,1.94205835913696));
#43259=CARTESIAN_POINT('Ctrl Pts',(-3.41692971994096,1.,1.94042111965246));
#43260=CARTESIAN_POINT('Ctrl Pts',(-3.40957978266642,1.,1.93874306008143));
#43261=CARTESIAN_POINT('Ctrl Pts',(-3.40226802104109,1.,1.93702857723098));
#43262=CARTESIAN_POINT('Ctrl Pts',(-3.39499923640795,1.,1.93527929945985));
#43263=CARTESIAN_POINT('Ctrl Pts',(-3.38777076883256,1.,1.93349233176788));
#43264=CARTESIAN_POINT('Ctrl Pts',(-3.3805676852555,1.,1.93165739093276));
#43265=CARTESIAN_POINT('Ctrl Pts',(-3.37336807068043,1.,1.92975993109877));
#43266=CARTESIAN_POINT('Ctrl Pts',(-3.36615168657567,1.,1.92778626543786));
#43267=CARTESIAN_POINT('Ctrl Pts',(-3.35890824422965,1.,1.92572846125756));
#43268=CARTESIAN_POINT('Ctrl Pts',(-3.35164424847223,1.,1.92358838440528));
#43269=CARTESIAN_POINT('Ctrl Pts',(-3.34439448941961,1.,1.92138450828404));
#43270=CARTESIAN_POINT('Ctrl Pts',(-3.33721230710012,1.,1.9191460961021));
#43271=CARTESIAN_POINT('Ctrl Pts',(-3.33014884257873,1.,1.91690081930331));
#43272=CARTESIAN_POINT('Ctrl Pts',(-3.32323403454535,1.,1.91466343916628));
#43273=CARTESIAN_POINT('Ctrl Pts',(-3.31646052426364,1.,1.91242616234442));
#43274=CARTESIAN_POINT('Ctrl Pts',(-3.30975721158596,1.,1.91014297830446));
#43275=CARTESIAN_POINT('Ctrl Pts',(-3.30300595568195,1.,1.90773912171341));
#43276=CARTESIAN_POINT('Ctrl Pts',(-3.29608978722113,1.,1.90513891864087));
#43277=CARTESIAN_POINT('Ctrl Pts',(-3.2889344860029,1.,1.90228971247527));
#43278=CARTESIAN_POINT('Ctrl Pts',(-3.28154737912352,1.,1.89918429230462));
#43279=CARTESIAN_POINT('Ctrl Pts',(-3.27407108933139,1.,1.89589172903793));
#43280=CARTESIAN_POINT('Ctrl Pts',(-3.26677653888676,1.,1.89255393500965));
#43281=CARTESIAN_POINT('Ctrl Pts',(-3.25999885193947,1.,1.88934996203698));
#43282=CARTESIAN_POINT('Ctrl Pts',(-3.25408686339463,1.,1.88646802523466));
#43283=CARTESIAN_POINT('Ctrl Pts',(-3.24935200511918,1.,1.88407708646357));
#43284=CARTESIAN_POINT('Ctrl Pts',(-3.2462565441079,1.,1.88242596600454));
#43285=CARTESIAN_POINT('Ctrl Pts',(-3.24480754676064,1.,1.88156537699203));
#43286=CARTESIAN_POINT('Ctrl Pts',(-3.24428080353022,1.,1.88117508446775));
#43287=CARTESIAN_POINT('Ctrl Pts',(-3.24415531671284,1.,1.8810229239812));
#43288=CARTESIAN_POINT('Ctrl Pts',(-3.24413672884812,1.,1.88097764062697));
#43289=CARTESIAN_POINT('',(-3.70708211654725,0.,1.97421938526992));
#43290=CARTESIAN_POINT('Ctrl Pts',(-3.42855728381368,-1.,1.519044091397));
#43291=CARTESIAN_POINT('Ctrl Pts',(-3.42855728381368,1.,1.519044091397));
#43292=CARTESIAN_POINT('Ctrl Pts',(-3.42852521763778,-1.,1.51896318668366));
#43293=CARTESIAN_POINT('Ctrl Pts',(-3.42852521763778,1.,1.51896318668366));
#43294=CARTESIAN_POINT('Ctrl Pts',(-3.42860527149177,-1.,1.51888450659652));
#43295=CARTESIAN_POINT('Ctrl Pts',(-3.42860527149177,1.,1.51888450659652));
#43296=CARTESIAN_POINT('Ctrl Pts',(-3.42915787669893,-1.,1.51901585839109));
#43297=CARTESIAN_POINT('Ctrl Pts',(-3.42915787669893,1.,1.51901585839109));
#43298=CARTESIAN_POINT('Ctrl Pts',(-3.43076036253837,-1.,1.51969006980999));
#43299=CARTESIAN_POINT('Ctrl Pts',(-3.43076036253837,1.,1.51969006980999));
#43300=CARTESIAN_POINT('Ctrl Pts',(-3.43417156977893,-1.,1.52134826724292));
#43301=CARTESIAN_POINT('Ctrl Pts',(-3.43417156977893,1.,1.52134826724292));
#43302=CARTESIAN_POINT('Ctrl Pts',(-3.4388889597401,-1.,1.5237734895035));
#43303=CARTESIAN_POINT('Ctrl Pts',(-3.4388889597401,1.,1.5237734895035));
#43304=CARTESIAN_POINT('Ctrl Pts',(-3.44469547526647,-1.,1.52686242875556));
#43305=CARTESIAN_POINT('Ctrl Pts',(-3.44469547526647,1.,1.52686242875556));
#43306=CARTESIAN_POINT('Ctrl Pts',(-3.45127136828305,-1.,1.53046244461635));
#43307=CARTESIAN_POINT('Ctrl Pts',(-3.45127136828305,1.,1.53046244461635));
#43308=CARTESIAN_POINT('Ctrl Pts',(-3.45825932955032,-1.,1.53440195378792));
#43309=CARTESIAN_POINT('Ctrl Pts',(-3.45825932955032,1.,1.53440195378792));
#43310=CARTESIAN_POINT('Ctrl Pts',(-3.46531752207153,-1.,1.53851507915502));
#43311=CARTESIAN_POINT('Ctrl Pts',(-3.46531752207153,1.,1.53851507915502));
#43312=CARTESIAN_POINT('Ctrl Pts',(-3.47217189224653,-1.,1.54266605398187));
#43313=CARTESIAN_POINT('Ctrl Pts',(-3.47217189224653,1.,1.54266605398187));
#43314=CARTESIAN_POINT('Ctrl Pts',(-3.47868272898751,-1.,1.54678009290276));
#43315=CARTESIAN_POINT('Ctrl Pts',(-3.47868272898751,1.,1.54678009290276));
#43316=CARTESIAN_POINT('Ctrl Pts',(-3.48485155928567,-1.,1.55084702970452));
#43317=CARTESIAN_POINT('Ctrl Pts',(-3.48485155928567,1.,1.55084702970452));
#43318=CARTESIAN_POINT('Ctrl Pts',(-3.4907646087742,-1.,1.55489595901116));
#43319=CARTESIAN_POINT('Ctrl Pts',(-3.4907646087742,1.,1.55489595901116));
#43320=CARTESIAN_POINT('Ctrl Pts',(-3.49655185179655,-1.,1.55897703097874));
#43321=CARTESIAN_POINT('Ctrl Pts',(-3.49655185179655,1.,1.55897703097874));
#43322=CARTESIAN_POINT('Ctrl Pts',(-3.50234321621578,-1.,1.56314187758675));
#43323=CARTESIAN_POINT('Ctrl Pts',(-3.50234321621578,1.,1.56314187758675));
#43324=CARTESIAN_POINT('Ctrl Pts',(-3.50821771695363,-1.,1.56742097575012));
#43325=CARTESIAN_POINT('Ctrl Pts',(-3.50821771695363,1.,1.56742097575012));
#43326=CARTESIAN_POINT('Ctrl Pts',(-3.51418598431665,-1.,1.57181569799743));
#43327=CARTESIAN_POINT('Ctrl Pts',(-3.51418598431665,1.,1.57181569799743));
#43328=CARTESIAN_POINT('Ctrl Pts',(-3.52021847865912,-1.,1.57631049988158));
#43329=CARTESIAN_POINT('Ctrl Pts',(-3.52021847865912,1.,1.57631049988158));
#43330=CARTESIAN_POINT('Ctrl Pts',(-3.52626275334881,-1.,1.58088027227848));
#43331=CARTESIAN_POINT('Ctrl Pts',(-3.52626275334881,1.,1.58088027227848));
#43332=CARTESIAN_POINT('Ctrl Pts',(-3.5322637814708,-1.,1.58549906268088));
#43333=CARTESIAN_POINT('Ctrl Pts',(-3.5322637814708,1.,1.58549906268088));
#43334=CARTESIAN_POINT('Ctrl Pts',(-3.53818616861077,-1.,1.59014958368739));
#43335=CARTESIAN_POINT('Ctrl Pts',(-3.53818616861077,1.,1.59014958368739));
#43336=CARTESIAN_POINT('Ctrl Pts',(-3.54402458182337,-1.,1.59482766949766));
#43337=CARTESIAN_POINT('Ctrl Pts',(-3.54402458182337,1.,1.59482766949766));
#43338=CARTESIAN_POINT('Ctrl Pts',(-3.54979148634454,-1.,1.59953698113457));
#43339=CARTESIAN_POINT('Ctrl Pts',(-3.54979148634454,1.,1.59953698113457));
#43340=CARTESIAN_POINT('Ctrl Pts',(-3.55550985096129,-1.,1.60428584699853));
#43341=CARTESIAN_POINT('Ctrl Pts',(-3.55550985096129,1.,1.60428584699853));
#43342=CARTESIAN_POINT('Ctrl Pts',(-3.5612043248298,-1.,1.60908344685457));
#43343=CARTESIAN_POINT('Ctrl Pts',(-3.5612043248298,1.,1.60908344685457));
#43344=CARTESIAN_POINT('Ctrl Pts',(-3.56689200468387,-1.,1.61393581747514));
#43345=CARTESIAN_POINT('Ctrl Pts',(-3.56689200468387,1.,1.61393581747514));
#43346=CARTESIAN_POINT('Ctrl Pts',(-3.57257679609806,-1.,1.61884340915404));
#43347=CARTESIAN_POINT('Ctrl Pts',(-3.57257679609806,1.,1.61884340915404));
#43348=CARTESIAN_POINT('Ctrl Pts',(-3.5782545595439,-1.,1.62380329464844));
#43349=CARTESIAN_POINT('Ctrl Pts',(-3.5782545595439,1.,1.62380329464844));
#43350=CARTESIAN_POINT('Ctrl Pts',(-3.58391625774343,-1.,1.62881051550745));
#43351=CARTESIAN_POINT('Ctrl Pts',(-3.58391625774343,1.,1.62881051550745));
#43352=CARTESIAN_POINT('Ctrl Pts',(-3.58955176627879,-1.,1.6338597145126));
#43353=CARTESIAN_POINT('Ctrl Pts',(-3.58955176627879,1.,1.6338597145126));
#43354=CARTESIAN_POINT('Ctrl Pts',(-3.59515368334893,-1.,1.63894676675352));
#43355=CARTESIAN_POINT('Ctrl Pts',(-3.59515368334893,1.,1.63894676675352));
#43356=CARTESIAN_POINT('Ctrl Pts',(-3.60072028513845,-1.,1.64407004385582));
#43357=CARTESIAN_POINT('Ctrl Pts',(-3.60072028513845,1.,1.64407004385582));
#43358=CARTESIAN_POINT('Ctrl Pts',(-3.60625346556992,-1.,1.64922952425832));
#43359=CARTESIAN_POINT('Ctrl Pts',(-3.60625346556992,1.,1.64922952425832));
#43360=CARTESIAN_POINT('Ctrl Pts',(-3.61175734965127,-1.,1.65442619244325));
#43361=CARTESIAN_POINT('Ctrl Pts',(-3.61175734965127,1.,1.65442619244325));
#43362=CARTESIAN_POINT('Ctrl Pts',(-3.61723666482456,-1.,1.65966133399186));
#43363=CARTESIAN_POINT('Ctrl Pts',(-3.61723666482456,1.,1.65966133399186));
#43364=CARTESIAN_POINT('Ctrl Pts',(-3.62269517989109,-1.,1.66493585923855));
#43365=CARTESIAN_POINT('Ctrl Pts',(-3.62269517989109,1.,1.66493585923855));
#43366=CARTESIAN_POINT('Ctrl Pts',(-3.62813422105271,-1.,1.67024966008045));
#43367=CARTESIAN_POINT('Ctrl Pts',(-3.62813422105271,1.,1.67024966008045));
#43368=CARTESIAN_POINT('Ctrl Pts',(-3.63355343201232,-1.,1.67560193613156));
#43369=CARTESIAN_POINT('Ctrl Pts',(-3.63355343201232,1.,1.67560193613156));
#43370=CARTESIAN_POINT('Ctrl Pts',(-3.63895140887462,-1.,1.68099146651586));
#43371=CARTESIAN_POINT('Ctrl Pts',(-3.63895140887462,1.,1.68099146651586));
#43372=CARTESIAN_POINT('Ctrl Pts',(-3.64432638915203,-1.,1.68641690471457));
#43373=CARTESIAN_POINT('Ctrl Pts',(-3.64432638915203,1.,1.68641690471457));
#43374=CARTESIAN_POINT('Ctrl Pts',(-3.64967689827371,-1.,1.69187705481689));
#43375=CARTESIAN_POINT('Ctrl Pts',(-3.64967689827371,1.,1.69187705481689));
#43376=CARTESIAN_POINT('Ctrl Pts',(-3.65500246526749,-1.,1.69737117722534));
#43377=CARTESIAN_POINT('Ctrl Pts',(-3.65500246526749,1.,1.69737117722534));
#43378=CARTESIAN_POINT('Ctrl Pts',(-3.66030338774847,-1.,1.70289888566873));
#43379=CARTESIAN_POINT('Ctrl Pts',(-3.66030338774847,1.,1.70289888566873));
#43380=CARTESIAN_POINT('Ctrl Pts',(-3.66558043198876,-1.,1.70846001610956));
#43381=CARTESIAN_POINT('Ctrl Pts',(-3.66558043198876,1.,1.70846001610956));
#43382=CARTESIAN_POINT('Ctrl Pts',(-3.67083454901611,-1.,1.71405450210383));
#43383=CARTESIAN_POINT('Ctrl Pts',(-3.67083454901611,1.,1.71405450210383));
#43384=CARTESIAN_POINT('Ctrl Pts',(-3.67606660374709,-1.,1.71968225581808));
#43385=CARTESIAN_POINT('Ctrl Pts',(-3.67606660374709,1.,1.71968225581808));
#43386=CARTESIAN_POINT('Ctrl Pts',(-3.68127704936579,-1.,1.72534302437056));
#43387=CARTESIAN_POINT('Ctrl Pts',(-3.68127704936579,1.,1.72534302437056));
#43388=CARTESIAN_POINT('Ctrl Pts',(-3.68646597019332,-1.,1.73103640956717));
#43389=CARTESIAN_POINT('Ctrl Pts',(-3.68646597019332,1.,1.73103640956717));
#43390=CARTESIAN_POINT('Ctrl Pts',(-3.69163322648036,-1.,1.73676193254557));
#43391=CARTESIAN_POINT('Ctrl Pts',(-3.69163322648036,1.,1.73676193254557));
#43392=CARTESIAN_POINT('Ctrl Pts',(-3.69677856910517,-1.,1.74251908492617));
#43393=CARTESIAN_POINT('Ctrl Pts',(-3.69677856910517,1.,1.74251908492617));
#43394=CARTESIAN_POINT('Ctrl Pts',(-3.7019017567335,-1.,1.74830738046057));
#43395=CARTESIAN_POINT('Ctrl Pts',(-3.7019017567335,1.,1.74830738046057));
#43396=CARTESIAN_POINT('Ctrl Pts',(-3.70700269736659,-1.,1.75412641804042));
#43397=CARTESIAN_POINT('Ctrl Pts',(-3.70700269736659,1.,1.75412641804042));
#43398=CARTESIAN_POINT('Ctrl Pts',(-3.71208146346136,-1.,1.75997588498865));
#43399=CARTESIAN_POINT('Ctrl Pts',(-3.71208146346136,1.,1.75997588498865));
#43400=CARTESIAN_POINT('Ctrl Pts',(-3.71713822377359,-1.,1.76585552124394));
#43401=CARTESIAN_POINT('Ctrl Pts',(-3.71713822377359,1.,1.76585552124394));
#43402=CARTESIAN_POINT('Ctrl Pts',(-3.72217319911254,-1.,1.77176509401761));
#43403=CARTESIAN_POINT('Ctrl Pts',(-3.72217319911254,1.,1.77176509401761));
#43404=CARTESIAN_POINT('Ctrl Pts',(-3.72718661205609,-1.,1.77770437039658));
#43405=CARTESIAN_POINT('Ctrl Pts',(-3.72718661205609,1.,1.77770437039658));
#43406=CARTESIAN_POINT('Ctrl Pts',(-3.7321786309547,-1.,1.78367308442901));
#43407=CARTESIAN_POINT('Ctrl Pts',(-3.7321786309547,1.,1.78367308442901));
#43408=CARTESIAN_POINT('Ctrl Pts',(-3.73714934730681,-1.,1.78967092823491));
#43409=CARTESIAN_POINT('Ctrl Pts',(-3.73714934730681,1.,1.78967092823491));
#43410=CARTESIAN_POINT('Ctrl Pts',(-3.74209880352445,-1.,1.79569757859422));
#43411=CARTESIAN_POINT('Ctrl Pts',(-3.74209880352445,1.,1.79569757859422));
#43412=CARTESIAN_POINT('Ctrl Pts',(-3.74702700875467,-1.,1.8017527148577));
#43413=CARTESIAN_POINT('Ctrl Pts',(-3.74702700875467,1.,1.8017527148577));
#43414=CARTESIAN_POINT('Ctrl Pts',(-3.75193395887977,-1.,1.80783603939617));
#43415=CARTESIAN_POINT('Ctrl Pts',(-3.75193395887977,1.,1.80783603939617));
#43416=CARTESIAN_POINT('Ctrl Pts',(-3.75681965683071,-1.,1.8139472983358));
#43417=CARTESIAN_POINT('Ctrl Pts',(-3.75681965683071,1.,1.8139472983358));
#43418=CARTESIAN_POINT('Ctrl Pts',(-3.76168412707948,-1.,1.82008629694091));
#43419=CARTESIAN_POINT('Ctrl Pts',(-3.76168412707948,1.,1.82008629694091));
#43420=CARTESIAN_POINT('Ctrl Pts',(-3.76652740353775,-1.,1.82625289220915));
#43421=CARTESIAN_POINT('Ctrl Pts',(-3.76652740353775,1.,1.82625289220915));
#43422=CARTESIAN_POINT('Ctrl Pts',(-3.77038509817999,-1.,1.83120816955645));
#43423=CARTESIAN_POINT('Ctrl Pts',(-3.77038509817999,1.,1.83120816955645));
#43424=CARTESIAN_POINT('Ctrl Pts',(-3.77326886064398,-1.,1.83493697934534));
#43425=CARTESIAN_POINT('Ctrl Pts',(-3.77326886064398,1.,1.83493697934534));
#43426=CARTESIAN_POINT('Ctrl Pts',(-3.77518714457833,-1.,1.83742834010626));
#43427=CARTESIAN_POINT('Ctrl Pts',(-3.77518714457833,1.,1.83742834010626));
#43428=CARTESIAN_POINT('Ctrl Pts',(-3.77614523045147,-1.,1.8386753923786));
#43429=CARTESIAN_POINT('Ctrl Pts',(-3.77614523045147,1.,1.8386753923786));
#43430=CARTESIAN_POINT('',(-3.42859860294306,1.,1.5189508286633));
#43431=CARTESIAN_POINT('Ctrl Pts',(-3.42859860294306,-1.,1.5189508286633));
#43432=CARTESIAN_POINT('Ctrl Pts',(-3.42859860294306,-0.666666666666667,
1.5189508286633));
#43433=CARTESIAN_POINT('Ctrl Pts',(-3.42859860294306,-0.333333333333333,
1.5189508286633));
#43434=CARTESIAN_POINT('Ctrl Pts',(-3.42859860294306,0.333333333333333,
1.5189508286633));
#43435=CARTESIAN_POINT('Ctrl Pts',(-3.42859860294306,0.666666666666667,
1.5189508286633));
#43436=CARTESIAN_POINT('Ctrl Pts',(-3.42859860294306,1.,1.5189508286633));
#43437=CARTESIAN_POINT('',(-3.77614523045147,1.,1.8386753923786));
#43438=CARTESIAN_POINT('',(-3.77614523045147,0.,1.8386753923786));
#43439=CARTESIAN_POINT('Ctrl Pts',(-3.42859860294306,1.,1.5189508286633));
#43440=CARTESIAN_POINT('Ctrl Pts',(-3.42864616361875,1.,1.51893924967331));
#43441=CARTESIAN_POINT('Ctrl Pts',(-3.42884302333841,1.,1.5189513329503));
#43442=CARTESIAN_POINT('Ctrl Pts',(-3.42946838852587,1.,1.51914806898491));
#43443=CARTESIAN_POINT('Ctrl Pts',(-3.43101631893414,1.,1.5198144909338));
#43444=CARTESIAN_POINT('Ctrl Pts',(-3.43417156977893,1.,1.52134826724292));
#43445=CARTESIAN_POINT('Ctrl Pts',(-3.4388889597401,1.,1.5237734895035));
#43446=CARTESIAN_POINT('Ctrl Pts',(-3.44469547526647,1.,1.52686242875556));
#43447=CARTESIAN_POINT('Ctrl Pts',(-3.45127136828305,1.,1.53046244461635));
#43448=CARTESIAN_POINT('Ctrl Pts',(-3.45825932955032,1.,1.53440195378792));
#43449=CARTESIAN_POINT('Ctrl Pts',(-3.46531752207153,1.,1.53851507915502));
#43450=CARTESIAN_POINT('Ctrl Pts',(-3.47217189224653,1.,1.54266605398187));
#43451=CARTESIAN_POINT('Ctrl Pts',(-3.47868272898751,1.,1.54678009290276));
#43452=CARTESIAN_POINT('Ctrl Pts',(-3.48485155928567,1.,1.55084702970452));
#43453=CARTESIAN_POINT('Ctrl Pts',(-3.4907646087742,1.,1.55489595901116));
#43454=CARTESIAN_POINT('Ctrl Pts',(-3.49655185179655,1.,1.55897703097874));
#43455=CARTESIAN_POINT('Ctrl Pts',(-3.50234321621578,1.,1.56314187758675));
#43456=CARTESIAN_POINT('Ctrl Pts',(-3.50821771695363,1.,1.56742097575012));
#43457=CARTESIAN_POINT('Ctrl Pts',(-3.51418598431665,1.,1.57181569799743));
#43458=CARTESIAN_POINT('Ctrl Pts',(-3.52021847865912,1.,1.57631049988158));
#43459=CARTESIAN_POINT('Ctrl Pts',(-3.52626275334881,1.,1.58088027227848));
#43460=CARTESIAN_POINT('Ctrl Pts',(-3.5322637814708,1.,1.58549906268088));
#43461=CARTESIAN_POINT('Ctrl Pts',(-3.53818616861077,1.,1.59014958368739));
#43462=CARTESIAN_POINT('Ctrl Pts',(-3.54402458182337,1.,1.59482766949766));
#43463=CARTESIAN_POINT('Ctrl Pts',(-3.54979148634454,1.,1.59953698113457));
#43464=CARTESIAN_POINT('Ctrl Pts',(-3.55550985096129,1.,1.60428584699853));
#43465=CARTESIAN_POINT('Ctrl Pts',(-3.5612043248298,1.,1.60908344685457));
#43466=CARTESIAN_POINT('Ctrl Pts',(-3.56689200468387,1.,1.61393581747514));
#43467=CARTESIAN_POINT('Ctrl Pts',(-3.57257679609806,1.,1.61884340915404));
#43468=CARTESIAN_POINT('Ctrl Pts',(-3.5782545595439,1.,1.62380329464844));
#43469=CARTESIAN_POINT('Ctrl Pts',(-3.58391625774343,1.,1.62881051550745));
#43470=CARTESIAN_POINT('Ctrl Pts',(-3.58955176627879,1.,1.6338597145126));
#43471=CARTESIAN_POINT('Ctrl Pts',(-3.59515368334893,1.,1.63894676675352));
#43472=CARTESIAN_POINT('Ctrl Pts',(-3.60072028513845,1.,1.64407004385582));
#43473=CARTESIAN_POINT('Ctrl Pts',(-3.60625346556992,1.,1.64922952425832));
#43474=CARTESIAN_POINT('Ctrl Pts',(-3.61175734965127,1.,1.65442619244325));
#43475=CARTESIAN_POINT('Ctrl Pts',(-3.61723666482456,1.,1.65966133399186));
#43476=CARTESIAN_POINT('Ctrl Pts',(-3.62269517989109,1.,1.66493585923855));
#43477=CARTESIAN_POINT('Ctrl Pts',(-3.62813422105271,1.,1.67024966008045));
#43478=CARTESIAN_POINT('Ctrl Pts',(-3.63355343201232,1.,1.67560193613156));
#43479=CARTESIAN_POINT('Ctrl Pts',(-3.63895140887462,1.,1.68099146651586));
#43480=CARTESIAN_POINT('Ctrl Pts',(-3.64432638915203,1.,1.68641690471457));
#43481=CARTESIAN_POINT('Ctrl Pts',(-3.64967689827371,1.,1.69187705481689));
#43482=CARTESIAN_POINT('Ctrl Pts',(-3.65500246526749,1.,1.69737117722534));
#43483=CARTESIAN_POINT('Ctrl Pts',(-3.66030338774847,1.,1.70289888566873));
#43484=CARTESIAN_POINT('Ctrl Pts',(-3.66558043198876,1.,1.70846001610956));
#43485=CARTESIAN_POINT('Ctrl Pts',(-3.67083454901611,1.,1.71405450210383));
#43486=CARTESIAN_POINT('Ctrl Pts',(-3.67606660374709,1.,1.71968225581808));
#43487=CARTESIAN_POINT('Ctrl Pts',(-3.68127704936579,1.,1.72534302437056));
#43488=CARTESIAN_POINT('Ctrl Pts',(-3.68646597019332,1.,1.73103640956717));
#43489=CARTESIAN_POINT('Ctrl Pts',(-3.69163322648036,1.,1.73676193254557));
#43490=CARTESIAN_POINT('Ctrl Pts',(-3.69677856910517,1.,1.74251908492617));
#43491=CARTESIAN_POINT('Ctrl Pts',(-3.7019017567335,1.,1.74830738046057));
#43492=CARTESIAN_POINT('Ctrl Pts',(-3.70700269736659,1.,1.75412641804042));
#43493=CARTESIAN_POINT('Ctrl Pts',(-3.71208146346136,1.,1.75997588498865));
#43494=CARTESIAN_POINT('Ctrl Pts',(-3.71713822377359,1.,1.76585552124394));
#43495=CARTESIAN_POINT('Ctrl Pts',(-3.72217319911254,1.,1.77176509401761));
#43496=CARTESIAN_POINT('Ctrl Pts',(-3.72718661205609,1.,1.77770437039658));
#43497=CARTESIAN_POINT('Ctrl Pts',(-3.7321786309547,1.,1.78367308442901));
#43498=CARTESIAN_POINT('Ctrl Pts',(-3.73714934730681,1.,1.78967092823491));
#43499=CARTESIAN_POINT('Ctrl Pts',(-3.74209880352445,1.,1.79569757859422));
#43500=CARTESIAN_POINT('Ctrl Pts',(-3.74702700875467,1.,1.8017527148577));
#43501=CARTESIAN_POINT('Ctrl Pts',(-3.75193395887977,1.,1.80783603939617));
#43502=CARTESIAN_POINT('Ctrl Pts',(-3.75681965683071,1.,1.8139472983358));
#43503=CARTESIAN_POINT('Ctrl Pts',(-3.76168412707948,1.,1.82008629694091));
#43504=CARTESIAN_POINT('Ctrl Pts',(-3.76652740353775,1.,1.82625289220915));
#43505=CARTESIAN_POINT('Ctrl Pts',(-3.77038509817999,1.,1.83120816955645));
#43506=CARTESIAN_POINT('Ctrl Pts',(-3.77326886064398,1.,1.83493697934534));
#43507=CARTESIAN_POINT('Ctrl Pts',(-3.77518714457833,1.,1.83742834010626));
#43508=CARTESIAN_POINT('Ctrl Pts',(-3.77614523045147,1.,1.8386753923786));
#43509=CARTESIAN_POINT('Origin',(-3.77614523045147,0.,1.8386753923786));
#43510=CARTESIAN_POINT('',(-3.70708211654725,1.,1.97421938526992));
#43511=CARTESIAN_POINT('Origin',(0.,0.,0.));
#43512=CARTESIAN_POINT('',(-3.49844575334386,1.,1.35032489087269));
#43513=CARTESIAN_POINT('Origin',(0.,1.,0.));
#43514=CARTESIAN_POINT('Ctrl Pts',(-3.49844575334386,1.,1.35032489087269));
#43515=CARTESIAN_POINT('Ctrl Pts',(-3.49844575334386,0.666666666666667,
1.35032489087269));
#43516=CARTESIAN_POINT('Ctrl Pts',(-3.49844575334386,0.333333333333333,
1.35032489087269));
#43517=CARTESIAN_POINT('Ctrl Pts',(-3.49844575334386,-0.333333333333333,
1.35032489087269));
#43518=CARTESIAN_POINT('Ctrl Pts',(-3.49844575334386,-0.666666666666667,
1.35032489087269));
#43519=CARTESIAN_POINT('Ctrl Pts',(-3.49844575334386,-1.,1.35032489087269));
#43520=CARTESIAN_POINT('Ctrl Pts',(-3.97027773754922,-1.,1.36999806084572));
#43521=CARTESIAN_POINT('Ctrl Pts',(-3.97027773754922,1.,1.36999806084572));
#43522=CARTESIAN_POINT('Ctrl Pts',(-3.9687184694173,-1.,1.37020239094758));
#43523=CARTESIAN_POINT('Ctrl Pts',(-3.9687184694173,1.,1.37020239094758));
#43524=CARTESIAN_POINT('Ctrl Pts',(-3.96560037975788,-1.,1.37060761746027));
#43525=CARTESIAN_POINT('Ctrl Pts',(-3.96560037975788,1.,1.37060761746027));
#43526=CARTESIAN_POINT('Ctrl Pts',(-3.96092458508407,-1.,1.37120515615663));
#43527=CARTESIAN_POINT('Ctrl Pts',(-3.96092458508407,1.,1.37120515615663));
#43528=CARTESIAN_POINT('Ctrl Pts',(-3.95469287283105,-1.,1.37198126433139));
#43529=CARTESIAN_POINT('Ctrl Pts',(-3.95469287283105,1.,1.37198126433139));
#43530=CARTESIAN_POINT('Ctrl Pts',(-3.94690771786926,-1.,1.37291699203423));
#43531=CARTESIAN_POINT('Ctrl Pts',(-3.94690771786926,1.,1.37291699203423));
#43532=CARTESIAN_POINT('Ctrl Pts',(-3.93912709041791,-1.,1.37381821967499));
#43533=CARTESIAN_POINT('Ctrl Pts',(-3.93912709041791,1.,1.37381821967499));
#43534=CARTESIAN_POINT('Ctrl Pts',(-3.93135106761941,-1.,1.37468482215784));
#43535=CARTESIAN_POINT('Ctrl Pts',(-3.93135106761941,1.,1.37468482215784));
#43536=CARTESIAN_POINT('Ctrl Pts',(-3.92357976987132,-1.,1.37551664448057));
#43537=CARTESIAN_POINT('Ctrl Pts',(-3.92357976987132,1.,1.37551664448057));
#43538=CARTESIAN_POINT('Ctrl Pts',(-3.91581337461825,-1.,1.37631350505516));
#43539=CARTESIAN_POINT('Ctrl Pts',(-3.91581337461825,1.,1.37631350505516));
#43540=CARTESIAN_POINT('Ctrl Pts',(-3.90805209522729,-1.,1.3770751963376));
#43541=CARTESIAN_POINT('Ctrl Pts',(-3.90805209522729,1.,1.3770751963376));
#43542=CARTESIAN_POINT('Ctrl Pts',(-3.90029615196255,-1.,1.3778014851263));
#43543=CARTESIAN_POINT('Ctrl Pts',(-3.90029615196255,1.,1.3778014851263));
#43544=CARTESIAN_POINT('Ctrl Pts',(-3.89254574338385,-1.,1.37849211287981));
#43545=CARTESIAN_POINT('Ctrl Pts',(-3.89254574338385,1.,1.37849211287981));
#43546=CARTESIAN_POINT('Ctrl Pts',(-3.88480102249461,-1.,1.37914679719446));
#43547=CARTESIAN_POINT('Ctrl Pts',(-3.88480102249461,1.,1.37914679719446));
#43548=CARTESIAN_POINT('Ctrl Pts',(-3.87706205830865,-1.,1.37976523097187));
#43549=CARTESIAN_POINT('Ctrl Pts',(-3.87706205830865,1.,1.37976523097187));
#43550=CARTESIAN_POINT('Ctrl Pts',(-3.86932885813403,-1.,1.38034709213129));
#43551=CARTESIAN_POINT('Ctrl Pts',(-3.86932885813403,1.,1.38034709213129));
#43552=CARTESIAN_POINT('Ctrl Pts',(-3.86160143044187,-1.,1.38089205993067));
#43553=CARTESIAN_POINT('Ctrl Pts',(-3.86160143044187,1.,1.38089205993067));
#43554=CARTESIAN_POINT('Ctrl Pts',(-3.85387983979557,-1.,1.38139983115075));
#43555=CARTESIAN_POINT('Ctrl Pts',(-3.85387983979557,1.,1.38139983115075));
#43556=CARTESIAN_POINT('Ctrl Pts',(-3.84616425605705,-1.,1.38187013346089));
#43557=CARTESIAN_POINT('Ctrl Pts',(-3.84616425605705,1.,1.38187013346089));
#43558=CARTESIAN_POINT('Ctrl Pts',(-3.83845502790609,-1.,1.38230274828774));
#43559=CARTESIAN_POINT('Ctrl Pts',(-3.83845502790609,1.,1.38230274828774));
#43560=CARTESIAN_POINT('Ctrl Pts',(-3.83075266982138,-1.,1.38269750245086));
#43561=CARTESIAN_POINT('Ctrl Pts',(-3.83075266982138,1.,1.38269750245086));
#43562=CARTESIAN_POINT('Ctrl Pts',(-3.82305771743715,-1.,1.38305421262724));
#43563=CARTESIAN_POINT('Ctrl Pts',(-3.82305771743715,1.,1.38305421262724));
#43564=CARTESIAN_POINT('Ctrl Pts',(-3.81537060817765,-1.,1.38337263902766));
#43565=CARTESIAN_POINT('Ctrl Pts',(-3.81537060817765,1.,1.38337263902766));
#43566=CARTESIAN_POINT('Ctrl Pts',(-3.80769156398429,-1.,1.38365244046226));
#43567=CARTESIAN_POINT('Ctrl Pts',(-3.80769156398429,1.,1.38365244046226));
#43568=CARTESIAN_POINT('Ctrl Pts',(-3.80002044322169,-1.,1.38389311766701));
#43569=CARTESIAN_POINT('Ctrl Pts',(-3.80002044322169,1.,1.38389311766701));
#43570=CARTESIAN_POINT('Ctrl Pts',(-3.79235669640907,-1.,1.38409399694588));
#43571=CARTESIAN_POINT('Ctrl Pts',(-3.79235669640907,1.,1.38409399694588));
#43572=CARTESIAN_POINT('Ctrl Pts',(-3.78469969805134,-1.,1.38425435883773));
#43573=CARTESIAN_POINT('Ctrl Pts',(-3.78469969805134,1.,1.38425435883773));
#43574=CARTESIAN_POINT('Ctrl Pts',(-3.77704902230441,-1.,1.38437354551435));
#43575=CARTESIAN_POINT('Ctrl Pts',(-3.77704902230441,1.,1.38437354551435));
#43576=CARTESIAN_POINT('Ctrl Pts',(-3.76940473185775,-1.,1.38445107339517));
#43577=CARTESIAN_POINT('Ctrl Pts',(-3.76940473185775,1.,1.38445107339517));
#43578=CARTESIAN_POINT('Ctrl Pts',(-3.76176768271347,-1.,1.38448675253343));
#43579=CARTESIAN_POINT('Ctrl Pts',(-3.76176768271347,1.,1.38448675253343));
#43580=CARTESIAN_POINT('Ctrl Pts',(-3.75413976318727,-1.,1.38448077997155));
#43581=CARTESIAN_POINT('Ctrl Pts',(-3.75413976318727,1.,1.38448077997155));
#43582=CARTESIAN_POINT('Ctrl Pts',(-3.7465231716786,-1.,1.38443344984389));
#43583=CARTESIAN_POINT('Ctrl Pts',(-3.7465231716786,1.,1.38443344984389));
#43584=CARTESIAN_POINT('Ctrl Pts',(-3.73891976418099,-1.,1.38434489156456));
#43585=CARTESIAN_POINT('Ctrl Pts',(-3.73891976418099,1.,1.38434489156456));
#43586=CARTESIAN_POINT('Ctrl Pts',(-3.73133035859283,-1.,1.38421479111531));
#43587=CARTESIAN_POINT('Ctrl Pts',(-3.73133035859283,1.,1.38421479111531));
#43588=CARTESIAN_POINT('Ctrl Pts',(-3.72375409358805,-1.,1.3840421342895));
#43589=CARTESIAN_POINT('Ctrl Pts',(-3.72375409358805,1.,1.3840421342895));
#43590=CARTESIAN_POINT('Ctrl Pts',(-3.7161876605181,-1.,1.38382489984585));
#43591=CARTESIAN_POINT('Ctrl Pts',(-3.7161876605181,1.,1.38382489984585));
#43592=CARTESIAN_POINT('Ctrl Pts',(-3.70862680753343,-1.,1.38356065402122));
#43593=CARTESIAN_POINT('Ctrl Pts',(-3.70862680753343,1.,1.38356065402122));
#43594=CARTESIAN_POINT('Ctrl Pts',(-3.70106792167894,-1.,1.38324717612862));
#43595=CARTESIAN_POINT('Ctrl Pts',(-3.70106792167894,1.,1.38324717612862));
#43596=CARTESIAN_POINT('Ctrl Pts',(-3.69350967899523,-1.,1.38288311171649));
#43597=CARTESIAN_POINT('Ctrl Pts',(-3.69350967899523,1.,1.38288311171649));
#43598=CARTESIAN_POINT('Ctrl Pts',(-3.68595444983844,-1.,1.38246852827185));
#43599=CARTESIAN_POINT('Ctrl Pts',(-3.68595444983844,1.,1.38246852827185));
#43600=CARTESIAN_POINT('Ctrl Pts',(-3.6784103848243,-1.,1.38200574290626));
#43601=CARTESIAN_POINT('Ctrl Pts',(-3.6784103848243,1.,1.38200574290626));
#43602=CARTESIAN_POINT('Ctrl Pts',(-3.67088843112282,-1.,1.38149812653876));
#43603=CARTESIAN_POINT('Ctrl Pts',(-3.67088843112282,1.,1.38149812653876));
#43604=CARTESIAN_POINT('Ctrl Pts',(-3.66339848520874,-1.,1.38094856333558));
#43605=CARTESIAN_POINT('Ctrl Pts',(-3.66339848520874,1.,1.38094856333558));
#43606=CARTESIAN_POINT('Ctrl Pts',(-3.65594554404396,-1.,1.38035791051215));
#43607=CARTESIAN_POINT('Ctrl Pts',(-3.65594554404396,1.,1.38035791051215));
#43608=CARTESIAN_POINT('Ctrl Pts',(-3.64852652756444,-1.,1.37972372481598));
#43609=CARTESIAN_POINT('Ctrl Pts',(-3.64852652756444,1.,1.37972372481598));
#43610=CARTESIAN_POINT('Ctrl Pts',(-3.64112507791112,-1.,1.37903818567347));
#43611=CARTESIAN_POINT('Ctrl Pts',(-3.64112507791112,1.,1.37903818567347));
#43612=CARTESIAN_POINT('Ctrl Pts',(-3.63371727442448,-1.,1.37829035457324));
#43613=CARTESIAN_POINT('Ctrl Pts',(-3.63371727442448,1.,1.37829035457324));
#43614=CARTESIAN_POINT('Ctrl Pts',(-3.62628098665112,-1.,1.37746987919868));
#43615=CARTESIAN_POINT('Ctrl Pts',(-3.62628098665112,1.,1.37746987919868));
#43616=CARTESIAN_POINT('Ctrl Pts',(-3.61880481160408,-1.,1.37657053403102));
#43617=CARTESIAN_POINT('Ctrl Pts',(-3.61880481160408,1.,1.37657053403102));
#43618=CARTESIAN_POINT('Ctrl Pts',(-3.61129546591082,-1.,1.37559314436641));
#43619=CARTESIAN_POINT('Ctrl Pts',(-3.61129546591082,1.,1.37559314436641));
#43620=CARTESIAN_POINT('Ctrl Pts',(-3.60379020124038,-1.,1.37455051379642));
#43621=CARTESIAN_POINT('Ctrl Pts',(-3.60379020124038,1.,1.37455051379642));
#43622=CARTESIAN_POINT('Ctrl Pts',(-3.59634627869117,-1.,1.37346320103184));
#43623=CARTESIAN_POINT('Ctrl Pts',(-3.59634627869117,1.,1.37346320103184));
#43624=CARTESIAN_POINT('Ctrl Pts',(-3.5890185384643,-1.,1.37235053661));
#43625=CARTESIAN_POINT('Ctrl Pts',(-3.5890185384643,1.,1.37235053661));
#43626=CARTESIAN_POINT('Ctrl Pts',(-3.58183885982745,-1.,1.37122241663073));
#43627=CARTESIAN_POINT('Ctrl Pts',(-3.58183885982745,1.,1.37122241663073));
#43628=CARTESIAN_POINT('Ctrl Pts',(-3.57479875549453,-1.,1.37007229485646));
#43629=CARTESIAN_POINT('Ctrl Pts',(-3.57479875549453,1.,1.37007229485646));
#43630=CARTESIAN_POINT('Ctrl Pts',(-3.56782080304554,-1.,1.36886584973349));
#43631=CARTESIAN_POINT('Ctrl Pts',(-3.56782080304554,1.,1.36886584973349));
#43632=CARTESIAN_POINT('Ctrl Pts',(-3.56077662028492,-1.,1.36754771771174));
#43633=CARTESIAN_POINT('Ctrl Pts',(-3.56077662028492,1.,1.36754771771174));
#43634=CARTESIAN_POINT('Ctrl Pts',(-3.55353883995793,-1.,1.36606145456711));
#43635=CARTESIAN_POINT('Ctrl Pts',(-3.55353883995793,1.,1.36606145456711));
#43636=CARTESIAN_POINT('Ctrl Pts',(-3.54602591832893,-1.,1.36436666257567));
#43637=CARTESIAN_POINT('Ctrl Pts',(-3.54602591832893,1.,1.36436666257567));
#43638=CARTESIAN_POINT('Ctrl Pts',(-3.53824396425032,-1.,1.36245507339334));
#43639=CARTESIAN_POINT('Ctrl Pts',(-3.53824396425032,1.,1.36245507339334));
#43640=CARTESIAN_POINT('Ctrl Pts',(-3.53034464961849,-1.,1.36037259643827));
#43641=CARTESIAN_POINT('Ctrl Pts',(-3.53034464961849,1.,1.36037259643827));
#43642=CARTESIAN_POINT('Ctrl Pts',(-3.52261776117121,-1.,1.35821701528975));
#43643=CARTESIAN_POINT('Ctrl Pts',(-3.52261776117121,1.,1.35821701528975));
#43644=CARTESIAN_POINT('Ctrl Pts',(-3.51542230699919,-1.,1.35611275237288));
#43645=CARTESIAN_POINT('Ctrl Pts',(-3.51542230699919,1.,1.35611275237288));
#43646=CARTESIAN_POINT('Ctrl Pts',(-3.50913227060177,-1.,1.35419113576022));
#43647=CARTESIAN_POINT('Ctrl Pts',(-3.50913227060177,1.,1.35419113576022));
#43648=CARTESIAN_POINT('Ctrl Pts',(-3.50408168106113,-1.,1.3525703284343));
#43649=CARTESIAN_POINT('Ctrl Pts',(-3.50408168106113,1.,1.3525703284343));
#43650=CARTESIAN_POINT('Ctrl Pts',(-3.50049707063673,-1.,1.35133076331065));
#43651=CARTESIAN_POINT('Ctrl Pts',(-3.50049707063673,1.,1.35133076331065));
#43652=CARTESIAN_POINT('Ctrl Pts',(-3.49888720256612,-1.,1.35067437417289));
#43653=CARTESIAN_POINT('Ctrl Pts',(-3.49888720256612,1.,1.35067437417289));
#43654=CARTESIAN_POINT('Ctrl Pts',(-3.49840357193384,-1.,1.35037650302887));
#43655=CARTESIAN_POINT('Ctrl Pts',(-3.49840357193384,1.,1.35037650302887));
#43656=CARTESIAN_POINT('Ctrl Pts',(-3.49840260053616,-1.,1.35026426118351));
#43657=CARTESIAN_POINT('Ctrl Pts',(-3.49840260053616,1.,1.35026426118351));
#43658=CARTESIAN_POINT('Ctrl Pts',(-3.49848248301936,-1.,1.35022972712301));
#43659=CARTESIAN_POINT('Ctrl Pts',(-3.49848248301936,1.,1.35022972712301));
#43660=CARTESIAN_POINT('',(-3.97027773754922,1.,1.36999806084572));
#43661=CARTESIAN_POINT('Ctrl Pts',(-3.97027773754922,1.,1.36999806084572));
#43662=CARTESIAN_POINT('Ctrl Pts',(-3.9687184694173,1.,1.37020239094758));
#43663=CARTESIAN_POINT('Ctrl Pts',(-3.96560037975788,1.,1.37060761746027));
#43664=CARTESIAN_POINT('Ctrl Pts',(-3.96092458508407,1.,1.37120515615663));
#43665=CARTESIAN_POINT('Ctrl Pts',(-3.95469287283105,1.,1.37198126433139));
#43666=CARTESIAN_POINT('Ctrl Pts',(-3.94690771786926,1.,1.37291699203423));
#43667=CARTESIAN_POINT('Ctrl Pts',(-3.93912709041791,1.,1.37381821967499));
#43668=CARTESIAN_POINT('Ctrl Pts',(-3.93135106761941,1.,1.37468482215784));
#43669=CARTESIAN_POINT('Ctrl Pts',(-3.92357976987132,1.,1.37551664448057));
#43670=CARTESIAN_POINT('Ctrl Pts',(-3.91581337461825,1.,1.37631350505516));
#43671=CARTESIAN_POINT('Ctrl Pts',(-3.90805209522729,1.,1.3770751963376));
#43672=CARTESIAN_POINT('Ctrl Pts',(-3.90029615196255,1.,1.3778014851263));
#43673=CARTESIAN_POINT('Ctrl Pts',(-3.89254574338385,1.,1.37849211287981));
#43674=CARTESIAN_POINT('Ctrl Pts',(-3.88480102249461,1.,1.37914679719446));
#43675=CARTESIAN_POINT('Ctrl Pts',(-3.87706205830865,1.,1.37976523097187));
#43676=CARTESIAN_POINT('Ctrl Pts',(-3.86932885813403,1.,1.38034709213129));
#43677=CARTESIAN_POINT('Ctrl Pts',(-3.86160143044187,1.,1.38089205993067));
#43678=CARTESIAN_POINT('Ctrl Pts',(-3.85387983979557,1.,1.38139983115075));
#43679=CARTESIAN_POINT('Ctrl Pts',(-3.84616425605705,1.,1.38187013346089));
#43680=CARTESIAN_POINT('Ctrl Pts',(-3.83845502790609,1.,1.38230274828774));
#43681=CARTESIAN_POINT('Ctrl Pts',(-3.83075266982138,1.,1.38269750245086));
#43682=CARTESIAN_POINT('Ctrl Pts',(-3.82305771743715,1.,1.38305421262724));
#43683=CARTESIAN_POINT('Ctrl Pts',(-3.81537060817765,1.,1.38337263902766));
#43684=CARTESIAN_POINT('Ctrl Pts',(-3.80769156398429,1.,1.38365244046226));
#43685=CARTESIAN_POINT('Ctrl Pts',(-3.80002044322169,1.,1.38389311766701));
#43686=CARTESIAN_POINT('Ctrl Pts',(-3.79235669640907,1.,1.38409399694588));
#43687=CARTESIAN_POINT('Ctrl Pts',(-3.78469969805134,1.,1.38425435883773));
#43688=CARTESIAN_POINT('Ctrl Pts',(-3.77704902230441,1.,1.38437354551435));
#43689=CARTESIAN_POINT('Ctrl Pts',(-3.76940473185775,1.,1.38445107339517));
#43690=CARTESIAN_POINT('Ctrl Pts',(-3.76176768271347,1.,1.38448675253343));
#43691=CARTESIAN_POINT('Ctrl Pts',(-3.75413976318727,1.,1.38448077997155));
#43692=CARTESIAN_POINT('Ctrl Pts',(-3.7465231716786,1.,1.38443344984389));
#43693=CARTESIAN_POINT('Ctrl Pts',(-3.73891976418099,1.,1.38434489156456));
#43694=CARTESIAN_POINT('Ctrl Pts',(-3.73133035859283,1.,1.38421479111531));
#43695=CARTESIAN_POINT('Ctrl Pts',(-3.72375409358805,1.,1.3840421342895));
#43696=CARTESIAN_POINT('Ctrl Pts',(-3.7161876605181,1.,1.38382489984585));
#43697=CARTESIAN_POINT('Ctrl Pts',(-3.70862680753343,1.,1.38356065402122));
#43698=CARTESIAN_POINT('Ctrl Pts',(-3.70106792167894,1.,1.38324717612862));
#43699=CARTESIAN_POINT('Ctrl Pts',(-3.69350967899523,1.,1.38288311171649));
#43700=CARTESIAN_POINT('Ctrl Pts',(-3.68595444983844,1.,1.38246852827185));
#43701=CARTESIAN_POINT('Ctrl Pts',(-3.6784103848243,1.,1.38200574290626));
#43702=CARTESIAN_POINT('Ctrl Pts',(-3.67088843112282,1.,1.38149812653876));
#43703=CARTESIAN_POINT('Ctrl Pts',(-3.66339848520874,1.,1.38094856333558));
#43704=CARTESIAN_POINT('Ctrl Pts',(-3.65594554404396,1.,1.38035791051215));
#43705=CARTESIAN_POINT('Ctrl Pts',(-3.64852652756444,1.,1.37972372481598));
#43706=CARTESIAN_POINT('Ctrl Pts',(-3.64112507791112,1.,1.37903818567347));
#43707=CARTESIAN_POINT('Ctrl Pts',(-3.63371727442448,1.,1.37829035457324));
#43708=CARTESIAN_POINT('Ctrl Pts',(-3.62628098665112,1.,1.37746987919868));
#43709=CARTESIAN_POINT('Ctrl Pts',(-3.61880481160408,1.,1.37657053403102));
#43710=CARTESIAN_POINT('Ctrl Pts',(-3.61129546591082,1.,1.37559314436641));
#43711=CARTESIAN_POINT('Ctrl Pts',(-3.60379020124038,1.,1.37455051379642));
#43712=CARTESIAN_POINT('Ctrl Pts',(-3.59634627869117,1.,1.37346320103184));
#43713=CARTESIAN_POINT('Ctrl Pts',(-3.5890185384643,1.,1.37235053661));
#43714=CARTESIAN_POINT('Ctrl Pts',(-3.58183885982745,1.,1.37122241663073));
#43715=CARTESIAN_POINT('Ctrl Pts',(-3.57479875549453,1.,1.37007229485646));
#43716=CARTESIAN_POINT('Ctrl Pts',(-3.56782080304554,1.,1.36886584973349));
#43717=CARTESIAN_POINT('Ctrl Pts',(-3.56077662028492,1.,1.36754771771174));
#43718=CARTESIAN_POINT('Ctrl Pts',(-3.55353883995793,1.,1.36606145456711));
#43719=CARTESIAN_POINT('Ctrl Pts',(-3.54602591832893,1.,1.36436666257567));
#43720=CARTESIAN_POINT('Ctrl Pts',(-3.53824396425032,1.,1.36245507339334));
#43721=CARTESIAN_POINT('Ctrl Pts',(-3.53034464961849,1.,1.36037259643827));
#43722=CARTESIAN_POINT('Ctrl Pts',(-3.52261776117121,1.,1.35821701528975));
#43723=CARTESIAN_POINT('Ctrl Pts',(-3.51542230699919,1.,1.35611275237288));
#43724=CARTESIAN_POINT('Ctrl Pts',(-3.50913227060177,1.,1.35419113576022));
#43725=CARTESIAN_POINT('Ctrl Pts',(-3.50408168106113,1.,1.3525703284343));
#43726=CARTESIAN_POINT('Ctrl Pts',(-3.5007660381658,1.,1.35142377279535));
#43727=CARTESIAN_POINT('Ctrl Pts',(-3.49920025459856,1.,1.35080045218652));
#43728=CARTESIAN_POINT('Ctrl Pts',(-3.49861894124915,1.,1.35049736560633));
#43729=CARTESIAN_POINT('Ctrl Pts',(-3.49847119623841,1.,1.35036670893102));
#43730=CARTESIAN_POINT('Ctrl Pts',(-3.49844575334386,1.,1.35032489087269));
#43731=CARTESIAN_POINT('',(-3.97027773754922,0.,1.36999806084572));
#43732=CARTESIAN_POINT('Ctrl Pts',(-3.62397690409552,-1.,0.96399761336957));
#43733=CARTESIAN_POINT('Ctrl Pts',(-3.62397690409552,1.,0.96399761336957));
#43734=CARTESIAN_POINT('Ctrl Pts',(-3.62393257642191,-1.,0.963922720982576));
#43735=CARTESIAN_POINT('Ctrl Pts',(-3.62393257642191,1.,0.963922720982576));
#43736=CARTESIAN_POINT('Ctrl Pts',(-3.62399933640277,-1.,0.963832486396055));
#43737=CARTESIAN_POINT('Ctrl Pts',(-3.62399933640277,1.,0.963832486396055));
#43738=CARTESIAN_POINT('Ctrl Pts',(-3.62456568607055,-1.,0.963875774532102));
#43739=CARTESIAN_POINT('Ctrl Pts',(-3.62456568607055,1.,0.963875774532102));
#43740=CARTESIAN_POINT('Ctrl Pts',(-3.62625391255277,-1.,0.964291001274618));
#43741=CARTESIAN_POINT('Ctrl Pts',(-3.62625391255277,1.,0.964291001274618));
#43742=CARTESIAN_POINT('Ctrl Pts',(-3.62988252139998,-1.,0.965395153165716));
#43743=CARTESIAN_POINT('Ctrl Pts',(-3.62988252139998,1.,0.965395153165716));
#43744=CARTESIAN_POINT('Ctrl Pts',(-3.6349212208096,-1.,0.967052554540877));
#43745=CARTESIAN_POINT('Ctrl Pts',(-3.6349212208096,1.,0.967052554540877));
#43746=CARTESIAN_POINT('Ctrl Pts',(-3.64113946505393,-1.,0.969195124674829));
#43747=CARTESIAN_POINT('Ctrl Pts',(-3.64113946505393,1.,0.969195124674829));
#43748=CARTESIAN_POINT('Ctrl Pts',(-3.64819756447072,-1.,0.971722122060277));
#43749=CARTESIAN_POINT('Ctrl Pts',(-3.64819756447072,1.,0.971722122060277));
#43750=CARTESIAN_POINT('Ctrl Pts',(-3.6557157673487,-1.,0.974519971354138));
#43751=CARTESIAN_POINT('Ctrl Pts',(-3.6557157673487,1.,0.974519971354138));
#43752=CARTESIAN_POINT('Ctrl Pts',(-3.66333049637403,-1.,0.977478312751416));
#43753=CARTESIAN_POINT('Ctrl Pts',(-3.66333049637403,1.,0.977478312751416));
#43754=CARTESIAN_POINT('Ctrl Pts',(-3.67074983340444,-1.,0.980505922458494));
#43755=CARTESIAN_POINT('Ctrl Pts',(-3.67074983340444,1.,0.980505922458494));
#43756=CARTESIAN_POINT('Ctrl Pts',(-3.67782408841876,-1.,0.983550791470864));
#43757=CARTESIAN_POINT('Ctrl Pts',(-3.67782408841876,1.,0.983550791470864));
#43758=CARTESIAN_POINT('Ctrl Pts',(-3.6845531792623,-1.,0.986602639864285));
#43759=CARTESIAN_POINT('Ctrl Pts',(-3.6845531792623,1.,0.986602639864285));
#43760=CARTESIAN_POINT('Ctrl Pts',(-3.69102682138955,-1.,0.989676715398858));
#43761=CARTESIAN_POINT('Ctrl Pts',(-3.69102682138955,1.,0.989676715398858));
#43762=CARTESIAN_POINT('Ctrl Pts',(-3.69738123415696,-1.,0.992802218332103));
#43763=CARTESIAN_POINT('Ctrl Pts',(-3.69738123415696,1.,0.992802218332103));
#43764=CARTESIAN_POINT('Ctrl Pts',(-3.70375282282107,-1.,0.996009819772431));
#43765=CARTESIAN_POINT('Ctrl Pts',(-3.70375282282107,1.,0.996009819772431));
#43766=CARTESIAN_POINT('Ctrl Pts',(-3.7102243971387,-1.,0.999317260756344));
#43767=CARTESIAN_POINT('Ctrl Pts',(-3.7102243971387,1.,0.999317260756344));
#43768=CARTESIAN_POINT('Ctrl Pts',(-3.71680667125047,-1.,1.00272423396802));
#43769=CARTESIAN_POINT('Ctrl Pts',(-3.71680667125047,1.,1.00272423396802));
#43770=CARTESIAN_POINT('Ctrl Pts',(-3.72346803750544,-1.,1.00622000735696));
#43771=CARTESIAN_POINT('Ctrl Pts',(-3.72346803750544,1.,1.00622000735696));
#43772=CARTESIAN_POINT('Ctrl Pts',(-3.73015276704407,-1.,1.00978798539491));
#43773=CARTESIAN_POINT('Ctrl Pts',(-3.73015276704407,1.,1.00978798539491));
#43774=CARTESIAN_POINT('Ctrl Pts',(-3.73680245055747,-1.,1.01341114319906));
#43775=CARTESIAN_POINT('Ctrl Pts',(-3.73680245055747,1.,1.01341114319906));
#43776=CARTESIAN_POINT('Ctrl Pts',(-3.74337942504993,-1.,1.01707794311088));
#43777=CARTESIAN_POINT('Ctrl Pts',(-3.74337942504993,1.,1.01707794311088));
#43778=CARTESIAN_POINT('Ctrl Pts',(-3.74987777155873,-1.,1.02078510487439));
#43779=CARTESIAN_POINT('Ctrl Pts',(-3.74987777155873,1.,1.02078510487439));
#43780=CARTESIAN_POINT('Ctrl Pts',(-3.75631037456224,-1.,1.02453429444668));
#43781=CARTESIAN_POINT('Ctrl Pts',(-3.75631037456224,1.,1.02453429444668));
#43782=CARTESIAN_POINT('Ctrl Pts',(-3.76270122291245,-1.,1.02833014458184));
#43783=CARTESIAN_POINT('Ctrl Pts',(-3.76270122291245,1.,1.02833014458184));
#43784=CARTESIAN_POINT('Ctrl Pts',(-3.76907609832516,-1.,1.03217786604919));
#43785=CARTESIAN_POINT('Ctrl Pts',(-3.76907609832516,1.,1.03217786604919));
#43786=CARTESIAN_POINT('Ctrl Pts',(-3.77545283140427,-1.,1.03608074678008));
#43787=CARTESIAN_POINT('Ctrl Pts',(-3.77545283140427,1.,1.03608074678008));
#43788=CARTESIAN_POINT('Ctrl Pts',(-3.7818353500817,-1.,1.04003862055798));
#43789=CARTESIAN_POINT('Ctrl Pts',(-3.7818353500817,1.,1.04003862055798));
#43790=CARTESIAN_POINT('Ctrl Pts',(-3.78821910787179,-1.,1.04404924374422));
#43791=CARTESIAN_POINT('Ctrl Pts',(-3.78821910787179,1.,1.04404924374422));
#43792=CARTESIAN_POINT('Ctrl Pts',(-3.79459440308786,-1.,1.04810913267639));
#43793=CARTESIAN_POINT('Ctrl Pts',(-3.79459440308786,1.,1.04810913267639));
#43794=CARTESIAN_POINT('Ctrl Pts',(-3.80095039790681,-1.,1.05221457990016));
#43795=CARTESIAN_POINT('Ctrl Pts',(-3.80095039790681,1.,1.05221457990016));
#43796=CARTESIAN_POINT('Ctrl Pts',(-3.80727913637791,-1.,1.05636266918644));
#43797=CARTESIAN_POINT('Ctrl Pts',(-3.80727913637791,1.,1.05636266918644));
#43798=CARTESIAN_POINT('Ctrl Pts',(-3.8135786611749,-1.,1.06055206187299));
#43799=CARTESIAN_POINT('Ctrl Pts',(-3.8135786611749,1.,1.06055206187299));
#43800=CARTESIAN_POINT('Ctrl Pts',(-3.81985083953012,-1.,1.0647824403893));
#43801=CARTESIAN_POINT('Ctrl Pts',(-3.81985083953012,1.,1.0647824403893));
#43802=CARTESIAN_POINT('Ctrl Pts',(-3.82609989967276,-1.,1.06905413180359));
#43803=CARTESIAN_POINT('Ctrl Pts',(-3.82609989967276,1.,1.06905413180359));
#43804=CARTESIAN_POINT('Ctrl Pts',(-3.83233071195144,-1.,1.07336766633459));
#43805=CARTESIAN_POINT('Ctrl Pts',(-3.83233071195144,1.,1.07336766633459));
#43806=CARTESIAN_POINT('Ctrl Pts',(-3.83854714117491,-1.,1.07772335353858));
#43807=CARTESIAN_POINT('Ctrl Pts',(-3.83854714117491,1.,1.07772335353858));
#43808=CARTESIAN_POINT('Ctrl Pts',(-3.8447504803063,-1.,1.08212087917991));
#43809=CARTESIAN_POINT('Ctrl Pts',(-3.8447504803063,1.,1.08212087917991));
#43810=CARTESIAN_POINT('Ctrl Pts',(-3.85094025222713,-1.,1.08655950846384));
#43811=CARTESIAN_POINT('Ctrl Pts',(-3.85094025222713,1.,1.08655950846384));
#43812=CARTESIAN_POINT('Ctrl Pts',(-3.85711487933931,-1.,1.09103825516294));
#43813=CARTESIAN_POINT('Ctrl Pts',(-3.85711487933931,1.,1.09103825516294));
#43814=CARTESIAN_POINT('Ctrl Pts',(-3.86327241021247,-1.,1.09555606505013));
#43815=CARTESIAN_POINT('Ctrl Pts',(-3.86327241021247,1.,1.09555606505013));
#43816=CARTESIAN_POINT('Ctrl Pts',(-3.86941120134849,-1.,1.10011198761195));
#43817=CARTESIAN_POINT('Ctrl Pts',(-3.86941120134849,1.,1.10011198761195));
#43818=CARTESIAN_POINT('Ctrl Pts',(-3.87553067187514,-1.,1.10470536603287));
#43819=CARTESIAN_POINT('Ctrl Pts',(-3.87553067187514,1.,1.10470536603287));
#43820=CARTESIAN_POINT('Ctrl Pts',(-3.88163105531724,-1.,1.10933577224008));
#43821=CARTESIAN_POINT('Ctrl Pts',(-3.88163105531724,1.,1.10933577224008));
#43822=CARTESIAN_POINT('Ctrl Pts',(-3.88771308285171,-1.,1.11400292434429));
#43823=CARTESIAN_POINT('Ctrl Pts',(-3.88771308285171,1.,1.11400292434429));
#43824=CARTESIAN_POINT('Ctrl Pts',(-3.89377768340344,-1.,1.11870660794603));
#43825=CARTESIAN_POINT('Ctrl Pts',(-3.89377768340344,1.,1.11870660794603));
#43826=CARTESIAN_POINT('Ctrl Pts',(-3.89982569750025,-1.,1.12344660099043));
#43827=CARTESIAN_POINT('Ctrl Pts',(-3.89982569750025,1.,1.12344660099043));
#43828=CARTESIAN_POINT('Ctrl Pts',(-3.90585753318737,-1.,1.12822258281553));
#43829=CARTESIAN_POINT('Ctrl Pts',(-3.90585753318737,1.,1.12822258281553));
#43830=CARTESIAN_POINT('Ctrl Pts',(-3.91187321145649,-1.,1.13303414693896));
#43831=CARTESIAN_POINT('Ctrl Pts',(-3.91187321145649,1.,1.13303414693896));
#43832=CARTESIAN_POINT('Ctrl Pts',(-3.91787251936827,-1.,1.13788084225554));
#43833=CARTESIAN_POINT('Ctrl Pts',(-3.91787251936827,1.,1.13788084225554));
#43834=CARTESIAN_POINT('Ctrl Pts',(-3.92385513133997,-1.,1.14276220561593));
#43835=CARTESIAN_POINT('Ctrl Pts',(-3.92385513133997,1.,1.14276220561593));
#43836=CARTESIAN_POINT('Ctrl Pts',(-3.92982073294257,-1.,1.14767779451123));
#43837=CARTESIAN_POINT('Ctrl Pts',(-3.92982073294257,1.,1.14767779451123));
#43838=CARTESIAN_POINT('Ctrl Pts',(-3.9357691705628,-1.,1.1526272271632));
#43839=CARTESIAN_POINT('Ctrl Pts',(-3.9357691705628,1.,1.1526272271632));
#43840=CARTESIAN_POINT('Ctrl Pts',(-3.94170046685203,-1.,1.15761018340956));
#43841=CARTESIAN_POINT('Ctrl Pts',(-3.94170046685203,1.,1.15761018340956));
#43842=CARTESIAN_POINT('Ctrl Pts',(-3.94761474780583,-1.,1.16262637999157));
#43843=CARTESIAN_POINT('Ctrl Pts',(-3.94761474780583,1.,1.16262637999157));
#43844=CARTESIAN_POINT('Ctrl Pts',(-3.95351219509876,-1.,1.16767555244438));
#43845=CARTESIAN_POINT('Ctrl Pts',(-3.95351219509876,1.,1.16767555244438));
#43846=CARTESIAN_POINT('Ctrl Pts',(-3.95939299213276,-1.,1.17275743590361));
#43847=CARTESIAN_POINT('Ctrl Pts',(-3.95939299213276,1.,1.17275743590361));
#43848=CARTESIAN_POINT('Ctrl Pts',(-3.96525726358159,-1.,1.17787174135592));
#43849=CARTESIAN_POINT('Ctrl Pts',(-3.96525726358159,1.,1.17787174135592));
#43850=CARTESIAN_POINT('Ctrl Pts',(-3.97110505165415,-1.,1.18301815039831));
#43851=CARTESIAN_POINT('Ctrl Pts',(-3.97110505165415,1.,1.18301815039831));
#43852=CARTESIAN_POINT('Ctrl Pts',(-3.97693634767754,-1.,1.18819633715539));
#43853=CARTESIAN_POINT('Ctrl Pts',(-3.97693634767754,1.,1.18819633715539));
#43854=CARTESIAN_POINT('Ctrl Pts',(-3.98275111052561,-1.,1.19340598349475));
#43855=CARTESIAN_POINT('Ctrl Pts',(-3.98275111052561,1.,1.19340598349475));
#43856=CARTESIAN_POINT('Ctrl Pts',(-3.98854928957189,-1.,1.19864679609566));
#43857=CARTESIAN_POINT('Ctrl Pts',(-3.98854928957189,1.,1.19864679609566));
#43858=CARTESIAN_POINT('Ctrl Pts',(-3.99433084799666,-1.,1.20391852375139));
#43859=CARTESIAN_POINT('Ctrl Pts',(-3.99433084799666,1.,1.20391852375139));
#43860=CARTESIAN_POINT('Ctrl Pts',(-4.00009577950721,-1.,1.20922097029551));
#43861=CARTESIAN_POINT('Ctrl Pts',(-4.00009577950721,1.,1.20922097029551));
#43862=CARTESIAN_POINT('Ctrl Pts',(-4.00584409522722,-1.,1.21455398918133));
#43863=CARTESIAN_POINT('Ctrl Pts',(-4.00584409522722,1.,1.21455398918133));
#43864=CARTESIAN_POINT('Ctrl Pts',(-4.01042947140789,-1.,1.21884478244403));
#43865=CARTESIAN_POINT('Ctrl Pts',(-4.01042947140789,1.,1.21884478244403));
#43866=CARTESIAN_POINT('Ctrl Pts',(-4.01386104433519,-1.,1.22207656455845));
#43867=CARTESIAN_POINT('Ctrl Pts',(-4.01386104433519,1.,1.22207656455845));
#43868=CARTESIAN_POINT('Ctrl Pts',(-4.01614544569895,-1.,1.22423716681317));
#43869=CARTESIAN_POINT('Ctrl Pts',(-4.01614544569895,1.,1.22423716681317));
#43870=CARTESIAN_POINT('Ctrl Pts',(-4.01728681790024,-1.,1.22531898815164));
#43871=CARTESIAN_POINT('Ctrl Pts',(-4.01728681790024,1.,1.22531898815164));
#43872=CARTESIAN_POINT('',(-3.62400312501199,1.,0.963899035118986));
#43873=CARTESIAN_POINT('Ctrl Pts',(-3.62400312501199,-1.,0.963899035118986));
#43874=CARTESIAN_POINT('Ctrl Pts',(-3.62400312501199,-0.666666666666667,
0.963899035118986));
#43875=CARTESIAN_POINT('Ctrl Pts',(-3.62400312501199,-0.333333333333333,
0.963899035118986));
#43876=CARTESIAN_POINT('Ctrl Pts',(-3.62400312501199,0.333333333333333,
0.963899035118986));
#43877=CARTESIAN_POINT('Ctrl Pts',(-3.62400312501199,0.666666666666667,
0.963899035118985));
#43878=CARTESIAN_POINT('Ctrl Pts',(-3.62400312501199,1.,0.963899035118985));
#43879=CARTESIAN_POINT('',(-4.01728681790024,1.,1.22531898815164));
#43880=CARTESIAN_POINT('',(-4.01728681790024,0.,1.22531898815164));
#43881=CARTESIAN_POINT('Ctrl Pts',(-3.62400312501199,1.,0.963899035118985));
#43882=CARTESIAN_POINT('Ctrl Pts',(-3.62404828878374,1.,0.963880158556713));
#43883=CARTESIAN_POINT('Ctrl Pts',(-3.62424461507455,1.,0.963861297423579));
#43884=CARTESIAN_POINT('Ctrl Pts',(-3.62489305727516,1.,0.963957782642589));
#43885=CARTESIAN_POINT('Ctrl Pts',(-3.62652618145252,1.,0.964373850166081));
#43886=CARTESIAN_POINT('Ctrl Pts',(-3.62988252139998,1.,0.965395153165716));
#43887=CARTESIAN_POINT('Ctrl Pts',(-3.6349212208096,1.,0.967052554540877));
#43888=CARTESIAN_POINT('Ctrl Pts',(-3.64113946505393,1.,0.969195124674829));
#43889=CARTESIAN_POINT('Ctrl Pts',(-3.64819756447072,1.,0.971722122060277));
#43890=CARTESIAN_POINT('Ctrl Pts',(-3.6557157673487,1.,0.974519971354138));
#43891=CARTESIAN_POINT('Ctrl Pts',(-3.66333049637403,1.,0.977478312751416));
#43892=CARTESIAN_POINT('Ctrl Pts',(-3.67074983340444,1.,0.980505922458494));
#43893=CARTESIAN_POINT('Ctrl Pts',(-3.67782408841876,1.,0.983550791470864));
#43894=CARTESIAN_POINT('Ctrl Pts',(-3.6845531792623,1.,0.986602639864285));
#43895=CARTESIAN_POINT('Ctrl Pts',(-3.69102682138955,1.,0.989676715398858));
#43896=CARTESIAN_POINT('Ctrl Pts',(-3.69738123415696,1.,0.992802218332103));
#43897=CARTESIAN_POINT('Ctrl Pts',(-3.70375282282107,1.,0.996009819772431));
#43898=CARTESIAN_POINT('Ctrl Pts',(-3.7102243971387,1.,0.999317260756344));
#43899=CARTESIAN_POINT('Ctrl Pts',(-3.71680667125047,1.,1.00272423396802));
#43900=CARTESIAN_POINT('Ctrl Pts',(-3.72346803750544,1.,1.00622000735696));
#43901=CARTESIAN_POINT('Ctrl Pts',(-3.73015276704407,1.,1.00978798539491));
#43902=CARTESIAN_POINT('Ctrl Pts',(-3.73680245055747,1.,1.01341114319906));
#43903=CARTESIAN_POINT('Ctrl Pts',(-3.74337942504993,1.,1.01707794311088));
#43904=CARTESIAN_POINT('Ctrl Pts',(-3.74987777155873,1.,1.02078510487439));
#43905=CARTESIAN_POINT('Ctrl Pts',(-3.75631037456224,1.,1.02453429444668));
#43906=CARTESIAN_POINT('Ctrl Pts',(-3.76270122291245,1.,1.02833014458184));
#43907=CARTESIAN_POINT('Ctrl Pts',(-3.76907609832516,1.,1.03217786604919));
#43908=CARTESIAN_POINT('Ctrl Pts',(-3.77545283140427,1.,1.03608074678008));
#43909=CARTESIAN_POINT('Ctrl Pts',(-3.7818353500817,1.,1.04003862055798));
#43910=CARTESIAN_POINT('Ctrl Pts',(-3.78821910787179,1.,1.04404924374422));
#43911=CARTESIAN_POINT('Ctrl Pts',(-3.79459440308786,1.,1.04810913267639));
#43912=CARTESIAN_POINT('Ctrl Pts',(-3.80095039790681,1.,1.05221457990016));
#43913=CARTESIAN_POINT('Ctrl Pts',(-3.80727913637791,1.,1.05636266918644));
#43914=CARTESIAN_POINT('Ctrl Pts',(-3.8135786611749,1.,1.06055206187299));
#43915=CARTESIAN_POINT('Ctrl Pts',(-3.81985083953012,1.,1.0647824403893));
#43916=CARTESIAN_POINT('Ctrl Pts',(-3.82609989967276,1.,1.06905413180359));
#43917=CARTESIAN_POINT('Ctrl Pts',(-3.83233071195144,1.,1.07336766633459));
#43918=CARTESIAN_POINT('Ctrl Pts',(-3.83854714117491,1.,1.07772335353858));
#43919=CARTESIAN_POINT('Ctrl Pts',(-3.8447504803063,1.,1.08212087917991));
#43920=CARTESIAN_POINT('Ctrl Pts',(-3.85094025222713,1.,1.08655950846384));
#43921=CARTESIAN_POINT('Ctrl Pts',(-3.85711487933931,1.,1.09103825516294));
#43922=CARTESIAN_POINT('Ctrl Pts',(-3.86327241021247,1.,1.09555606505013));
#43923=CARTESIAN_POINT('Ctrl Pts',(-3.86941120134849,1.,1.10011198761195));
#43924=CARTESIAN_POINT('Ctrl Pts',(-3.87553067187514,1.,1.10470536603287));
#43925=CARTESIAN_POINT('Ctrl Pts',(-3.88163105531724,1.,1.10933577224008));
#43926=CARTESIAN_POINT('Ctrl Pts',(-3.88771308285171,1.,1.11400292434429));
#43927=CARTESIAN_POINT('Ctrl Pts',(-3.89377768340344,1.,1.11870660794603));
#43928=CARTESIAN_POINT('Ctrl Pts',(-3.89982569750025,1.,1.12344660099043));
#43929=CARTESIAN_POINT('Ctrl Pts',(-3.90585753318737,1.,1.12822258281553));
#43930=CARTESIAN_POINT('Ctrl Pts',(-3.91187321145649,1.,1.13303414693896));
#43931=CARTESIAN_POINT('Ctrl Pts',(-3.91787251936827,1.,1.13788084225554));
#43932=CARTESIAN_POINT('Ctrl Pts',(-3.92385513133997,1.,1.14276220561593));
#43933=CARTESIAN_POINT('Ctrl Pts',(-3.92982073294257,1.,1.14767779451123));
#43934=CARTESIAN_POINT('Ctrl Pts',(-3.9357691705628,1.,1.1526272271632));
#43935=CARTESIAN_POINT('Ctrl Pts',(-3.94170046685203,1.,1.15761018340956));
#43936=CARTESIAN_POINT('Ctrl Pts',(-3.94761474780583,1.,1.16262637999157));
#43937=CARTESIAN_POINT('Ctrl Pts',(-3.95351219509876,1.,1.16767555244438));
#43938=CARTESIAN_POINT('Ctrl Pts',(-3.95939299213276,1.,1.17275743590361));
#43939=CARTESIAN_POINT('Ctrl Pts',(-3.96525726358159,1.,1.17787174135592));
#43940=CARTESIAN_POINT('Ctrl Pts',(-3.97110505165415,1.,1.18301815039831));
#43941=CARTESIAN_POINT('Ctrl Pts',(-3.97693634767754,1.,1.18819633715539));
#43942=CARTESIAN_POINT('Ctrl Pts',(-3.98275111052561,1.,1.19340598349475));
#43943=CARTESIAN_POINT('Ctrl Pts',(-3.98854928957189,1.,1.19864679609566));
#43944=CARTESIAN_POINT('Ctrl Pts',(-3.99433084799666,1.,1.20391852375139));
#43945=CARTESIAN_POINT('Ctrl Pts',(-4.00009577950721,1.,1.20922097029551));
#43946=CARTESIAN_POINT('Ctrl Pts',(-4.00584409522722,1.,1.21455398918133));
#43947=CARTESIAN_POINT('Ctrl Pts',(-4.01042947140789,1.,1.21884478244403));
#43948=CARTESIAN_POINT('Ctrl Pts',(-4.01386104433519,1.,1.22207656455845));
#43949=CARTESIAN_POINT('Ctrl Pts',(-4.01614544569895,1.,1.22423716681317));
#43950=CARTESIAN_POINT('Ctrl Pts',(-4.01728681790024,1.,1.22531898815164));
#43951=CARTESIAN_POINT('Origin',(-4.01728681790024,0.,1.22531898815164));
#43952=CARTESIAN_POINT('',(-3.97027773754922,1.,1.36999806084572));
#43953=CARTESIAN_POINT('Origin',(0.,0.,0.));
#43954=CARTESIAN_POINT('',(-3.66661143271648,1.,0.786422660833743));
#43955=CARTESIAN_POINT('Origin',(0.,1.,0.));
#43956=CARTESIAN_POINT('Ctrl Pts',(-3.66661143271648,1.,0.786422660833743));
#43957=CARTESIAN_POINT('Ctrl Pts',(-3.66661143271648,0.666666666666667,
0.786422660833743));
#43958=CARTESIAN_POINT('Ctrl Pts',(-3.66661143271648,0.333333333333333,
0.786422660833743));
#43959=CARTESIAN_POINT('Ctrl Pts',(-3.66661143271648,-0.333333333333333,
0.786422660833743));
#43960=CARTESIAN_POINT('Ctrl Pts',(-3.66661143271648,-0.666666666666667,
0.786422660833743));
#43961=CARTESIAN_POINT('Ctrl Pts',(-3.66661143271648,-1.,0.786422660833743));
#43962=CARTESIAN_POINT('Ctrl Pts',(-4.13571194405636,-1.,0.732042837400619));
#43963=CARTESIAN_POINT('Ctrl Pts',(-4.13571194405636,1.,0.732042837400619));
#43964=CARTESIAN_POINT('Ctrl Pts',(-4.13420383737278,-1.,0.732488575135926));
#43965=CARTESIAN_POINT('Ctrl Pts',(-4.13420383737278,1.,0.732488575135926));
#43966=CARTESIAN_POINT('Ctrl Pts',(-4.13118752796397,-1.,0.733376589325634));
#43967=CARTESIAN_POINT('Ctrl Pts',(-4.13118752796397,1.,0.733376589325634));
#43968=CARTESIAN_POINT('Ctrl Pts',(-4.12666277572794,-1.,0.734698226767512));
#43969=CARTESIAN_POINT('Ctrl Pts',(-4.12666277572794,1.,0.734698226767512));
#43970=CARTESIAN_POINT('Ctrl Pts',(-4.12062919626082,-1.,0.736439634335347));
#43971=CARTESIAN_POINT('Ctrl Pts',(-4.12062919626082,1.,0.736439634335347));
#43972=CARTESIAN_POINT('Ctrl Pts',(-4.11308626953795,-1.,0.738581708229118));
#43973=CARTESIAN_POINT('Ctrl Pts',(-4.11308626953795,1.,0.738581708229118));
#43974=CARTESIAN_POINT('Ctrl Pts',(-4.1055424175856,-1.,0.740688998555151));
#43975=CARTESIAN_POINT('Ctrl Pts',(-4.1055424175856,1.,0.740688998555151));
#43976=CARTESIAN_POINT('Ctrl Pts',(-4.09799769702712,-1.,0.742761369690017));
#43977=CARTESIAN_POINT('Ctrl Pts',(-4.09799769702712,1.,0.742761369690017));
#43978=CARTESIAN_POINT('Ctrl Pts',(-4.09045220253011,-1.,0.744798649705514));
#43979=CARTESIAN_POINT('Ctrl Pts',(-4.09045220253011,1.,0.744798649705514));
#43980=CARTESIAN_POINT('Ctrl Pts',(-4.08290608094789,-1.,0.746800631490821));
#43981=CARTESIAN_POINT('Ctrl Pts',(-4.08290608094789,1.,0.746800631490821));
#43982=CARTESIAN_POINT('Ctrl Pts',(-4.07535951055363,-1.,0.748767076679177));
#43983=CARTESIAN_POINT('Ctrl Pts',(-4.07535951055363,1.,0.748767076679177));
#43984=CARTESIAN_POINT('Ctrl Pts',(-4.06781267241886,-1.,0.750697720483175));
#43985=CARTESIAN_POINT('Ctrl Pts',(-4.06781267241886,1.,0.750697720483175));
#43986=CARTESIAN_POINT('Ctrl Pts',(-4.06026572221399,-1.,0.752592276482869));
#43987=CARTESIAN_POINT('Ctrl Pts',(-4.06026572221399,1.,0.752592276482869));
#43988=CARTESIAN_POINT('Ctrl Pts',(-4.05271876688106,-1.,0.754450441816411));
#43989=CARTESIAN_POINT('Ctrl Pts',(-4.05271876688106,1.,0.754450441816411));
#43990=CARTESIAN_POINT('Ctrl Pts',(-4.04517182654344,-1.,0.756271902370186));
#43991=CARTESIAN_POINT('Ctrl Pts',(-4.04517182654344,1.,0.756271902370186));
#43992=CARTESIAN_POINT('Ctrl Pts',(-4.03762485803468,-1.,0.758056338885553));
#43993=CARTESIAN_POINT('Ctrl Pts',(-4.03762485803468,1.,0.758056338885553));
#43994=CARTESIAN_POINT('Ctrl Pts',(-4.0300778195465,-1.,0.759803433244166));
#43995=CARTESIAN_POINT('Ctrl Pts',(-4.0300778195465,1.,0.759803433244166));
#43996=CARTESIAN_POINT('Ctrl Pts',(-4.02253072741347,-1.,0.761512875859941));
#43997=CARTESIAN_POINT('Ctrl Pts',(-4.02253072741347,1.,0.761512875859941));
#43998=CARTESIAN_POINT('Ctrl Pts',(-4.01498370680434,-1.,0.763184371182826));
#43999=CARTESIAN_POINT('Ctrl Pts',(-4.01498370680434,1.,0.763184371182826));
#44000=CARTESIAN_POINT('Ctrl Pts',(-4.00743706791366,-1.,0.764817648784946));
#44001=CARTESIAN_POINT('Ctrl Pts',(-4.00743706791366,1.,0.764817648784946));
#44002=CARTESIAN_POINT('Ctrl Pts',(-3.99989129179464,-1.,0.766412457135785));
#44003=CARTESIAN_POINT('Ctrl Pts',(-3.99989129179464,1.,0.766412457135785));
#44004=CARTESIAN_POINT('Ctrl Pts',(-3.99234687880892,-1.,0.767968531377708));
#44005=CARTESIAN_POINT('Ctrl Pts',(-3.99234687880892,1.,0.767968531377708));
#44006=CARTESIAN_POINT('Ctrl Pts',(-3.98480422348403,-1.,0.769485566245459));
#44007=CARTESIAN_POINT('Ctrl Pts',(-3.98480422348403,1.,0.769485566245459));
#44008=CARTESIAN_POINT('Ctrl Pts',(-3.97726349165507,-1.,0.770963190030503));
#44009=CARTESIAN_POINT('Ctrl Pts',(-3.97726349165507,1.,0.770963190030503));
#44010=CARTESIAN_POINT('Ctrl Pts',(-3.96972446532832,-1.,0.772400931772238));
#44011=CARTESIAN_POINT('Ctrl Pts',(-3.96972446532832,1.,0.772400931772238));
#44012=CARTESIAN_POINT('Ctrl Pts',(-3.96218649639876,-1.,0.773798212026682));
#44013=CARTESIAN_POINT('Ctrl Pts',(-3.96218649639876,1.,0.773798212026682));
#44014=CARTESIAN_POINT('Ctrl Pts',(-3.95464885452364,-1.,0.775154418039441));
#44015=CARTESIAN_POINT('Ctrl Pts',(-3.95464885452364,1.,0.775154418039441));
#44016=CARTESIAN_POINT('Ctrl Pts',(-3.94711101619471,-1.,0.77646896669796));
#44017=CARTESIAN_POINT('Ctrl Pts',(-3.94711101619471,1.,0.77646896669796));
#44018=CARTESIAN_POINT('Ctrl Pts',(-3.93957296768098,-1.,0.777741370568549));
#44019=CARTESIAN_POINT('Ctrl Pts',(-3.93957296768098,1.,0.777741370568549));
#44020=CARTESIAN_POINT('Ctrl Pts',(-3.93203552473153,-1.,0.778971308134786));
#44021=CARTESIAN_POINT('Ctrl Pts',(-3.93203552473153,1.,0.778971308134786));
#44022=CARTESIAN_POINT('Ctrl Pts',(-3.92450058323799,-1.,0.780158678615506));
#44023=CARTESIAN_POINT('Ctrl Pts',(-3.92450058323799,1.,0.780158678615506));
#44024=CARTESIAN_POINT('Ctrl Pts',(-3.9169703605466,-1.,0.781303428618343));
#44025=CARTESIAN_POINT('Ctrl Pts',(-3.9169703605466,1.,0.781303428618343));
#44026=CARTESIAN_POINT('Ctrl Pts',(-3.90944671004536,-1.,0.782405395622758));
#44027=CARTESIAN_POINT('Ctrl Pts',(-3.90944671004536,1.,0.782405395622758));
#44028=CARTESIAN_POINT('Ctrl Pts',(-3.90193039043971,-1.,0.783464141529082));
#44029=CARTESIAN_POINT('Ctrl Pts',(-3.90193039043971,1.,0.783464141529082));
#44030=CARTESIAN_POINT('Ctrl Pts',(-3.89442039235105,-1.,0.784478799358335));
#44031=CARTESIAN_POINT('Ctrl Pts',(-3.89442039235105,1.,0.784478799358335));
#44032=CARTESIAN_POINT('Ctrl Pts',(-3.88691313167399,-1.,0.785447890340723));
#44033=CARTESIAN_POINT('Ctrl Pts',(-3.88691313167399,1.,0.785447890340723));
#44034=CARTESIAN_POINT('Ctrl Pts',(-3.87940402818186,-1.,0.786369675812592));
#44035=CARTESIAN_POINT('Ctrl Pts',(-3.87940402818186,1.,0.786369675812592));
#44036=CARTESIAN_POINT('Ctrl Pts',(-3.87188916600905,-1.,0.78724252761798));
#44037=CARTESIAN_POINT('Ctrl Pts',(-3.87188916600905,1.,0.78724252761798));
#44038=CARTESIAN_POINT('Ctrl Pts',(-3.86436702561342,-1.,0.788065315093771));
#44039=CARTESIAN_POINT('Ctrl Pts',(-3.86436702561342,1.,0.788065315093771));
#44040=CARTESIAN_POINT('Ctrl Pts',(-3.85683995872536,-1.,0.788837734090688));
#44041=CARTESIAN_POINT('Ctrl Pts',(-3.85683995872536,1.,0.788837734090688));
#44042=CARTESIAN_POINT('Ctrl Pts',(-3.8493163780891,-1.,0.789560798155618));
#44043=CARTESIAN_POINT('Ctrl Pts',(-3.8493163780891,1.,0.789560798155618));
#44044=CARTESIAN_POINT('Ctrl Pts',(-3.84180762342476,-1.,0.790236124191289));
#44045=CARTESIAN_POINT('Ctrl Pts',(-3.84180762342476,1.,0.790236124191289));
#44046=CARTESIAN_POINT('Ctrl Pts',(-3.83432392054804,-1.,0.79086501270534));
#44047=CARTESIAN_POINT('Ctrl Pts',(-3.83432392054804,1.,0.79086501270534));
#44048=CARTESIAN_POINT('Ctrl Pts',(-3.82687033899799,-1.,0.791447528662381));
#44049=CARTESIAN_POINT('Ctrl Pts',(-3.82687033899799,1.,0.791447528662381));
#44050=CARTESIAN_POINT('Ctrl Pts',(-3.81944345442237,-1.,0.791981740718606));
#44051=CARTESIAN_POINT('Ctrl Pts',(-3.81944345442237,1.,0.791981740718606));
#44052=CARTESIAN_POINT('Ctrl Pts',(-3.81202588694726,-1.,0.792462483517568));
#44053=CARTESIAN_POINT('Ctrl Pts',(-3.81202588694726,1.,0.792462483517568));
#44054=CARTESIAN_POINT('Ctrl Pts',(-3.80459229925598,-1.,0.792882695234693));
#44055=CARTESIAN_POINT('Ctrl Pts',(-3.80459229925598,1.,0.792882695234693));
#44056=CARTESIAN_POINT('Ctrl Pts',(-3.79711921389862,-1.,0.7932356129732));
#44057=CARTESIAN_POINT('Ctrl Pts',(-3.79711921389862,1.,0.7932356129732));
#44058=CARTESIAN_POINT('Ctrl Pts',(-3.78959439439222,-1.,0.793516871680966));
#44059=CARTESIAN_POINT('Ctrl Pts',(-3.78959439439222,1.,0.793516871680966));
#44060=CARTESIAN_POINT('Ctrl Pts',(-3.78202460377617,-1.,0.793726235781339));
#44061=CARTESIAN_POINT('Ctrl Pts',(-3.78202460377617,1.,0.793726235781339));
#44062=CARTESIAN_POINT('Ctrl Pts',(-3.77444863801264,-1.,0.793870523787515));
#44063=CARTESIAN_POINT('Ctrl Pts',(-3.77444863801264,1.,0.793870523787515));
#44064=CARTESIAN_POINT('Ctrl Pts',(-3.76692626931184,-1.,0.793961083689141));
#44065=CARTESIAN_POINT('Ctrl Pts',(-3.76692626931184,1.,0.793961083689141));
#44066=CARTESIAN_POINT('Ctrl Pts',(-3.75951468666325,-1.,0.794008429135047));
#44067=CARTESIAN_POINT('Ctrl Pts',(-3.75951468666325,1.,0.794008429135047));
#44068=CARTESIAN_POINT('Ctrl Pts',(-3.75224692493895,-1.,0.79401734737144));
#44069=CARTESIAN_POINT('Ctrl Pts',(-3.75224692493895,1.,0.79401734737144));
#44070=CARTESIAN_POINT('Ctrl Pts',(-3.74511357728827,-1.,0.79398270045988));
#44071=CARTESIAN_POINT('Ctrl Pts',(-3.74511357728827,1.,0.79398270045988));
#44072=CARTESIAN_POINT('Ctrl Pts',(-3.73803280541576,-1.,0.79388270093679));
#44073=CARTESIAN_POINT('Ctrl Pts',(-3.73803280541576,1.,0.79388270093679));
#44074=CARTESIAN_POINT('Ctrl Pts',(-3.7308691469564,-1.,0.793682750269347));
#44075=CARTESIAN_POINT('Ctrl Pts',(-3.7308691469564,1.,0.793682750269347));
#44076=CARTESIAN_POINT('Ctrl Pts',(-3.7234879729357,-1.,0.79334702378387));
#44077=CARTESIAN_POINT('Ctrl Pts',(-3.7234879729357,1.,0.79334702378387));
#44078=CARTESIAN_POINT('Ctrl Pts',(-3.7158024239604,-1.,0.792848377370115));
#44079=CARTESIAN_POINT('Ctrl Pts',(-3.7158024239604,1.,0.792848377370115));
#44080=CARTESIAN_POINT('Ctrl Pts',(-3.70781724021879,-1.,0.792177688845967));
#44081=CARTESIAN_POINT('Ctrl Pts',(-3.70781724021879,1.,0.792177688845967));
#44082=CARTESIAN_POINT('Ctrl Pts',(-3.69968940808982,-1.,0.791356575696509));
#44083=CARTESIAN_POINT('Ctrl Pts',(-3.69968940808982,1.,0.791356575696509));
#44084=CARTESIAN_POINT('Ctrl Pts',(-3.69172044327754,-1.,0.79043628498958));
#44085=CARTESIAN_POINT('Ctrl Pts',(-3.69172044327754,1.,0.79043628498958));
#44086=CARTESIAN_POINT('Ctrl Pts',(-3.68428439784285,-1.,0.789483546065158));
#44087=CARTESIAN_POINT('Ctrl Pts',(-3.68428439784285,1.,0.789483546065158));
#44088=CARTESIAN_POINT('Ctrl Pts',(-3.67777119516438,-1.,0.788569566220662));
#44089=CARTESIAN_POINT('Ctrl Pts',(-3.67777119516438,1.,0.788569566220662));
#44090=CARTESIAN_POINT('Ctrl Pts',(-3.672529236635,-1.,0.787758799995426));
#44091=CARTESIAN_POINT('Ctrl Pts',(-3.672529236635,1.,0.787758799995426));
#44092=CARTESIAN_POINT('Ctrl Pts',(-3.66879484800625,-1.,0.787095252589507));
#44093=CARTESIAN_POINT('Ctrl Pts',(-3.66879484800625,1.,0.787095252589507));
#44094=CARTESIAN_POINT('Ctrl Pts',(-3.66710211819938,-1.,0.786698783541657));
#44095=CARTESIAN_POINT('Ctrl Pts',(-3.66710211819938,1.,0.786698783541657));
#44096=CARTESIAN_POINT('Ctrl Pts',(-3.66657784454965,-1.,0.786480236184947));
#44097=CARTESIAN_POINT('Ctrl Pts',(-3.66657784454965,1.,0.786480236184947));
#44098=CARTESIAN_POINT('Ctrl Pts',(-3.66655932661846,-1.,0.786369528183039));
#44099=CARTESIAN_POINT('Ctrl Pts',(-3.66655932661846,1.,0.786369528183039));
#44100=CARTESIAN_POINT('Ctrl Pts',(-3.66663282329846,-1.,0.786322922920599));
#44101=CARTESIAN_POINT('Ctrl Pts',(-3.66663282329846,1.,0.786322922920599));
#44102=CARTESIAN_POINT('',(-4.13571194405636,1.,0.732042837400619));
#44103=CARTESIAN_POINT('Ctrl Pts',(-4.13571194405636,1.,0.732042837400619));
#44104=CARTESIAN_POINT('Ctrl Pts',(-4.13420383737278,1.,0.732488575135926));
#44105=CARTESIAN_POINT('Ctrl Pts',(-4.13118752796397,1.,0.733376589325634));
#44106=CARTESIAN_POINT('Ctrl Pts',(-4.12666277572794,1.,0.734698226767512));
#44107=CARTESIAN_POINT('Ctrl Pts',(-4.12062919626082,1.,0.736439634335347));
#44108=CARTESIAN_POINT('Ctrl Pts',(-4.11308626953795,1.,0.738581708229118));
#44109=CARTESIAN_POINT('Ctrl Pts',(-4.1055424175856,1.,0.740688998555151));
#44110=CARTESIAN_POINT('Ctrl Pts',(-4.09799769702712,1.,0.742761369690017));
#44111=CARTESIAN_POINT('Ctrl Pts',(-4.09045220253011,1.,0.744798649705514));
#44112=CARTESIAN_POINT('Ctrl Pts',(-4.08290608094789,1.,0.746800631490821));
#44113=CARTESIAN_POINT('Ctrl Pts',(-4.07535951055363,1.,0.748767076679177));
#44114=CARTESIAN_POINT('Ctrl Pts',(-4.06781267241886,1.,0.750697720483175));
#44115=CARTESIAN_POINT('Ctrl Pts',(-4.06026572221399,1.,0.752592276482869));
#44116=CARTESIAN_POINT('Ctrl Pts',(-4.05271876688106,1.,0.754450441816411));
#44117=CARTESIAN_POINT('Ctrl Pts',(-4.04517182654344,1.,0.756271902370186));
#44118=CARTESIAN_POINT('Ctrl Pts',(-4.03762485803468,1.,0.758056338885553));
#44119=CARTESIAN_POINT('Ctrl Pts',(-4.0300778195465,1.,0.759803433244166));
#44120=CARTESIAN_POINT('Ctrl Pts',(-4.02253072741347,1.,0.761512875859941));
#44121=CARTESIAN_POINT('Ctrl Pts',(-4.01498370680434,1.,0.763184371182826));
#44122=CARTESIAN_POINT('Ctrl Pts',(-4.00743706791366,1.,0.764817648784946));
#44123=CARTESIAN_POINT('Ctrl Pts',(-3.99989129179464,1.,0.766412457135785));
#44124=CARTESIAN_POINT('Ctrl Pts',(-3.99234687880892,1.,0.767968531377708));
#44125=CARTESIAN_POINT('Ctrl Pts',(-3.98480422348403,1.,0.769485566245459));
#44126=CARTESIAN_POINT('Ctrl Pts',(-3.97726349165507,1.,0.770963190030503));
#44127=CARTESIAN_POINT('Ctrl Pts',(-3.96972446532832,1.,0.772400931772238));
#44128=CARTESIAN_POINT('Ctrl Pts',(-3.96218649639876,1.,0.773798212026682));
#44129=CARTESIAN_POINT('Ctrl Pts',(-3.95464885452364,1.,0.775154418039441));
#44130=CARTESIAN_POINT('Ctrl Pts',(-3.94711101619471,1.,0.77646896669796));
#44131=CARTESIAN_POINT('Ctrl Pts',(-3.93957296768098,1.,0.777741370568549));
#44132=CARTESIAN_POINT('Ctrl Pts',(-3.93203552473153,1.,0.778971308134786));
#44133=CARTESIAN_POINT('Ctrl Pts',(-3.92450058323799,1.,0.780158678615506));
#44134=CARTESIAN_POINT('Ctrl Pts',(-3.9169703605466,1.,0.781303428618343));
#44135=CARTESIAN_POINT('Ctrl Pts',(-3.90944671004536,1.,0.782405395622758));
#44136=CARTESIAN_POINT('Ctrl Pts',(-3.90193039043971,1.,0.783464141529082));
#44137=CARTESIAN_POINT('Ctrl Pts',(-3.89442039235105,1.,0.784478799358335));
#44138=CARTESIAN_POINT('Ctrl Pts',(-3.88691313167399,1.,0.785447890340723));
#44139=CARTESIAN_POINT('Ctrl Pts',(-3.87940402818186,1.,0.786369675812592));
#44140=CARTESIAN_POINT('Ctrl Pts',(-3.87188916600905,1.,0.78724252761798));
#44141=CARTESIAN_POINT('Ctrl Pts',(-3.86436702561342,1.,0.788065315093771));
#44142=CARTESIAN_POINT('Ctrl Pts',(-3.85683995872536,1.,0.788837734090688));
#44143=CARTESIAN_POINT('Ctrl Pts',(-3.8493163780891,1.,0.789560798155618));
#44144=CARTESIAN_POINT('Ctrl Pts',(-3.84180762342476,1.,0.790236124191289));
#44145=CARTESIAN_POINT('Ctrl Pts',(-3.83432392054804,1.,0.79086501270534));
#44146=CARTESIAN_POINT('Ctrl Pts',(-3.82687033899799,1.,0.791447528662381));
#44147=CARTESIAN_POINT('Ctrl Pts',(-3.81944345442237,1.,0.791981740718606));
#44148=CARTESIAN_POINT('Ctrl Pts',(-3.81202588694726,1.,0.792462483517568));
#44149=CARTESIAN_POINT('Ctrl Pts',(-3.80459229925598,1.,0.792882695234693));
#44150=CARTESIAN_POINT('Ctrl Pts',(-3.79711921389862,1.,0.7932356129732));
#44151=CARTESIAN_POINT('Ctrl Pts',(-3.78959439439222,1.,0.793516871680966));
#44152=CARTESIAN_POINT('Ctrl Pts',(-3.78202460377617,1.,0.793726235781339));
#44153=CARTESIAN_POINT('Ctrl Pts',(-3.77444863801264,1.,0.793870523787515));
#44154=CARTESIAN_POINT('Ctrl Pts',(-3.76692626931184,1.,0.793961083689141));
#44155=CARTESIAN_POINT('Ctrl Pts',(-3.75951468666325,1.,0.794008429135047));
#44156=CARTESIAN_POINT('Ctrl Pts',(-3.75224692493895,1.,0.79401734737144));
#44157=CARTESIAN_POINT('Ctrl Pts',(-3.74511357728827,1.,0.79398270045988));
#44158=CARTESIAN_POINT('Ctrl Pts',(-3.73803280541576,1.,0.79388270093679));
#44159=CARTESIAN_POINT('Ctrl Pts',(-3.7308691469564,1.,0.793682750269347));
#44160=CARTESIAN_POINT('Ctrl Pts',(-3.7234879729357,1.,0.79334702378387));
#44161=CARTESIAN_POINT('Ctrl Pts',(-3.7158024239604,1.,0.792848377370115));
#44162=CARTESIAN_POINT('Ctrl Pts',(-3.70781724021879,1.,0.792177688845967));
#44163=CARTESIAN_POINT('Ctrl Pts',(-3.69968940808982,1.,0.791356575696509));
#44164=CARTESIAN_POINT('Ctrl Pts',(-3.69172044327754,1.,0.79043628498958));
#44165=CARTESIAN_POINT('Ctrl Pts',(-3.68428439784285,1.,0.789483546065158));
#44166=CARTESIAN_POINT('Ctrl Pts',(-3.67777119516438,1.,0.788569566220662));
#44167=CARTESIAN_POINT('Ctrl Pts',(-3.672529236635,1.,0.787758799995426));
#44168=CARTESIAN_POINT('Ctrl Pts',(-3.66907505398769,1.,0.787145041181588));
#44169=CARTESIAN_POINT('Ctrl Pts',(-3.66743103898844,1.,0.786774337198499));
#44170=CARTESIAN_POINT('Ctrl Pts',(-3.66680946938396,1.,0.786565919559889));
#44171=CARTESIAN_POINT('Ctrl Pts',(-3.66664310415236,1.,0.786459983896781));
#44172=CARTESIAN_POINT('Ctrl Pts',(-3.66661143271648,1.,0.786422660833743));
#44173=CARTESIAN_POINT('',(-4.13571194405636,0.,0.732042837400619));
#44174=CARTESIAN_POINT('Ctrl Pts',(-3.73016218570874,-1.,0.385214314776329));
#44175=CARTESIAN_POINT('Ctrl Pts',(-3.73016218570874,1.,0.385214314776329));
#44176=CARTESIAN_POINT('Ctrl Pts',(-3.73010668803185,-1.,0.385147278814804));
#44177=CARTESIAN_POINT('Ctrl Pts',(-3.73010668803185,1.,0.385147278814804));
#44178=CARTESIAN_POINT('Ctrl Pts',(-3.73015851028729,-1.,0.385047711603887));
#44179=CARTESIAN_POINT('Ctrl Pts',(-3.73015851028729,1.,0.385047711603887));
#44180=CARTESIAN_POINT('Ctrl Pts',(-3.73072465900727,-1.,0.385001870183841));
#44181=CARTESIAN_POINT('Ctrl Pts',(-3.73072465900727,1.,0.385001870183841));
#44182=CARTESIAN_POINT('Ctrl Pts',(-3.73245705639337,-1.,0.385147887989514));
#44183=CARTESIAN_POINT('Ctrl Pts',(-3.73245705639337,1.,0.385147887989514));
#44184=CARTESIAN_POINT('Ctrl Pts',(-3.73621371845475,-1.,0.385670806454744));
#44185=CARTESIAN_POINT('Ctrl Pts',(-3.73621371845475,1.,0.385670806454744));
#44186=CARTESIAN_POINT('Ctrl Pts',(-3.74144965781088,-1.,0.386519576222035));
#44187=CARTESIAN_POINT('Ctrl Pts',(-3.74144965781088,1.,0.386519576222035));
#44188=CARTESIAN_POINT('Ctrl Pts',(-3.74792651696269,-1.,0.387663020050396));
#44189=CARTESIAN_POINT('Ctrl Pts',(-3.74792651696269,1.,0.387663020050396));
#44190=CARTESIAN_POINT('Ctrl Pts',(-3.75529302894757,-1.,0.389054775898251));
#44191=CARTESIAN_POINT('Ctrl Pts',(-3.75529302894757,1.,0.389054775898251));
#44192=CARTESIAN_POINT('Ctrl Pts',(-3.76315635032993,-1.,0.390642072979259));
#44193=CARTESIAN_POINT('Ctrl Pts',(-3.76315635032993,1.,0.390642072979259));
#44194=CARTESIAN_POINT('Ctrl Pts',(-3.77114011595892,-1.,0.392372786223346));
#44195=CARTESIAN_POINT('Ctrl Pts',(-3.77114011595892,1.,0.392372786223346));
#44196=CARTESIAN_POINT('Ctrl Pts',(-3.77894173114368,-1.,0.394202481011595));
#44197=CARTESIAN_POINT('Ctrl Pts',(-3.77894173114368,1.,0.394202481011595));
#44198=CARTESIAN_POINT('Ctrl Pts',(-3.78640521279479,-1.,0.396103205335028));
#44199=CARTESIAN_POINT('Ctrl Pts',(-3.78640521279479,1.,0.396103205335028));
#44200=CARTESIAN_POINT('Ctrl Pts',(-3.79352887163457,-1.,0.398064818684158));
#44201=CARTESIAN_POINT('Ctrl Pts',(-3.79352887163457,1.,0.398064818684158));
#44202=CARTESIAN_POINT('Ctrl Pts',(-3.80040370384659,-1.,0.400088346504726));
#44203=CARTESIAN_POINT('Ctrl Pts',(-3.80040370384659,1.,0.400088346504726));
#44204=CARTESIAN_POINT('Ctrl Pts',(-3.80716881962763,-1.,0.402181320148474));
#44205=CARTESIAN_POINT('Ctrl Pts',(-3.80716881962763,1.,0.402181320148474));
#44206=CARTESIAN_POINT('Ctrl Pts',(-3.81396374287762,-1.,0.404352694628236));
#44207=CARTESIAN_POINT('Ctrl Pts',(-3.81396374287762,1.,0.404352694628236));
#44208=CARTESIAN_POINT('Ctrl Pts',(-3.82087303913741,-1.,0.406607038258906));
#44209=CARTESIAN_POINT('Ctrl Pts',(-3.82087303913741,1.,0.406607038258906));
#44210=CARTESIAN_POINT('Ctrl Pts',(-3.82790724256397,-1.,0.408942371447377));
#44211=CARTESIAN_POINT('Ctrl Pts',(-3.82790724256397,1.,0.408942371447377));
#44212=CARTESIAN_POINT('Ctrl Pts',(-3.83503345578645,-1.,0.411353038798459));
#44213=CARTESIAN_POINT('Ctrl Pts',(-3.83503345578645,1.,0.411353038798459));
#44214=CARTESIAN_POINT('Ctrl Pts',(-3.84219403994742,-1.,0.413831367016726));
#44215=CARTESIAN_POINT('Ctrl Pts',(-3.84219403994742,1.,0.413831367016726));
#44216=CARTESIAN_POINT('Ctrl Pts',(-3.8493286415751,-1.,0.41636967805292));
#44217=CARTESIAN_POINT('Ctrl Pts',(-3.8493286415751,1.,0.41636967805292));
#44218=CARTESIAN_POINT('Ctrl Pts',(-3.85639825648031,-1.,0.418962468086809));
#44219=CARTESIAN_POINT('Ctrl Pts',(-3.85639825648031,1.,0.418962468086809));
#44220=CARTESIAN_POINT('Ctrl Pts',(-3.86339652542749,-1.,0.421607423177575));
#44221=CARTESIAN_POINT('Ctrl Pts',(-3.86339652542749,1.,0.421607423177575));
#44222=CARTESIAN_POINT('Ctrl Pts',(-3.87033643487882,-1.,0.424304173195142));
#44223=CARTESIAN_POINT('Ctrl Pts',(-3.87033643487882,1.,0.424304173195142));
#44224=CARTESIAN_POINT('Ctrl Pts',(-3.87724240306609,-1.,0.427053541173469));
#44225=CARTESIAN_POINT('Ctrl Pts',(-3.87724240306609,1.,0.427053541173469));
#44226=CARTESIAN_POINT('Ctrl Pts',(-3.88414070943334,-1.,0.429856640579733));
#44227=CARTESIAN_POINT('Ctrl Pts',(-3.88414070943334,1.,0.429856640579733));
#44228=CARTESIAN_POINT('Ctrl Pts',(-3.89104947940592,-1.,0.432713929544439));
#44229=CARTESIAN_POINT('Ctrl Pts',(-3.89104947940592,1.,0.432713929544439));
#44230=CARTESIAN_POINT('Ctrl Pts',(-3.8979725665544,-1.,0.435624629433505));
#44231=CARTESIAN_POINT('Ctrl Pts',(-3.8979725665544,1.,0.435624629433505));
#44232=CARTESIAN_POINT('Ctrl Pts',(-3.90490512938546,-1.,0.438587235458233));
#44233=CARTESIAN_POINT('Ctrl Pts',(-3.90490512938546,1.,0.438587235458233));
#44234=CARTESIAN_POINT('Ctrl Pts',(-3.91183704069146,-1.,0.441599824524047));
#44235=CARTESIAN_POINT('Ctrl Pts',(-3.91183704069146,1.,0.441599824524047));
#44236=CARTESIAN_POINT('Ctrl Pts',(-3.91875701610721,-1.,0.444660430230592));
#44237=CARTESIAN_POINT('Ctrl Pts',(-3.91875701610721,1.,0.444660430230592));
#44238=CARTESIAN_POINT('Ctrl Pts',(-3.92565674143424,-1.,0.447767416837296));
#44239=CARTESIAN_POINT('Ctrl Pts',(-3.92565674143424,1.,0.447767416837296));
#44240=CARTESIAN_POINT('Ctrl Pts',(-3.93253407403128,-1.,0.450919768356347));
#44241=CARTESIAN_POINT('Ctrl Pts',(-3.93253407403128,1.,0.450919768356347));
#44242=CARTESIAN_POINT('Ctrl Pts',(-3.93939080846298,-1.,0.454116879027576));
#44243=CARTESIAN_POINT('Ctrl Pts',(-3.93939080846298,1.,0.454116879027576));
#44244=CARTESIAN_POINT('Ctrl Pts',(-3.94623117206675,-1.,0.457358410451674));
#44245=CARTESIAN_POINT('Ctrl Pts',(-3.94623117206675,1.,0.457358410451674));
#44246=CARTESIAN_POINT('Ctrl Pts',(-3.95306005817363,-1.,0.460644124429119));
#44247=CARTESIAN_POINT('Ctrl Pts',(-3.95306005817363,1.,0.460644124429119));
#44248=CARTESIAN_POINT('Ctrl Pts',(-3.95988133243543,-1.,0.463973722115744));
#44249=CARTESIAN_POINT('Ctrl Pts',(-3.95988133243543,1.,0.463973722115744));
#44250=CARTESIAN_POINT('Ctrl Pts',(-3.96669622273946,-1.,0.467346690880671));
#44251=CARTESIAN_POINT('Ctrl Pts',(-3.96669622273946,1.,0.467346690880671));
#44252=CARTESIAN_POINT('Ctrl Pts',(-3.97350414289415,-1.,0.470762379613477));
#44253=CARTESIAN_POINT('Ctrl Pts',(-3.97350414289415,1.,0.470762379613477));
#44254=CARTESIAN_POINT('Ctrl Pts',(-3.9803033804443,-1.,0.474220061019542));
#44255=CARTESIAN_POINT('Ctrl Pts',(-3.9803033804443,1.,0.474220061019542));
#44256=CARTESIAN_POINT('Ctrl Pts',(-3.98709184306743,-1.,0.477718999122033));
#44257=CARTESIAN_POINT('Ctrl Pts',(-3.98709184306743,1.,0.477718999122033));
#44258=CARTESIAN_POINT('Ctrl Pts',(-3.99386775880655,-1.,0.481258512209638));
#44259=CARTESIAN_POINT('Ctrl Pts',(-3.99386775880655,1.,0.481258512209638));
#44260=CARTESIAN_POINT('Ctrl Pts',(-4.00063045119234,-1.,0.484838042421754));
#44261=CARTESIAN_POINT('Ctrl Pts',(-4.00063045119234,1.,0.484838042421754));
#44262=CARTESIAN_POINT('Ctrl Pts',(-4.0073800839092,-1.,0.48845713042453));
#44263=CARTESIAN_POINT('Ctrl Pts',(-4.0073800839092,1.,0.48845713042453));
#44264=CARTESIAN_POINT('Ctrl Pts',(-4.01411733503486,-1.,0.49211538341793));
#44265=CARTESIAN_POINT('Ctrl Pts',(-4.01411733503486,1.,0.49211538341793));
#44266=CARTESIAN_POINT('Ctrl Pts',(-4.02084308851813,-1.,0.495812444326223));
#44267=CARTESIAN_POINT('Ctrl Pts',(-4.02084308851813,1.,0.495812444326223));
#44268=CARTESIAN_POINT('Ctrl Pts',(-4.0275581398015,-1.,0.499547962340889));
#44269=CARTESIAN_POINT('Ctrl Pts',(-4.0275581398015,1.,0.499547962340889));
#44270=CARTESIAN_POINT('Ctrl Pts',(-4.0342628417439,-1.,0.503321556915513));
#44271=CARTESIAN_POINT('Ctrl Pts',(-4.0342628417439,1.,0.503321556915513));
#44272=CARTESIAN_POINT('Ctrl Pts',(-4.04095715149074,-1.,0.507132823288361));
#44273=CARTESIAN_POINT('Ctrl Pts',(-4.04095715149074,1.,0.507132823288361));
#44274=CARTESIAN_POINT('Ctrl Pts',(-4.04764078815591,-1.,0.510981349219173));
#44275=CARTESIAN_POINT('Ctrl Pts',(-4.04764078815591,1.,0.510981349219173));
#44276=CARTESIAN_POINT('Ctrl Pts',(-4.05431335771261,-1.,0.514866728193104));
#44277=CARTESIAN_POINT('Ctrl Pts',(-4.05431335771261,1.,0.514866728193104));
#44278=CARTESIAN_POINT('Ctrl Pts',(-4.06097448037934,-1.,0.518788572336809));
#44279=CARTESIAN_POINT('Ctrl Pts',(-4.06097448037934,1.,0.518788572336809));
#44280=CARTESIAN_POINT('Ctrl Pts',(-4.06762394471075,-1.,0.522746528602767));
#44281=CARTESIAN_POINT('Ctrl Pts',(-4.06762394471075,1.,0.522746528602767));
#44282=CARTESIAN_POINT('Ctrl Pts',(-4.07426172299496,-1.,0.526740277226999));
#44283=CARTESIAN_POINT('Ctrl Pts',(-4.07426172299496,1.,0.526740277226999));
#44284=CARTESIAN_POINT('Ctrl Pts',(-4.08088789536488,-1.,0.530769518728075));
#44285=CARTESIAN_POINT('Ctrl Pts',(-4.08088789536488,1.,0.530769518728075));
#44286=CARTESIAN_POINT('Ctrl Pts',(-4.08750259988693,-1.,0.534833963476999));
#44287=CARTESIAN_POINT('Ctrl Pts',(-4.08750259988693,1.,0.534833963476999));
#44288=CARTESIAN_POINT('Ctrl Pts',(-4.09410597627116,-1.,0.53893332117992));
#44289=CARTESIAN_POINT('Ctrl Pts',(-4.09410597627116,1.,0.53893332117992));
#44290=CARTESIAN_POINT('Ctrl Pts',(-4.10069810244473,-1.,0.543067286878457));
#44291=CARTESIAN_POINT('Ctrl Pts',(-4.10069810244473,1.,0.543067286878457));
#44292=CARTESIAN_POINT('Ctrl Pts',(-4.1072789702877,-1.,0.547235539486759));
#44293=CARTESIAN_POINT('Ctrl Pts',(-4.1072789702877,1.,0.547235539486759));
#44294=CARTESIAN_POINT('Ctrl Pts',(-4.11384852025578,-1.,0.551437758498246));
#44295=CARTESIAN_POINT('Ctrl Pts',(-4.11384852025578,1.,0.551437758498246));
#44296=CARTESIAN_POINT('Ctrl Pts',(-4.1204066619623,-1.,0.555673636130778));
#44297=CARTESIAN_POINT('Ctrl Pts',(-4.1204066619623,1.,0.555673636130778));
#44298=CARTESIAN_POINT('Ctrl Pts',(-4.12695329951859,-1.,0.559942890594628));
#44299=CARTESIAN_POINT('Ctrl Pts',(-4.12695329951859,1.,0.559942890594628));
#44300=CARTESIAN_POINT('Ctrl Pts',(-4.13348835726086,-1.,0.564245279535705));
#44301=CARTESIAN_POINT('Ctrl Pts',(-4.13348835726086,1.,0.564245279535705));
#44302=CARTESIAN_POINT('Ctrl Pts',(-4.14001179828669,-1.,0.568580610187116));
#44303=CARTESIAN_POINT('Ctrl Pts',(-4.14001179828669,1.,0.568580610187116));
#44304=CARTESIAN_POINT('Ctrl Pts',(-4.14652361065787,-1.,0.572948736066276));
#44305=CARTESIAN_POINT('Ctrl Pts',(-4.14652361065787,1.,0.572948736066276));
#44306=CARTESIAN_POINT('Ctrl Pts',(-4.1517237611974,-1.,0.576469391673916));
#44307=CARTESIAN_POINT('Ctrl Pts',(-4.1517237611974,1.,0.576469391673916));
#44308=CARTESIAN_POINT('Ctrl Pts',(-4.15561864787379,-1.,0.579124568912543));
#44309=CARTESIAN_POINT('Ctrl Pts',(-4.15561864787379,1.,0.579124568912543));
#44310=CARTESIAN_POINT('Ctrl Pts',(-4.15821291712391,-1.,0.580901211462913));
#44311=CARTESIAN_POINT('Ctrl Pts',(-4.15821291712391,1.,0.580901211462913));
#44312=CARTESIAN_POINT('Ctrl Pts',(-4.15950947128175,-1.,0.581791163835814));
#44313=CARTESIAN_POINT('Ctrl Pts',(-4.15950947128175,1.,0.581791163835814));
#44314=CARTESIAN_POINT('',(-3.73017266276632,1.,0.385112848332549));
#44315=CARTESIAN_POINT('Ctrl Pts',(-3.73017266276632,-1.,0.385112848332549));
#44316=CARTESIAN_POINT('Ctrl Pts',(-3.73017266276632,-0.666666666666667,
0.385112848332549));
#44317=CARTESIAN_POINT('Ctrl Pts',(-3.73017266276632,-0.333333333333333,
0.385112848332549));
#44318=CARTESIAN_POINT('Ctrl Pts',(-3.73017266276632,0.333333333333333,
0.385112848332549));
#44319=CARTESIAN_POINT('Ctrl Pts',(-3.73017266276632,0.666666666666667,
0.385112848332549));
#44320=CARTESIAN_POINT('Ctrl Pts',(-3.73017266276632,1.,0.385112848332549));
#44321=CARTESIAN_POINT('',(-4.15950947128175,1.,0.581791163835814));
#44322=CARTESIAN_POINT('',(-4.15950947128175,0.,0.581791163835814));
#44323=CARTESIAN_POINT('Ctrl Pts',(-3.73017266276632,1.,0.385112848332549));
#44324=CARTESIAN_POINT('Ctrl Pts',(-3.73021431755218,1.,0.385087139001609));
#44325=CARTESIAN_POINT('Ctrl Pts',(-3.73040527620929,1.,0.385037797882046));
#44326=CARTESIAN_POINT('Ctrl Pts',(-3.73106082862399,1.,0.385031656499141));
#44327=CARTESIAN_POINT('Ctrl Pts',(-3.73273893363318,1.,0.385187124633964));
#44328=CARTESIAN_POINT('Ctrl Pts',(-3.73621371845475,1.,0.385670806454744));
#44329=CARTESIAN_POINT('Ctrl Pts',(-3.74144965781088,1.,0.386519576222035));
#44330=CARTESIAN_POINT('Ctrl Pts',(-3.74792651696269,1.,0.387663020050396));
#44331=CARTESIAN_POINT('Ctrl Pts',(-3.75529302894757,1.,0.389054775898251));
#44332=CARTESIAN_POINT('Ctrl Pts',(-3.76315635032993,1.,0.390642072979259));
#44333=CARTESIAN_POINT('Ctrl Pts',(-3.77114011595892,1.,0.392372786223346));
#44334=CARTESIAN_POINT('Ctrl Pts',(-3.77894173114368,1.,0.394202481011595));
#44335=CARTESIAN_POINT('Ctrl Pts',(-3.78640521279479,1.,0.396103205335028));
#44336=CARTESIAN_POINT('Ctrl Pts',(-3.79352887163457,1.,0.398064818684158));
#44337=CARTESIAN_POINT('Ctrl Pts',(-3.80040370384659,1.,0.400088346504726));
#44338=CARTESIAN_POINT('Ctrl Pts',(-3.80716881962763,1.,0.402181320148474));
#44339=CARTESIAN_POINT('Ctrl Pts',(-3.81396374287762,1.,0.404352694628236));
#44340=CARTESIAN_POINT('Ctrl Pts',(-3.82087303913741,1.,0.406607038258906));
#44341=CARTESIAN_POINT('Ctrl Pts',(-3.82790724256397,1.,0.408942371447377));
#44342=CARTESIAN_POINT('Ctrl Pts',(-3.83503345578645,1.,0.411353038798459));
#44343=CARTESIAN_POINT('Ctrl Pts',(-3.84219403994742,1.,0.413831367016726));
#44344=CARTESIAN_POINT('Ctrl Pts',(-3.8493286415751,1.,0.41636967805292));
#44345=CARTESIAN_POINT('Ctrl Pts',(-3.85639825648031,1.,0.418962468086809));
#44346=CARTESIAN_POINT('Ctrl Pts',(-3.86339652542749,1.,0.421607423177575));
#44347=CARTESIAN_POINT('Ctrl Pts',(-3.87033643487882,1.,0.424304173195142));
#44348=CARTESIAN_POINT('Ctrl Pts',(-3.87724240306609,1.,0.427053541173469));
#44349=CARTESIAN_POINT('Ctrl Pts',(-3.88414070943334,1.,0.429856640579733));
#44350=CARTESIAN_POINT('Ctrl Pts',(-3.89104947940592,1.,0.432713929544439));
#44351=CARTESIAN_POINT('Ctrl Pts',(-3.8979725665544,1.,0.435624629433505));
#44352=CARTESIAN_POINT('Ctrl Pts',(-3.90490512938546,1.,0.438587235458233));
#44353=CARTESIAN_POINT('Ctrl Pts',(-3.91183704069146,1.,0.441599824524047));
#44354=CARTESIAN_POINT('Ctrl Pts',(-3.91875701610721,1.,0.444660430230592));
#44355=CARTESIAN_POINT('Ctrl Pts',(-3.92565674143424,1.,0.447767416837296));
#44356=CARTESIAN_POINT('Ctrl Pts',(-3.93253407403128,1.,0.450919768356347));
#44357=CARTESIAN_POINT('Ctrl Pts',(-3.93939080846298,1.,0.454116879027576));
#44358=CARTESIAN_POINT('Ctrl Pts',(-3.94623117206675,1.,0.457358410451674));
#44359=CARTESIAN_POINT('Ctrl Pts',(-3.95306005817363,1.,0.460644124429119));
#44360=CARTESIAN_POINT('Ctrl Pts',(-3.95988133243543,1.,0.463973722115744));
#44361=CARTESIAN_POINT('Ctrl Pts',(-3.96669622273946,1.,0.467346690880671));
#44362=CARTESIAN_POINT('Ctrl Pts',(-3.97350414289415,1.,0.470762379613477));
#44363=CARTESIAN_POINT('Ctrl Pts',(-3.9803033804443,1.,0.474220061019542));
#44364=CARTESIAN_POINT('Ctrl Pts',(-3.98709184306743,1.,0.477718999122033));
#44365=CARTESIAN_POINT('Ctrl Pts',(-3.99386775880655,1.,0.481258512209638));
#44366=CARTESIAN_POINT('Ctrl Pts',(-4.00063045119234,1.,0.484838042421754));
#44367=CARTESIAN_POINT('Ctrl Pts',(-4.0073800839092,1.,0.48845713042453));
#44368=CARTESIAN_POINT('Ctrl Pts',(-4.01411733503486,1.,0.49211538341793));
#44369=CARTESIAN_POINT('Ctrl Pts',(-4.02084308851813,1.,0.495812444326223));
#44370=CARTESIAN_POINT('Ctrl Pts',(-4.0275581398015,1.,0.499547962340889));
#44371=CARTESIAN_POINT('Ctrl Pts',(-4.0342628417439,1.,0.503321556915513));
#44372=CARTESIAN_POINT('Ctrl Pts',(-4.04095715149074,1.,0.507132823288361));
#44373=CARTESIAN_POINT('Ctrl Pts',(-4.04764078815591,1.,0.510981349219173));
#44374=CARTESIAN_POINT('Ctrl Pts',(-4.05431335771261,1.,0.514866728193104));
#44375=CARTESIAN_POINT('Ctrl Pts',(-4.06097448037934,1.,0.518788572336809));
#44376=CARTESIAN_POINT('Ctrl Pts',(-4.06762394471075,1.,0.522746528602767));
#44377=CARTESIAN_POINT('Ctrl Pts',(-4.07426172299496,1.,0.526740277226999));
#44378=CARTESIAN_POINT('Ctrl Pts',(-4.08088789536488,1.,0.530769518728075));
#44379=CARTESIAN_POINT('Ctrl Pts',(-4.08750259988693,1.,0.534833963476999));
#44380=CARTESIAN_POINT('Ctrl Pts',(-4.09410597627116,1.,0.53893332117992));
#44381=CARTESIAN_POINT('Ctrl Pts',(-4.10069810244473,1.,0.543067286878457));
#44382=CARTESIAN_POINT('Ctrl Pts',(-4.1072789702877,1.,0.547235539486759));
#44383=CARTESIAN_POINT('Ctrl Pts',(-4.11384852025578,1.,0.551437758498246));
#44384=CARTESIAN_POINT('Ctrl Pts',(-4.1204066619623,1.,0.555673636130778));
#44385=CARTESIAN_POINT('Ctrl Pts',(-4.12695329951859,1.,0.559942890594628));
#44386=CARTESIAN_POINT('Ctrl Pts',(-4.13348835726086,1.,0.564245279535705));
#44387=CARTESIAN_POINT('Ctrl Pts',(-4.14001179828669,1.,0.568580610187116));
#44388=CARTESIAN_POINT('Ctrl Pts',(-4.14652361065787,1.,0.572948736066276));
#44389=CARTESIAN_POINT('Ctrl Pts',(-4.1517237611974,1.,0.576469391673916));
#44390=CARTESIAN_POINT('Ctrl Pts',(-4.15561864787379,1.,0.579124568912543));
#44391=CARTESIAN_POINT('Ctrl Pts',(-4.15821291712391,1.,0.580901211462913));
#44392=CARTESIAN_POINT('Ctrl Pts',(-4.15950947128175,1.,0.581791163835814));
#44393=CARTESIAN_POINT('Origin',(-4.15950947128175,0.,0.581791163835814));
#44394=CARTESIAN_POINT('',(-4.13571194405636,1.,0.732042837400619));
#44395=CARTESIAN_POINT('Origin',(0.,0.,0.));
#44396=CARTESIAN_POINT('',(-3.74449296982994,1.,0.203156094897896));
#44397=CARTESIAN_POINT('Origin',(0.,1.,0.));
#44398=CARTESIAN_POINT('Ctrl Pts',(-3.74449296982994,1.,0.203156094897896));
#44399=CARTESIAN_POINT('Ctrl Pts',(-3.74449296982994,0.666666666666667,
0.203156094897896));
#44400=CARTESIAN_POINT('Ctrl Pts',(-3.74449296982994,0.333333333333333,
0.203156094897896));
#44401=CARTESIAN_POINT('Ctrl Pts',(-3.74449296982994,-0.333333333333333,
0.203156094897896));
#44402=CARTESIAN_POINT('Ctrl Pts',(-3.74449296982994,-0.666666666666667,
0.203156094897896));
#44403=CARTESIAN_POINT('Ctrl Pts',(-3.74449296982994,-1.,0.203156094897896));
#44404=CARTESIAN_POINT('Ctrl Pts',(-4.19931119685982,-1.,0.0760622897878236));
#44405=CARTESIAN_POINT('Ctrl Pts',(-4.19931119685982,1.,0.0760622897878236));
#44406=CARTESIAN_POINT('Ctrl Pts',(-4.19789138621624,-1.,0.0767384596142195));
#44407=CARTESIAN_POINT('Ctrl Pts',(-4.19789138621624,1.,0.0767384596142195));
#44408=CARTESIAN_POINT('Ctrl Pts',(-4.19505112860624,-1.,0.0780873956244402));
#44409=CARTESIAN_POINT('Ctrl Pts',(-4.19505112860624,1.,0.0780873956244402));
#44410=CARTESIAN_POINT('Ctrl Pts',(-4.19078883322483,-1.,0.0801005887117603));
#44411=CARTESIAN_POINT('Ctrl Pts',(-4.19078883322483,1.,0.0801005887117603));
#44412=CARTESIAN_POINT('Ctrl Pts',(-4.1851019532944,-1.,0.082764416438951));
#44413=CARTESIAN_POINT('Ctrl Pts',(-4.1851019532944,1.,0.082764416438951));
#44414=CARTESIAN_POINT('Ctrl Pts',(-4.17798698669991,-1.,0.0860600915552515));
#44415=CARTESIAN_POINT('Ctrl Pts',(-4.17798698669991,1.,0.0860600915552515));
#44416=CARTESIAN_POINT('Ctrl Pts',(-4.17086566491823,-1.,0.0893215560850327));
#44417=CARTESIAN_POINT('Ctrl Pts',(-4.17086566491823,1.,0.0893215560850327));
#44418=CARTESIAN_POINT('Ctrl Pts',(-4.16373802265942,-1.,0.092548667216769));
#44419=CARTESIAN_POINT('Ctrl Pts',(-4.16373802265942,1.,0.092548667216769));
#44420=CARTESIAN_POINT('Ctrl Pts',(-4.15660412653006,-1.,0.0957412403297067));
#44421=CARTESIAN_POINT('Ctrl Pts',(-4.15660412653006,1.,0.0957412403297067));
#44422=CARTESIAN_POINT('Ctrl Pts',(-4.1494640891762,-1.,0.0988990478899811));
#44423=CARTESIAN_POINT('Ctrl Pts',(-4.1494640891762,1.,0.0988990478899811));
#44424=CARTESIAN_POINT('Ctrl Pts',(-4.14231804938737,-1.,0.102021826577454));
#44425=CARTESIAN_POINT('Ctrl Pts',(-4.14231804938737,1.,0.102021826577454));
#44426=CARTESIAN_POINT('Ctrl Pts',(-4.13516614458396,-1.,0.105109286538864));
#44427=CARTESIAN_POINT('Ctrl Pts',(-4.13516614458396,1.,0.105109286538864));
#44428=CARTESIAN_POINT('Ctrl Pts',(-4.12800848371386,-1.,0.10816112052835));
#44429=CARTESIAN_POINT('Ctrl Pts',(-4.12800848371386,1.,0.10816112052835));
#44430=CARTESIAN_POINT('Ctrl Pts',(-4.12084512502444,-1.,0.111177012683377));
#44431=CARTESIAN_POINT('Ctrl Pts',(-4.12084512502444,1.,0.111177012683377));
#44432=CARTESIAN_POINT('Ctrl Pts',(-4.11367603925313,-1.,0.114156649609601));
#44433=CARTESIAN_POINT('Ctrl Pts',(-4.11367603925313,1.,0.114156649609601));
#44434=CARTESIAN_POINT('Ctrl Pts',(-4.10650113382187,-1.,0.117099722731704));
#44435=CARTESIAN_POINT('Ctrl Pts',(-4.10650113382187,1.,0.117099722731704));
#44436=CARTESIAN_POINT('Ctrl Pts',(-4.09932031767243,-1.,0.120005924388162));
#44437=CARTESIAN_POINT('Ctrl Pts',(-4.09932031767243,1.,0.120005924388162));
#44438=CARTESIAN_POINT('Ctrl Pts',(-4.09213355850836,-1.,0.122874946249119));
#44439=CARTESIAN_POINT('Ctrl Pts',(-4.09213355850836,1.,0.122874946249119));
#44440=CARTESIAN_POINT('Ctrl Pts',(-4.08494093372315,-1.,0.125706476822529));
#44441=CARTESIAN_POINT('Ctrl Pts',(-4.08494093372315,1.,0.125706476822529));
#44442=CARTESIAN_POINT('Ctrl Pts',(-4.07774270738809,-1.,0.128500200484814));
#44443=CARTESIAN_POINT('Ctrl Pts',(-4.07774270738809,1.,0.128500200484814));
#44444=CARTESIAN_POINT('Ctrl Pts',(-4.07053931528579,-1.,0.131255793548914));
#44445=CARTESIAN_POINT('Ctrl Pts',(-4.07053931528579,1.,0.131255793548914));
#44446=CARTESIAN_POINT('Ctrl Pts',(-4.06333121018476,-1.,0.133972916144225));
#44447=CARTESIAN_POINT('Ctrl Pts',(-4.06333121018476,1.,0.133972916144225));
#44448=CARTESIAN_POINT('Ctrl Pts',(-4.05611873400122,-1.,0.136651205046111));
#44449=CARTESIAN_POINT('Ctrl Pts',(-4.05611873400122,1.,0.136651205046111));
#44450=CARTESIAN_POINT('Ctrl Pts',(-4.04890199238056,-1.,0.139290267180059));
#44451=CARTESIAN_POINT('Ctrl Pts',(-4.04890199238056,1.,0.139290267180059));
#44452=CARTESIAN_POINT('Ctrl Pts',(-4.04168069633842,-1.,0.141889671485508));
#44453=CARTESIAN_POINT('Ctrl Pts',(-4.04168069633842,1.,0.141889671485508));
#44454=CARTESIAN_POINT('Ctrl Pts',(-4.03445411510403,-1.,0.144448947038352));
#44455=CARTESIAN_POINT('Ctrl Pts',(-4.03445411510403,1.,0.144448947038352));
#44456=CARTESIAN_POINT('Ctrl Pts',(-4.02722143147048,-1.,0.146967602878998));
#44457=CARTESIAN_POINT('Ctrl Pts',(-4.02722143147048,1.,0.146967602878998));
#44458=CARTESIAN_POINT('Ctrl Pts',(-4.01998203715588,-1.,0.149445144968707));
#44459=CARTESIAN_POINT('Ctrl Pts',(-4.01998203715588,1.,0.149445144968707));
#44460=CARTESIAN_POINT('Ctrl Pts',(-4.01273584234684,-1.,0.151881094022909));
#44461=CARTESIAN_POINT('Ctrl Pts',(-4.01273584234684,1.,0.151881094022909));
#44462=CARTESIAN_POINT('Ctrl Pts',(-4.00548360245297,-1.,0.15427500487231));
#44463=CARTESIAN_POINT('Ctrl Pts',(-4.00548360245297,1.,0.15427500487231));
#44464=CARTESIAN_POINT('Ctrl Pts',(-3.99822717425869,-1.,0.156626481393735));
#44465=CARTESIAN_POINT('Ctrl Pts',(-3.99822717425869,1.,0.156626481393735));
#44466=CARTESIAN_POINT('Ctrl Pts',(-3.99096873945862,-1.,0.158935123982796));
#44467=CARTESIAN_POINT('Ctrl Pts',(-3.99096873945862,1.,0.158935123982796));
#44468=CARTESIAN_POINT('Ctrl Pts',(-3.98371010319866,-1.,0.161200482186087));
#44469=CARTESIAN_POINT('Ctrl Pts',(-3.98371010319866,1.,0.161200482186087));
#44470=CARTESIAN_POINT('Ctrl Pts',(-3.97645194630944,-1.,0.163422004609999));
#44471=CARTESIAN_POINT('Ctrl Pts',(-3.97645194630944,1.,0.163422004609999));
#44472=CARTESIAN_POINT('Ctrl Pts',(-3.9691931362141,-1.,0.165598992851097));
#44473=CARTESIAN_POINT('Ctrl Pts',(-3.9691931362141,1.,0.165598992851097));
#44474=CARTESIAN_POINT('Ctrl Pts',(-3.96192990160296,-1.,0.167730547023312));
#44475=CARTESIAN_POINT('Ctrl Pts',(-3.96192990160296,1.,0.167730547023312));
#44476=CARTESIAN_POINT('Ctrl Pts',(-3.95465744665263,-1.,0.16981566637413));
#44477=CARTESIAN_POINT('Ctrl Pts',(-3.95465744665263,1.,0.16981566637413));
#44478=CARTESIAN_POINT('Ctrl Pts',(-3.94737164900861,-1.,0.171853355369233));
#44479=CARTESIAN_POINT('Ctrl Pts',(-3.94737164900861,1.,0.171853355369233));
#44480=CARTESIAN_POINT('Ctrl Pts',(-3.94007083096214,-1.,0.173842734974607));
#44481=CARTESIAN_POINT('Ctrl Pts',(-3.94007083096214,1.,0.173842734974607));
#44482=CARTESIAN_POINT('Ctrl Pts',(-3.93275726771049,-1.,0.175783136893872));
#44483=CARTESIAN_POINT('Ctrl Pts',(-3.93275726771049,1.,0.175783136893872));
#44484=CARTESIAN_POINT('Ctrl Pts',(-3.92543942697672,-1.,0.177674246152328));
#44485=CARTESIAN_POINT('Ctrl Pts',(-3.92543942697672,1.,0.177674246152328));
#44486=CARTESIAN_POINT('Ctrl Pts',(-3.91812876180948,-1.,0.179515885822894));
#44487=CARTESIAN_POINT('Ctrl Pts',(-3.91812876180948,1.,0.179515885822894));
#44488=CARTESIAN_POINT('Ctrl Pts',(-3.91083557557193,-1.,0.181307740731796));
#44489=CARTESIAN_POINT('Ctrl Pts',(-3.91083557557193,1.,0.181307740731796));
#44490=CARTESIAN_POINT('Ctrl Pts',(-3.90356488555138,-1.,0.183049081993193));
#44491=CARTESIAN_POINT('Ctrl Pts',(-3.90356488555138,1.,0.183049081993193));
#44492=CARTESIAN_POINT('Ctrl Pts',(-3.89631300742633,-1.,0.184738537728035));
#44493=CARTESIAN_POINT('Ctrl Pts',(-3.89631300742633,1.,0.184738537728035));
#44494=CARTESIAN_POINT('Ctrl Pts',(-3.88906196725817,-1.,0.186373724985263));
#44495=CARTESIAN_POINT('Ctrl Pts',(-3.88906196725817,1.,0.186373724985263));
#44496=CARTESIAN_POINT('Ctrl Pts',(-3.88178563496187,-1.,0.187951632512663));
#44497=CARTESIAN_POINT('Ctrl Pts',(-3.88178563496187,1.,0.187951632512663));
#44498=CARTESIAN_POINT('Ctrl Pts',(-3.87445976418377,-1.,0.189469253358254));
#44499=CARTESIAN_POINT('Ctrl Pts',(-3.87445976418377,1.,0.189469253358254));
#44500=CARTESIAN_POINT('Ctrl Pts',(-3.8670715862477,-1.,0.190924190418613));
#44501=CARTESIAN_POINT('Ctrl Pts',(-3.8670715862477,1.,0.190924190418613));
#44502=CARTESIAN_POINT('Ctrl Pts',(-3.85962774407652,-1.,0.192315153044979));
#44503=CARTESIAN_POINT('Ctrl Pts',(-3.85962774407652,1.,0.192315153044979));
#44504=CARTESIAN_POINT('Ctrl Pts',(-3.85216762264019,-1.,0.193642806777747));
#44505=CARTESIAN_POINT('Ctrl Pts',(-3.85216762264019,1.,0.193642806777747));
#44506=CARTESIAN_POINT('Ctrl Pts',(-3.84475203347052,-1.,0.194909009460254));
#44507=CARTESIAN_POINT('Ctrl Pts',(-3.84475203347052,1.,0.194909009460254));
#44508=CARTESIAN_POINT('Ctrl Pts',(-3.83743910616265,-1.,0.196115198971889));
#44509=CARTESIAN_POINT('Ctrl Pts',(-3.83743910616265,1.,0.196115198971889));
#44510=CARTESIAN_POINT('Ctrl Pts',(-3.83026221776488,-1.,0.197260935827375));
#44511=CARTESIAN_POINT('Ctrl Pts',(-3.83026221776488,1.,0.197260935827375));
#44512=CARTESIAN_POINT('Ctrl Pts',(-3.82321127348981,-1.,0.19834261690047));
#44513=CARTESIAN_POINT('Ctrl Pts',(-3.82321127348981,1.,0.19834261690047));
#44514=CARTESIAN_POINT('Ctrl Pts',(-3.81620203429702,-1.,0.199351525297396));
#44515=CARTESIAN_POINT('Ctrl Pts',(-3.81620203429702,1.,0.199351525297396));
#44516=CARTESIAN_POINT('Ctrl Pts',(-3.80909529318501,-1.,0.20027467943329));
#44517=CARTESIAN_POINT('Ctrl Pts',(-3.80909529318501,1.,0.20027467943329));
#44518=CARTESIAN_POINT('Ctrl Pts',(-3.80175247447171,-1.,0.201097756307252));
#44519=CARTESIAN_POINT('Ctrl Pts',(-3.80175247447171,1.,0.201097756307252));
#44520=CARTESIAN_POINT('Ctrl Pts',(-3.79408354187274,-1.,0.201807533800799));
#44521=CARTESIAN_POINT('Ctrl Pts',(-3.79408354187274,1.,0.201807533800799));
#44522=CARTESIAN_POINT('Ctrl Pts',(-3.78609175019317,-1.,0.202394260512193));
#44523=CARTESIAN_POINT('Ctrl Pts',(-3.78609175019317,1.,0.202394260512193));
#44524=CARTESIAN_POINT('Ctrl Pts',(-3.77793553476879,-1.,0.202854729699196));
#44525=CARTESIAN_POINT('Ctrl Pts',(-3.77793553476879,1.,0.202854729699196));
#44526=CARTESIAN_POINT('Ctrl Pts',(-3.76992071595267,-1.,0.203192390045337));
#44527=CARTESIAN_POINT('Ctrl Pts',(-3.76992071595267,1.,0.203192390045337));
#44528=CARTESIAN_POINT('Ctrl Pts',(-3.76242717937273,-1.,0.203414634707646));
#44529=CARTESIAN_POINT('Ctrl Pts',(-3.76242717937273,1.,0.203414634707646));
#44530=CARTESIAN_POINT('Ctrl Pts',(-3.75585118707924,-1.,0.203530796848403));
#44531=CARTESIAN_POINT('Ctrl Pts',(-3.75585118707924,1.,0.203530796848403));
#44532=CARTESIAN_POINT('Ctrl Pts',(-3.75054693397716,-1.,0.203550035479097));
#44533=CARTESIAN_POINT('Ctrl Pts',(-3.75054693397716,1.,0.203550035479097));
#44534=CARTESIAN_POINT('Ctrl Pts',(-3.74675472018582,-1.,0.203478844530229));
#44535=CARTESIAN_POINT('Ctrl Pts',(-3.74675472018582,1.,0.203478844530229));
#44536=CARTESIAN_POINT('Ctrl Pts',(-3.7450208092684,-1.,0.203352057956055));
#44537=CARTESIAN_POINT('Ctrl Pts',(-3.7450208092684,1.,0.203352057956055));
#44538=CARTESIAN_POINT('Ctrl Pts',(-3.74446880195845,-1.,0.203218215747894));
#44539=CARTESIAN_POINT('Ctrl Pts',(-3.74446880195845,1.,0.203218215747894));
#44540=CARTESIAN_POINT('Ctrl Pts',(-3.74443319346666,-1.,0.20311176758786));
#44541=CARTESIAN_POINT('Ctrl Pts',(-3.74443319346666,1.,0.20311176758786));
#44542=CARTESIAN_POINT('Ctrl Pts',(-3.74449849461127,-1.,0.203054238699719));
#44543=CARTESIAN_POINT('Ctrl Pts',(-3.74449849461127,1.,0.203054238699719));
#44544=CARTESIAN_POINT('',(-4.19931119685982,1.,0.0760622897878236));
#44545=CARTESIAN_POINT('Ctrl Pts',(-4.19931119685982,1.,0.0760622897878236));
#44546=CARTESIAN_POINT('Ctrl Pts',(-4.19789138621624,1.,0.0767384596142195));
#44547=CARTESIAN_POINT('Ctrl Pts',(-4.19505112860624,1.,0.0780873956244402));
#44548=CARTESIAN_POINT('Ctrl Pts',(-4.19078883322483,1.,0.0801005887117603));
#44549=CARTESIAN_POINT('Ctrl Pts',(-4.1851019532944,1.,0.082764416438951));
#44550=CARTESIAN_POINT('Ctrl Pts',(-4.17798698669991,1.,0.0860600915552515));
#44551=CARTESIAN_POINT('Ctrl Pts',(-4.17086566491823,1.,0.0893215560850327));
#44552=CARTESIAN_POINT('Ctrl Pts',(-4.16373802265942,1.,0.092548667216769));
#44553=CARTESIAN_POINT('Ctrl Pts',(-4.15660412653006,1.,0.0957412403297067));
#44554=CARTESIAN_POINT('Ctrl Pts',(-4.1494640891762,1.,0.0988990478899811));
#44555=CARTESIAN_POINT('Ctrl Pts',(-4.14231804938737,1.,0.102021826577454));
#44556=CARTESIAN_POINT('Ctrl Pts',(-4.13516614458396,1.,0.105109286538864));
#44557=CARTESIAN_POINT('Ctrl Pts',(-4.12800848371386,1.,0.10816112052835));
#44558=CARTESIAN_POINT('Ctrl Pts',(-4.12084512502444,1.,0.111177012683377));
#44559=CARTESIAN_POINT('Ctrl Pts',(-4.11367603925313,1.,0.114156649609601));
#44560=CARTESIAN_POINT('Ctrl Pts',(-4.10650113382187,1.,0.117099722731704));
#44561=CARTESIAN_POINT('Ctrl Pts',(-4.09932031767243,1.,0.120005924388162));
#44562=CARTESIAN_POINT('Ctrl Pts',(-4.09213355850836,1.,0.122874946249119));
#44563=CARTESIAN_POINT('Ctrl Pts',(-4.08494093372315,1.,0.125706476822529));
#44564=CARTESIAN_POINT('Ctrl Pts',(-4.07774270738809,1.,0.128500200484814));
#44565=CARTESIAN_POINT('Ctrl Pts',(-4.07053931528579,1.,0.131255793548914));
#44566=CARTESIAN_POINT('Ctrl Pts',(-4.06333121018476,1.,0.133972916144225));
#44567=CARTESIAN_POINT('Ctrl Pts',(-4.05611873400122,1.,0.136651205046111));
#44568=CARTESIAN_POINT('Ctrl Pts',(-4.04890199238056,1.,0.139290267180059));
#44569=CARTESIAN_POINT('Ctrl Pts',(-4.04168069633842,1.,0.141889671485508));
#44570=CARTESIAN_POINT('Ctrl Pts',(-4.03445411510403,1.,0.144448947038352));
#44571=CARTESIAN_POINT('Ctrl Pts',(-4.02722143147048,1.,0.146967602878998));
#44572=CARTESIAN_POINT('Ctrl Pts',(-4.01998203715588,1.,0.149445144968707));
#44573=CARTESIAN_POINT('Ctrl Pts',(-4.01273584234684,1.,0.151881094022909));
#44574=CARTESIAN_POINT('Ctrl Pts',(-4.00548360245297,1.,0.15427500487231));
#44575=CARTESIAN_POINT('Ctrl Pts',(-3.99822717425869,1.,0.156626481393735));
#44576=CARTESIAN_POINT('Ctrl Pts',(-3.99096873945862,1.,0.158935123982796));
#44577=CARTESIAN_POINT('Ctrl Pts',(-3.98371010319866,1.,0.161200482186087));
#44578=CARTESIAN_POINT('Ctrl Pts',(-3.97645194630944,1.,0.163422004609999));
#44579=CARTESIAN_POINT('Ctrl Pts',(-3.9691931362141,1.,0.165598992851097));
#44580=CARTESIAN_POINT('Ctrl Pts',(-3.96192990160296,1.,0.167730547023312));
#44581=CARTESIAN_POINT('Ctrl Pts',(-3.95465744665263,1.,0.16981566637413));
#44582=CARTESIAN_POINT('Ctrl Pts',(-3.94737164900861,1.,0.171853355369233));
#44583=CARTESIAN_POINT('Ctrl Pts',(-3.94007083096214,1.,0.173842734974607));
#44584=CARTESIAN_POINT('Ctrl Pts',(-3.93275726771049,1.,0.175783136893872));
#44585=CARTESIAN_POINT('Ctrl Pts',(-3.92543942697672,1.,0.177674246152328));
#44586=CARTESIAN_POINT('Ctrl Pts',(-3.91812876180948,1.,0.179515885822894));
#44587=CARTESIAN_POINT('Ctrl Pts',(-3.91083557557193,1.,0.181307740731796));
#44588=CARTESIAN_POINT('Ctrl Pts',(-3.90356488555138,1.,0.183049081993193));
#44589=CARTESIAN_POINT('Ctrl Pts',(-3.89631300742633,1.,0.184738537728035));
#44590=CARTESIAN_POINT('Ctrl Pts',(-3.88906196725817,1.,0.186373724985263));
#44591=CARTESIAN_POINT('Ctrl Pts',(-3.88178563496187,1.,0.187951632512663));
#44592=CARTESIAN_POINT('Ctrl Pts',(-3.87445976418377,1.,0.189469253358254));
#44593=CARTESIAN_POINT('Ctrl Pts',(-3.8670715862477,1.,0.190924190418613));
#44594=CARTESIAN_POINT('Ctrl Pts',(-3.85962774407652,1.,0.192315153044979));
#44595=CARTESIAN_POINT('Ctrl Pts',(-3.85216762264019,1.,0.193642806777747));
#44596=CARTESIAN_POINT('Ctrl Pts',(-3.84475203347052,1.,0.194909009460254));
#44597=CARTESIAN_POINT('Ctrl Pts',(-3.83743910616265,1.,0.196115198971889));
#44598=CARTESIAN_POINT('Ctrl Pts',(-3.83026221776488,1.,0.197260935827375));
#44599=CARTESIAN_POINT('Ctrl Pts',(-3.82321127348981,1.,0.19834261690047));
#44600=CARTESIAN_POINT('Ctrl Pts',(-3.81620203429702,1.,0.199351525297396));
#44601=CARTESIAN_POINT('Ctrl Pts',(-3.80909529318501,1.,0.20027467943329));
#44602=CARTESIAN_POINT('Ctrl Pts',(-3.80175247447171,1.,0.201097756307252));
#44603=CARTESIAN_POINT('Ctrl Pts',(-3.79408354187274,1.,0.201807533800799));
#44604=CARTESIAN_POINT('Ctrl Pts',(-3.78609175019317,1.,0.202394260512193));
#44605=CARTESIAN_POINT('Ctrl Pts',(-3.77793553476879,1.,0.202854729699196));
#44606=CARTESIAN_POINT('Ctrl Pts',(-3.76992071595267,1.,0.203192390045337));
#44607=CARTESIAN_POINT('Ctrl Pts',(-3.76242717937273,1.,0.203414634707646));
#44608=CARTESIAN_POINT('Ctrl Pts',(-3.75585118707924,1.,0.203530796848403));
#44609=CARTESIAN_POINT('Ctrl Pts',(-3.75054693397716,1.,0.203550035479097));
#44610=CARTESIAN_POINT('Ctrl Pts',(-3.74703926501843,1.,0.203484186269314));
#44611=CARTESIAN_POINT('Ctrl Pts',(-3.74535749969262,1.,0.203375226874331));
#44612=CARTESIAN_POINT('Ctrl Pts',(-3.74471097893961,1.,0.203266610111264));
#44613=CARTESIAN_POINT('Ctrl Pts',(-3.74453008995129,1.,0.203188003947965));
#44614=CARTESIAN_POINT('Ctrl Pts',(-3.74449296982994,1.,0.203156094897896));
#44615=CARTESIAN_POINT('',(-4.19931119685982,0.,0.0760622897878236));
#44616=CARTESIAN_POINT('Ctrl Pts',(-3.74449849461127,-1.,-0.20305423869972));
#44617=CARTESIAN_POINT('Ctrl Pts',(-3.74449849461127,1.,-0.20305423869972));
#44618=CARTESIAN_POINT('Ctrl Pts',(-3.7444331934681,-1.,-0.203111767587923));
#44619=CARTESIAN_POINT('Ctrl Pts',(-3.7444331934681,1.,-0.203111767587923));
#44620=CARTESIAN_POINT('Ctrl Pts',(-3.7444688019622,-1.,-0.203218215748059));
#44621=CARTESIAN_POINT('Ctrl Pts',(-3.7444688019622,1.,-0.203218215748059));
#44622=CARTESIAN_POINT('Ctrl Pts',(-3.74502080927395,-1.,-0.203352057956297));
#44623=CARTESIAN_POINT('Ctrl Pts',(-3.74502080927395,1.,-0.203352057956297));
#44624=CARTESIAN_POINT('Ctrl Pts',(-3.7467547201908,-1.,-0.203478844530447));
#44625=CARTESIAN_POINT('Ctrl Pts',(-3.7467547201908,1.,-0.203478844530447));
#44626=CARTESIAN_POINT('Ctrl Pts',(-3.75054693397875,-1.,-0.203550035479166));
#44627=CARTESIAN_POINT('Ctrl Pts',(-3.75054693397875,1.,-0.203550035479166));
#44628=CARTESIAN_POINT('Ctrl Pts',(-3.75585118707734,-1.,-0.203530796848322));
#44629=CARTESIAN_POINT('Ctrl Pts',(-3.75585118707734,1.,-0.203530796848322));
#44630=CARTESIAN_POINT('Ctrl Pts',(-3.76242717936885,-1.,-0.203414634707478));
#44631=CARTESIAN_POINT('Ctrl Pts',(-3.76242717936885,1.,-0.203414634707478));
#44632=CARTESIAN_POINT('Ctrl Pts',(-3.7699207159487,-1.,-0.203192390045164));
#44633=CARTESIAN_POINT('Ctrl Pts',(-3.7699207159487,1.,-0.203192390045164));
#44634=CARTESIAN_POINT('Ctrl Pts',(-3.77793553476614,-1.,-0.202854729699081));
#44635=CARTESIAN_POINT('Ctrl Pts',(-3.77793553476614,1.,-0.202854729699081));
#44636=CARTESIAN_POINT('Ctrl Pts',(-3.78609175019242,-1.,-0.20239426051216));
#44637=CARTESIAN_POINT('Ctrl Pts',(-3.78609175019242,1.,-0.20239426051216));
#44638=CARTESIAN_POINT('Ctrl Pts',(-3.7940835418736,-1.,-0.201807533800837));
#44639=CARTESIAN_POINT('Ctrl Pts',(-3.7940835418736,1.,-0.201807533800837));
#44640=CARTESIAN_POINT('Ctrl Pts',(-3.80175247447337,-1.,-0.201097756307326));
#44641=CARTESIAN_POINT('Ctrl Pts',(-3.80175247447337,1.,-0.201097756307326));
#44642=CARTESIAN_POINT('Ctrl Pts',(-3.80909529318669,-1.,-0.200274679433364));
#44643=CARTESIAN_POINT('Ctrl Pts',(-3.80909529318669,1.,-0.200274679433364));
#44644=CARTESIAN_POINT('Ctrl Pts',(-3.81620203429815,-1.,-0.199351525297447));
#44645=CARTESIAN_POINT('Ctrl Pts',(-3.81620203429815,1.,-0.199351525297447));
#44646=CARTESIAN_POINT('Ctrl Pts',(-3.82321127349016,-1.,-0.198342616900486));
#44647=CARTESIAN_POINT('Ctrl Pts',(-3.82321127349016,1.,-0.198342616900486));
#44648=CARTESIAN_POINT('Ctrl Pts',(-3.83026221776456,-1.,-0.197260935827361));
#44649=CARTESIAN_POINT('Ctrl Pts',(-3.83026221776456,1.,-0.197260935827361));
#44650=CARTESIAN_POINT('Ctrl Pts',(-3.83743910616195,-1.,-0.196115198971859));
#44651=CARTESIAN_POINT('Ctrl Pts',(-3.83743910616195,1.,-0.196115198971859));
#44652=CARTESIAN_POINT('Ctrl Pts',(-3.84475203346977,-1.,-0.194909009460221));
#44653=CARTESIAN_POINT('Ctrl Pts',(-3.84475203346977,1.,-0.194909009460221));
#44654=CARTESIAN_POINT('Ctrl Pts',(-3.85216762263966,-1.,-0.193642806777723));
#44655=CARTESIAN_POINT('Ctrl Pts',(-3.85216762263966,1.,-0.193642806777723));
#44656=CARTESIAN_POINT('Ctrl Pts',(-3.85962774407633,-1.,-0.192315153044971));
#44657=CARTESIAN_POINT('Ctrl Pts',(-3.85962774407633,1.,-0.192315153044971));
#44658=CARTESIAN_POINT('Ctrl Pts',(-3.86707158624783,-1.,-0.19092419041862));
#44659=CARTESIAN_POINT('Ctrl Pts',(-3.86707158624783,1.,-0.19092419041862));
#44660=CARTESIAN_POINT('Ctrl Pts',(-3.87445976418412,-1.,-0.189469253358272));
#44661=CARTESIAN_POINT('Ctrl Pts',(-3.87445976418412,1.,-0.189469253358272));
#44662=CARTESIAN_POINT('Ctrl Pts',(-3.88178563496228,-1.,-0.187951632512685));
#44663=CARTESIAN_POINT('Ctrl Pts',(-3.88178563496228,1.,-0.187951632512685));
#44664=CARTESIAN_POINT('Ctrl Pts',(-3.88906196725848,-1.,-0.18637372498528));
#44665=CARTESIAN_POINT('Ctrl Pts',(-3.88906196725848,1.,-0.18637372498528));
#44666=CARTESIAN_POINT('Ctrl Pts',(-3.89631300742646,-1.,-0.184738537728043));
#44667=CARTESIAN_POINT('Ctrl Pts',(-3.89631300742646,1.,-0.184738537728043));
#44668=CARTESIAN_POINT('Ctrl Pts',(-3.90356488555132,-1.,-0.183049081993191));
#44669=CARTESIAN_POINT('Ctrl Pts',(-3.90356488555132,1.,-0.183049081993191));
#44670=CARTESIAN_POINT('Ctrl Pts',(-3.91083557557175,-1.,-0.181307740731786));
#44671=CARTESIAN_POINT('Ctrl Pts',(-3.91083557557175,1.,-0.181307740731786));
#44672=CARTESIAN_POINT('Ctrl Pts',(-3.91812876180926,-1.,-0.179515885822882));
#44673=CARTESIAN_POINT('Ctrl Pts',(-3.91812876180926,1.,-0.179515885822882));
#44674=CARTESIAN_POINT('Ctrl Pts',(-3.92543942697655,-1.,-0.177674246152317));
#44675=CARTESIAN_POINT('Ctrl Pts',(-3.92543942697655,1.,-0.177674246152317));
#44676=CARTESIAN_POINT('Ctrl Pts',(-3.93275726771042,-1.,-0.175783136893868));
#44677=CARTESIAN_POINT('Ctrl Pts',(-3.93275726771042,1.,-0.175783136893868));
#44678=CARTESIAN_POINT('Ctrl Pts',(-3.94007083096217,-1.,-0.17384273497461));
#44679=CARTESIAN_POINT('Ctrl Pts',(-3.94007083096217,1.,-0.17384273497461));
#44680=CARTESIAN_POINT('Ctrl Pts',(-3.94737164900868,-1.,-0.17185335536924));
#44681=CARTESIAN_POINT('Ctrl Pts',(-3.94737164900868,1.,-0.17185335536924));
#44682=CARTESIAN_POINT('Ctrl Pts',(-3.95465744665268,-1.,-0.169815666374139));
#44683=CARTESIAN_POINT('Ctrl Pts',(-3.95465744665268,1.,-0.169815666374139));
#44684=CARTESIAN_POINT('Ctrl Pts',(-3.96192990160296,-1.,-0.167730547023319));
#44685=CARTESIAN_POINT('Ctrl Pts',(-3.96192990160296,1.,-0.167730547023319));
#44686=CARTESIAN_POINT('Ctrl Pts',(-3.96919313621407,-1.,-0.165598992851102));
#44687=CARTESIAN_POINT('Ctrl Pts',(-3.96919313621407,1.,-0.165598992851102));
#44688=CARTESIAN_POINT('Ctrl Pts',(-3.97645194630943,-1.,-0.163422004609999));
#44689=CARTESIAN_POINT('Ctrl Pts',(-3.97645194630943,1.,-0.163422004609999));
#44690=CARTESIAN_POINT('Ctrl Pts',(-3.98371010319872,-1.,-0.161200482186085));
#44691=CARTESIAN_POINT('Ctrl Pts',(-3.98371010319872,1.,-0.161200482186085));
#44692=CARTESIAN_POINT('Ctrl Pts',(-3.99096873945878,-1.,-0.158935123982793));
#44693=CARTESIAN_POINT('Ctrl Pts',(-3.99096873945878,1.,-0.158935123982793));
#44694=CARTESIAN_POINT('Ctrl Pts',(-3.99822717425893,-1.,-0.156626481393734));
#44695=CARTESIAN_POINT('Ctrl Pts',(-3.99822717425893,1.,-0.156626481393734));
#44696=CARTESIAN_POINT('Ctrl Pts',(-4.00548360245319,-1.,-0.154275004872311));
#44697=CARTESIAN_POINT('Ctrl Pts',(-4.00548360245319,1.,-0.154275004872311));
#44698=CARTESIAN_POINT('Ctrl Pts',(-4.01273584234689,-1.,-0.151881094022911));
#44699=CARTESIAN_POINT('Ctrl Pts',(-4.01273584234689,1.,-0.151881094022911));
#44700=CARTESIAN_POINT('Ctrl Pts',(-4.01998203715564,-1.,-0.149445144968707));
#44701=CARTESIAN_POINT('Ctrl Pts',(-4.01998203715564,1.,-0.149445144968707));
#44702=CARTESIAN_POINT('Ctrl Pts',(-4.02722143146994,-1.,-0.146967602878994));
#44703=CARTESIAN_POINT('Ctrl Pts',(-4.02722143146994,1.,-0.146967602878994));
#44704=CARTESIAN_POINT('Ctrl Pts',(-4.03445411510333,-1.,-0.144448947038345));
#44705=CARTESIAN_POINT('Ctrl Pts',(-4.03445411510333,1.,-0.144448947038345));
#44706=CARTESIAN_POINT('Ctrl Pts',(-4.04168069633781,-1.,-0.1418896714855));
#44707=CARTESIAN_POINT('Ctrl Pts',(-4.04168069633781,1.,-0.1418896714855));
#44708=CARTESIAN_POINT('Ctrl Pts',(-4.04890199238036,-1.,-0.139290267180057));
#44709=CARTESIAN_POINT('Ctrl Pts',(-4.04890199238036,1.,-0.139290267180057));
#44710=CARTESIAN_POINT('Ctrl Pts',(-4.05611873400172,-1.,-0.136651205046119));
#44711=CARTESIAN_POINT('Ctrl Pts',(-4.05611873400172,1.,-0.136651205046119));
#44712=CARTESIAN_POINT('Ctrl Pts',(-4.06333121018596,-1.,-0.133972916144245));
#44713=CARTESIAN_POINT('Ctrl Pts',(-4.06333121018596,1.,-0.133972916144245));
#44714=CARTESIAN_POINT('Ctrl Pts',(-4.0705393152874,-1.,-0.13125579354894));
#44715=CARTESIAN_POINT('Ctrl Pts',(-4.0705393152874,1.,-0.13125579354894));
#44716=CARTESIAN_POINT('Ctrl Pts',(-4.07774270738954,-1.,-0.128500200484838));
#44717=CARTESIAN_POINT('Ctrl Pts',(-4.07774270738954,1.,-0.128500200484838));
#44718=CARTESIAN_POINT('Ctrl Pts',(-4.08494093372377,-1.,-0.12570647682254));
#44719=CARTESIAN_POINT('Ctrl Pts',(-4.08494093372377,1.,-0.12570647682254));
#44720=CARTESIAN_POINT('Ctrl Pts',(-4.09213355850756,-1.,-0.122874946249107));
#44721=CARTESIAN_POINT('Ctrl Pts',(-4.09213355850756,1.,-0.122874946249107));
#44722=CARTESIAN_POINT('Ctrl Pts',(-4.09932031767002,-1.,-0.120005924388124));
#44723=CARTESIAN_POINT('Ctrl Pts',(-4.09932031767002,1.,-0.120005924388124));
#44724=CARTESIAN_POINT('Ctrl Pts',(-4.10650113381833,-1.,-0.117099722731648));
#44725=CARTESIAN_POINT('Ctrl Pts',(-4.10650113381833,1.,-0.117099722731648));
#44726=CARTESIAN_POINT('Ctrl Pts',(-4.11367603924961,-1.,-0.114156649609546));
#44727=CARTESIAN_POINT('Ctrl Pts',(-4.11367603924961,1.,-0.114156649609546));
#44728=CARTESIAN_POINT('Ctrl Pts',(-4.1208451250225,-1.,-0.111177012683347));
#44729=CARTESIAN_POINT('Ctrl Pts',(-4.1208451250225,1.,-0.111177012683347));
#44730=CARTESIAN_POINT('Ctrl Pts',(-4.12800848371504,-1.,-0.108161120528369));
#44731=CARTESIAN_POINT('Ctrl Pts',(-4.12800848371504,1.,-0.108161120528369));
#44732=CARTESIAN_POINT('Ctrl Pts',(-4.13516614458895,-1.,-0.105109286538945));
#44733=CARTESIAN_POINT('Ctrl Pts',(-4.13516614458895,1.,-0.105109286538945));
#44734=CARTESIAN_POINT('Ctrl Pts',(-4.14231804939538,-1.,-0.102021826577584));
#44735=CARTESIAN_POINT('Ctrl Pts',(-4.14231804939538,1.,-0.102021826577584));
#44736=CARTESIAN_POINT('Ctrl Pts',(-4.14946408918485,-1.,-0.0988990478901226));
#44737=CARTESIAN_POINT('Ctrl Pts',(-4.14946408918485,1.,-0.0988990478901226));
#44738=CARTESIAN_POINT('Ctrl Pts',(-4.15660412653577,-1.,-0.0957412403298007));
#44739=CARTESIAN_POINT('Ctrl Pts',(-4.15660412653577,1.,-0.0957412403298007));
#44740=CARTESIAN_POINT('Ctrl Pts',(-4.16373802265839,-1.,-0.0925486672167531));
#44741=CARTESIAN_POINT('Ctrl Pts',(-4.16373802265839,1.,-0.0925486672167531));
#44742=CARTESIAN_POINT('Ctrl Pts',(-4.17086566490794,-1.,-0.0893215560848649));
#44743=CARTESIAN_POINT('Ctrl Pts',(-4.17086566490794,1.,-0.0893215560848649));
#44744=CARTESIAN_POINT('Ctrl Pts',(-4.17798698668094,-1.,-0.0860600915549397));
#44745=CARTESIAN_POINT('Ctrl Pts',(-4.17798698668094,1.,-0.0860600915549397));
#44746=CARTESIAN_POINT('Ctrl Pts',(-4.18510195327123,-1.,-0.0827644164385679));
#44747=CARTESIAN_POINT('Ctrl Pts',(-4.18510195327123,1.,-0.0827644164385679));
#44748=CARTESIAN_POINT('Ctrl Pts',(-4.19078883320504,-1.,-0.080100588711432));
#44749=CARTESIAN_POINT('Ctrl Pts',(-4.19078883320504,1.,-0.080100588711432));
#44750=CARTESIAN_POINT('Ctrl Pts',(-4.19505112859416,-1.,-0.0780873956242397));
#44751=CARTESIAN_POINT('Ctrl Pts',(-4.19505112859416,1.,-0.0780873956242397));
#44752=CARTESIAN_POINT('Ctrl Pts',(-4.1978913862118,-1.,-0.0767384596141464));
#44753=CARTESIAN_POINT('Ctrl Pts',(-4.1978913862118,1.,-0.0767384596141464));
#44754=CARTESIAN_POINT('Ctrl Pts',(-4.19931119685982,-1.,-0.0760622897878246));
#44755=CARTESIAN_POINT('Ctrl Pts',(-4.19931119685982,1.,-0.0760622897878246));
#44756=CARTESIAN_POINT('',(-3.74449296983004,1.,-0.2031560948961));
#44757=CARTESIAN_POINT('Ctrl Pts',(-3.74449296983004,-1.,-0.203156094896101));
#44758=CARTESIAN_POINT('Ctrl Pts',(-3.74449296983004,-0.666666666666667,
-0.203156094896101));
#44759=CARTESIAN_POINT('Ctrl Pts',(-3.74449296983004,-0.333333333333333,
-0.203156094896101));
#44760=CARTESIAN_POINT('Ctrl Pts',(-3.74449296983004,0.333333333333333,
-0.203156094896101));
#44761=CARTESIAN_POINT('Ctrl Pts',(-3.74449296983004,0.666666666666667,
-0.203156094896101));
#44762=CARTESIAN_POINT('Ctrl Pts',(-3.74449296983004,1.,-0.203156094896101));
#44763=CARTESIAN_POINT('',(-4.19931119685982,1.,-0.0760622897878246));
#44764=CARTESIAN_POINT('',(-4.19931119685982,0.,-0.0760622897878246));
#44765=CARTESIAN_POINT('Ctrl Pts',(-3.74449296983004,1.,-0.203156094896101));
#44766=CARTESIAN_POINT('Ctrl Pts',(-3.74453008995092,1.,-0.203188003946657));
#44767=CARTESIAN_POINT('Ctrl Pts',(-3.74471097893844,1.,-0.203266610110531));
#44768=CARTESIAN_POINT('Ctrl Pts',(-3.74535749969115,1.,-0.203375226874121));
#44769=CARTESIAN_POINT('Ctrl Pts',(-3.74703926501752,1.,-0.203484186269415));
#44770=CARTESIAN_POINT('Ctrl Pts',(-3.75054693397875,1.,-0.203550035479166));
#44771=CARTESIAN_POINT('Ctrl Pts',(-3.75585118707734,1.,-0.203530796848322));
#44772=CARTESIAN_POINT('Ctrl Pts',(-3.76242717936885,1.,-0.203414634707478));
#44773=CARTESIAN_POINT('Ctrl Pts',(-3.7699207159487,1.,-0.203192390045164));
#44774=CARTESIAN_POINT('Ctrl Pts',(-3.77793553476614,1.,-0.202854729699081));
#44775=CARTESIAN_POINT('Ctrl Pts',(-3.78609175019242,1.,-0.20239426051216));
#44776=CARTESIAN_POINT('Ctrl Pts',(-3.7940835418736,1.,-0.201807533800837));
#44777=CARTESIAN_POINT('Ctrl Pts',(-3.80175247447337,1.,-0.201097756307326));
#44778=CARTESIAN_POINT('Ctrl Pts',(-3.80909529318669,1.,-0.200274679433364));
#44779=CARTESIAN_POINT('Ctrl Pts',(-3.81620203429815,1.,-0.199351525297447));
#44780=CARTESIAN_POINT('Ctrl Pts',(-3.82321127349016,1.,-0.198342616900486));
#44781=CARTESIAN_POINT('Ctrl Pts',(-3.83026221776456,1.,-0.197260935827361));
#44782=CARTESIAN_POINT('Ctrl Pts',(-3.83743910616195,1.,-0.196115198971859));
#44783=CARTESIAN_POINT('Ctrl Pts',(-3.84475203346977,1.,-0.194909009460221));
#44784=CARTESIAN_POINT('Ctrl Pts',(-3.85216762263966,1.,-0.193642806777723));
#44785=CARTESIAN_POINT('Ctrl Pts',(-3.85962774407633,1.,-0.192315153044971));
#44786=CARTESIAN_POINT('Ctrl Pts',(-3.86707158624783,1.,-0.19092419041862));
#44787=CARTESIAN_POINT('Ctrl Pts',(-3.87445976418412,1.,-0.189469253358272));
#44788=CARTESIAN_POINT('Ctrl Pts',(-3.88178563496228,1.,-0.187951632512685));
#44789=CARTESIAN_POINT('Ctrl Pts',(-3.88906196725848,1.,-0.18637372498528));
#44790=CARTESIAN_POINT('Ctrl Pts',(-3.89631300742646,1.,-0.184738537728043));
#44791=CARTESIAN_POINT('Ctrl Pts',(-3.90356488555132,1.,-0.183049081993191));
#44792=CARTESIAN_POINT('Ctrl Pts',(-3.91083557557175,1.,-0.181307740731786));
#44793=CARTESIAN_POINT('Ctrl Pts',(-3.91812876180926,1.,-0.179515885822882));
#44794=CARTESIAN_POINT('Ctrl Pts',(-3.92543942697655,1.,-0.177674246152317));
#44795=CARTESIAN_POINT('Ctrl Pts',(-3.93275726771042,1.,-0.175783136893868));
#44796=CARTESIAN_POINT('Ctrl Pts',(-3.94007083096217,1.,-0.17384273497461));
#44797=CARTESIAN_POINT('Ctrl Pts',(-3.94737164900868,1.,-0.17185335536924));
#44798=CARTESIAN_POINT('Ctrl Pts',(-3.95465744665268,1.,-0.169815666374139));
#44799=CARTESIAN_POINT('Ctrl Pts',(-3.96192990160296,1.,-0.167730547023319));
#44800=CARTESIAN_POINT('Ctrl Pts',(-3.96919313621407,1.,-0.165598992851102));
#44801=CARTESIAN_POINT('Ctrl Pts',(-3.97645194630943,1.,-0.163422004609999));
#44802=CARTESIAN_POINT('Ctrl Pts',(-3.98371010319872,1.,-0.161200482186085));
#44803=CARTESIAN_POINT('Ctrl Pts',(-3.99096873945878,1.,-0.158935123982793));
#44804=CARTESIAN_POINT('Ctrl Pts',(-3.99822717425893,1.,-0.156626481393734));
#44805=CARTESIAN_POINT('Ctrl Pts',(-4.00548360245319,1.,-0.154275004872311));
#44806=CARTESIAN_POINT('Ctrl Pts',(-4.01273584234689,1.,-0.151881094022911));
#44807=CARTESIAN_POINT('Ctrl Pts',(-4.01998203715564,1.,-0.149445144968707));
#44808=CARTESIAN_POINT('Ctrl Pts',(-4.02722143146994,1.,-0.146967602878994));
#44809=CARTESIAN_POINT('Ctrl Pts',(-4.03445411510333,1.,-0.144448947038345));
#44810=CARTESIAN_POINT('Ctrl Pts',(-4.04168069633781,1.,-0.1418896714855));
#44811=CARTESIAN_POINT('Ctrl Pts',(-4.04890199238036,1.,-0.139290267180057));
#44812=CARTESIAN_POINT('Ctrl Pts',(-4.05611873400172,1.,-0.136651205046119));
#44813=CARTESIAN_POINT('Ctrl Pts',(-4.06333121018596,1.,-0.133972916144245));
#44814=CARTESIAN_POINT('Ctrl Pts',(-4.0705393152874,1.,-0.13125579354894));
#44815=CARTESIAN_POINT('Ctrl Pts',(-4.07774270738954,1.,-0.128500200484838));
#44816=CARTESIAN_POINT('Ctrl Pts',(-4.08494093372377,1.,-0.12570647682254));
#44817=CARTESIAN_POINT('Ctrl Pts',(-4.09213355850756,1.,-0.122874946249107));
#44818=CARTESIAN_POINT('Ctrl Pts',(-4.09932031767002,1.,-0.120005924388124));
#44819=CARTESIAN_POINT('Ctrl Pts',(-4.10650113381833,1.,-0.117099722731648));
#44820=CARTESIAN_POINT('Ctrl Pts',(-4.11367603924961,1.,-0.114156649609546));
#44821=CARTESIAN_POINT('Ctrl Pts',(-4.1208451250225,1.,-0.111177012683347));
#44822=CARTESIAN_POINT('Ctrl Pts',(-4.12800848371504,1.,-0.108161120528369));
#44823=CARTESIAN_POINT('Ctrl Pts',(-4.13516614458895,1.,-0.105109286538945));
#44824=CARTESIAN_POINT('Ctrl Pts',(-4.14231804939538,1.,-0.102021826577584));
#44825=CARTESIAN_POINT('Ctrl Pts',(-4.14946408918485,1.,-0.0988990478901226));
#44826=CARTESIAN_POINT('Ctrl Pts',(-4.15660412653577,1.,-0.0957412403298007));
#44827=CARTESIAN_POINT('Ctrl Pts',(-4.16373802265839,1.,-0.0925486672167531));
#44828=CARTESIAN_POINT('Ctrl Pts',(-4.17086566490794,1.,-0.0893215560848649));
#44829=CARTESIAN_POINT('Ctrl Pts',(-4.17798698668094,1.,-0.0860600915549397));
#44830=CARTESIAN_POINT('Ctrl Pts',(-4.18510195327123,1.,-0.0827644164385679));
#44831=CARTESIAN_POINT('Ctrl Pts',(-4.19078883320504,1.,-0.080100588711432));
#44832=CARTESIAN_POINT('Ctrl Pts',(-4.19505112859416,1.,-0.0780873956242397));
#44833=CARTESIAN_POINT('Ctrl Pts',(-4.1978913862118,1.,-0.0767384596141464));
#44834=CARTESIAN_POINT('Ctrl Pts',(-4.19931119685982,1.,-0.0760622897878246));
#44835=CARTESIAN_POINT('Origin',(-4.19931119685982,0.,-0.0760622897878246));
#44836=CARTESIAN_POINT('',(-4.19931119685982,1.,0.0760622897878236));
#44837=CARTESIAN_POINT('Origin',(0.,0.,0.));
#44838=CARTESIAN_POINT('',(-3.73017266276651,1.,-0.385112848330761));
#44839=CARTESIAN_POINT('Origin',(0.,1.,0.));
#44840=CARTESIAN_POINT('Ctrl Pts',(-3.73017266276651,1.,-0.385112848330762));
#44841=CARTESIAN_POINT('Ctrl Pts',(-3.73017266276651,0.666666666666667,
-0.385112848330762));
#44842=CARTESIAN_POINT('Ctrl Pts',(-3.73017266276651,0.333333333333333,
-0.385112848330762));
#44843=CARTESIAN_POINT('Ctrl Pts',(-3.73017266276651,-0.333333333333333,
-0.385112848330762));
#44844=CARTESIAN_POINT('Ctrl Pts',(-3.73017266276651,-0.666666666666667,
-0.385112848330762));
#44845=CARTESIAN_POINT('Ctrl Pts',(-3.73017266276651,-1.,-0.385112848330762));
#44846=CARTESIAN_POINT('Ctrl Pts',(-4.15950947128175,-1.,-0.581791163835815));
#44847=CARTESIAN_POINT('Ctrl Pts',(-4.15950947128175,1.,-0.581791163835815));
#44848=CARTESIAN_POINT('Ctrl Pts',(-4.1582129171283,-1.,-0.580901211463535));
#44849=CARTESIAN_POINT('Ctrl Pts',(-4.1582129171283,1.,-0.580901211463535));
#44850=CARTESIAN_POINT('Ctrl Pts',(-4.15561864788576,-1.,-0.579124568914235));
#44851=CARTESIAN_POINT('Ctrl Pts',(-4.15561864788576,1.,-0.579124568914235));
#44852=CARTESIAN_POINT('Ctrl Pts',(-4.151723761217,-1.,-0.576469391676688));
#44853=CARTESIAN_POINT('Ctrl Pts',(-4.151723761217,1.,-0.576469391676688));
#44854=CARTESIAN_POINT('Ctrl Pts',(-4.14652361068081,-1.,-0.572948736069522));
#44855=CARTESIAN_POINT('Ctrl Pts',(-4.14652361068081,1.,-0.572948736069522));
#44856=CARTESIAN_POINT('Ctrl Pts',(-4.14001179830547,-1.,-0.568580610189774));
#44857=CARTESIAN_POINT('Ctrl Pts',(-4.14001179830547,1.,-0.568580610189774));
#44858=CARTESIAN_POINT('Ctrl Pts',(-4.13348835727104,-1.,-0.564245279537148));
#44859=CARTESIAN_POINT('Ctrl Pts',(-4.13348835727104,1.,-0.564245279537148));
#44860=CARTESIAN_POINT('Ctrl Pts',(-4.12695329951961,-1.,-0.559942890594773));
#44861=CARTESIAN_POINT('Ctrl Pts',(-4.12695329951961,1.,-0.559942890594773));
#44862=CARTESIAN_POINT('Ctrl Pts',(-4.12040666195664,-1.,-0.555673636129977));
#44863=CARTESIAN_POINT('Ctrl Pts',(-4.12040666195664,1.,-0.555673636129977));
#44864=CARTESIAN_POINT('Ctrl Pts',(-4.11384852024721,-1.,-0.551437758497032));
#44865=CARTESIAN_POINT('Ctrl Pts',(-4.11384852024721,1.,-0.551437758497032));
#44866=CARTESIAN_POINT('Ctrl Pts',(-4.10727897027977,-1.,-0.547235539485637));
#44867=CARTESIAN_POINT('Ctrl Pts',(-4.10727897027977,1.,-0.547235539485637));
#44868=CARTESIAN_POINT('Ctrl Pts',(-4.10069810243979,-1.,-0.543067286877757));
#44869=CARTESIAN_POINT('Ctrl Pts',(-4.10069810243979,1.,-0.543067286877757));
#44870=CARTESIAN_POINT('Ctrl Pts',(-4.09410597627,-1.,-0.538933321179756));
#44871=CARTESIAN_POINT('Ctrl Pts',(-4.09410597627,1.,-0.538933321179756));
#44872=CARTESIAN_POINT('Ctrl Pts',(-4.08750259988885,-1.,-0.534833963477273));
#44873=CARTESIAN_POINT('Ctrl Pts',(-4.08750259988885,1.,-0.534833963477273));
#44874=CARTESIAN_POINT('Ctrl Pts',(-4.08088789536836,-1.,-0.530769518728571));
#44875=CARTESIAN_POINT('Ctrl Pts',(-4.08088789536836,1.,-0.530769518728571));
#44876=CARTESIAN_POINT('Ctrl Pts',(-4.07426172299847,-1.,-0.526740277227498));
#44877=CARTESIAN_POINT('Ctrl Pts',(-4.07426172299847,1.,-0.526740277227498));
#44878=CARTESIAN_POINT('Ctrl Pts',(-4.06762394471314,-1.,-0.522746528603107));
#44879=CARTESIAN_POINT('Ctrl Pts',(-4.06762394471314,1.,-0.522746528603107));
#44880=CARTESIAN_POINT('Ctrl Pts',(-4.06097448038013,-1.,-0.518788572336923));
#44881=CARTESIAN_POINT('Ctrl Pts',(-4.06097448038013,1.,-0.518788572336923));
#44882=CARTESIAN_POINT('Ctrl Pts',(-4.05431335771199,-1.,-0.514866728193017));
#44883=CARTESIAN_POINT('Ctrl Pts',(-4.05431335771199,1.,-0.514866728193017));
#44884=CARTESIAN_POINT('Ctrl Pts',(-4.04764078815447,-1.,-0.51098134921897));
#44885=CARTESIAN_POINT('Ctrl Pts',(-4.04764078815447,1.,-0.51098134921897));
#44886=CARTESIAN_POINT('Ctrl Pts',(-4.04095715148915,-1.,-0.507132823288136));
#44887=CARTESIAN_POINT('Ctrl Pts',(-4.04095715148915,1.,-0.507132823288136));
#44888=CARTESIAN_POINT('Ctrl Pts',(-4.03426284174272,-1.,-0.503321556915346));
#44889=CARTESIAN_POINT('Ctrl Pts',(-4.03426284174272,1.,-0.503321556915346));
#44890=CARTESIAN_POINT('Ctrl Pts',(-4.02755813980101,-1.,-0.499547962340821));
#44891=CARTESIAN_POINT('Ctrl Pts',(-4.02755813980101,1.,-0.499547962340821));
#44892=CARTESIAN_POINT('Ctrl Pts',(-4.02084308851832,-1.,-0.495812444326251));
#44893=CARTESIAN_POINT('Ctrl Pts',(-4.02084308851832,1.,-0.495812444326251));
#44894=CARTESIAN_POINT('Ctrl Pts',(-4.01411733503546,-1.,-0.492115383418018));
#44895=CARTESIAN_POINT('Ctrl Pts',(-4.01411733503546,1.,-0.492115383418018));
#44896=CARTESIAN_POINT('Ctrl Pts',(-4.0073800839099,-1.,-0.488457130424633));
#44897=CARTESIAN_POINT('Ctrl Pts',(-4.0073800839099,1.,-0.488457130424633));
#44898=CARTESIAN_POINT('Ctrl Pts',(-4.00063045119288,-1.,-0.484838042421835));
#44899=CARTESIAN_POINT('Ctrl Pts',(-4.00063045119288,1.,-0.484838042421835));
#44900=CARTESIAN_POINT('Ctrl Pts',(-3.99386775880679,-1.,-0.481258512209675));
#44901=CARTESIAN_POINT('Ctrl Pts',(-3.99386775880679,1.,-0.481258512209675));
#44902=CARTESIAN_POINT('Ctrl Pts',(-3.98709184306738,-1.,-0.477718999122027));
#44903=CARTESIAN_POINT('Ctrl Pts',(-3.98709184306738,1.,-0.477718999122027));
#44904=CARTESIAN_POINT('Ctrl Pts',(-3.98030338044409,-1.,-0.47422006101951));
#44905=CARTESIAN_POINT('Ctrl Pts',(-3.98030338044409,1.,-0.47422006101951));
#44906=CARTESIAN_POINT('Ctrl Pts',(-3.97350414289392,-1.,-0.470762379613439));
#44907=CARTESIAN_POINT('Ctrl Pts',(-3.97350414289392,1.,-0.470762379613439));
#44908=CARTESIAN_POINT('Ctrl Pts',(-3.9666962227393,-1.,-0.467346690880643));
#44909=CARTESIAN_POINT('Ctrl Pts',(-3.9666962227393,1.,-0.467346690880643));
#44910=CARTESIAN_POINT('Ctrl Pts',(-3.95988133243538,-1.,-0.463973722115733));
#44911=CARTESIAN_POINT('Ctrl Pts',(-3.95988133243538,1.,-0.463973722115733));
#44912=CARTESIAN_POINT('Ctrl Pts',(-3.95306005817364,-1.,-0.460644124429121));
#44913=CARTESIAN_POINT('Ctrl Pts',(-3.95306005817364,1.,-0.460644124429121));
#44914=CARTESIAN_POINT('Ctrl Pts',(-3.94623117206678,-1.,-0.457358410451683));
#44915=CARTESIAN_POINT('Ctrl Pts',(-3.94623117206678,1.,-0.457358410451683));
#44916=CARTESIAN_POINT('Ctrl Pts',(-3.93939080846298,-1.,-0.454116879027584));
#44917=CARTESIAN_POINT('Ctrl Pts',(-3.93939080846298,1.,-0.454116879027584));
#44918=CARTESIAN_POINT('Ctrl Pts',(-3.93253407403123,-1.,-0.450919768356348));
#44919=CARTESIAN_POINT('Ctrl Pts',(-3.93253407403123,1.,-0.450919768356348));
#44920=CARTESIAN_POINT('Ctrl Pts',(-3.92565674143416,-1.,-0.447767416837292));
#44921=CARTESIAN_POINT('Ctrl Pts',(-3.92565674143416,1.,-0.447767416837292));
#44922=CARTESIAN_POINT('Ctrl Pts',(-3.91875701610719,-1.,-0.444660430230591));
#44923=CARTESIAN_POINT('Ctrl Pts',(-3.91875701610719,1.,-0.444660430230591));
#44924=CARTESIAN_POINT('Ctrl Pts',(-3.91183704069153,-1.,-0.441599824524054));
#44925=CARTESIAN_POINT('Ctrl Pts',(-3.91183704069153,1.,-0.441599824524054));
#44926=CARTESIAN_POINT('Ctrl Pts',(-3.90490512938563,-1.,-0.438587235458249));
#44927=CARTESIAN_POINT('Ctrl Pts',(-3.90490512938563,1.,-0.438587235458249));
#44928=CARTESIAN_POINT('Ctrl Pts',(-3.89797256655462,-1.,-0.435624629433527));
#44929=CARTESIAN_POINT('Ctrl Pts',(-3.89797256655462,1.,-0.435624629433527));
#44930=CARTESIAN_POINT('Ctrl Pts',(-3.89104947940611,-1.,-0.432713929544458));
#44931=CARTESIAN_POINT('Ctrl Pts',(-3.89104947940611,1.,-0.432713929544458));
#44932=CARTESIAN_POINT('Ctrl Pts',(-3.88414070943341,-1.,-0.429856640579741));
#44933=CARTESIAN_POINT('Ctrl Pts',(-3.88414070943341,1.,-0.429856640579741));
#44934=CARTESIAN_POINT('Ctrl Pts',(-3.87724240306597,-1.,-0.427053541173457));
#44935=CARTESIAN_POINT('Ctrl Pts',(-3.87724240306597,1.,-0.427053541173457));
#44936=CARTESIAN_POINT('Ctrl Pts',(-3.87033643487851,-1.,-0.424304173195111));
#44937=CARTESIAN_POINT('Ctrl Pts',(-3.87033643487851,1.,-0.424304173195111));
#44938=CARTESIAN_POINT('Ctrl Pts',(-3.86339652542709,-1.,-0.421607423177534));
#44939=CARTESIAN_POINT('Ctrl Pts',(-3.86339652542709,1.,-0.421607423177534));
#44940=CARTESIAN_POINT('Ctrl Pts',(-3.85639825647996,-1.,-0.418962468086773));
#44941=CARTESIAN_POINT('Ctrl Pts',(-3.85639825647996,1.,-0.418962468086773));
#44942=CARTESIAN_POINT('Ctrl Pts',(-3.84932864157497,-1.,-0.416369678052907));
#44943=CARTESIAN_POINT('Ctrl Pts',(-3.84932864157497,1.,-0.416369678052907));
#44944=CARTESIAN_POINT('Ctrl Pts',(-3.84219403994762,-1.,-0.413831367016748));
#44945=CARTESIAN_POINT('Ctrl Pts',(-3.84219403994762,1.,-0.413831367016748));
#44946=CARTESIAN_POINT('Ctrl Pts',(-3.83503345578698,-1.,-0.411353038798518));
#44947=CARTESIAN_POINT('Ctrl Pts',(-3.83503345578698,1.,-0.411353038798518));
#44948=CARTESIAN_POINT('Ctrl Pts',(-3.82790724256471,-1.,-0.40894237144746));
#44949=CARTESIAN_POINT('Ctrl Pts',(-3.82790724256471,1.,-0.40894237144746));
#44950=CARTESIAN_POINT('Ctrl Pts',(-3.8208730391381,-1.,-0.406607038258985));
#44951=CARTESIAN_POINT('Ctrl Pts',(-3.8208730391381,1.,-0.406607038258985));
#44952=CARTESIAN_POINT('Ctrl Pts',(-3.81396374287793,-1.,-0.404352694628273));
#44953=CARTESIAN_POINT('Ctrl Pts',(-3.81396374287793,1.,-0.404352694628273));
#44954=CARTESIAN_POINT('Ctrl Pts',(-3.80716881962728,-1.,-0.402181320148436));
#44955=CARTESIAN_POINT('Ctrl Pts',(-3.80716881962728,1.,-0.402181320148436));
#44956=CARTESIAN_POINT('Ctrl Pts',(-3.80040370384546,-1.,-0.4000883465046));
#44957=CARTESIAN_POINT('Ctrl Pts',(-3.80040370384546,1.,-0.4000883465046));
#44958=CARTESIAN_POINT('Ctrl Pts',(-3.7935288716329,-1.,-0.398064818683969));
#44959=CARTESIAN_POINT('Ctrl Pts',(-3.7935288716329,1.,-0.398064818683969));
#44960=CARTESIAN_POINT('Ctrl Pts',(-3.78640521279313,-1.,-0.396103205334841));
#44961=CARTESIAN_POINT('Ctrl Pts',(-3.78640521279313,1.,-0.396103205334841));
#44962=CARTESIAN_POINT('Ctrl Pts',(-3.77894173114283,-1.,-0.394202481011499));
#44963=CARTESIAN_POINT('Ctrl Pts',(-3.77894173114283,1.,-0.394202481011499));
#44964=CARTESIAN_POINT('Ctrl Pts',(-3.77114011595967,-1.,-0.392372786223432));
#44965=CARTESIAN_POINT('Ctrl Pts',(-3.77114011595967,1.,-0.392372786223432));
#44966=CARTESIAN_POINT('Ctrl Pts',(-3.76315635033257,-1.,-0.39064207297956));
#44967=CARTESIAN_POINT('Ctrl Pts',(-3.76315635033257,1.,-0.39064207297956));
#44968=CARTESIAN_POINT('Ctrl Pts',(-3.75529302895152,-1.,-0.389054775898702));
#44969=CARTESIAN_POINT('Ctrl Pts',(-3.75529302895152,1.,-0.389054775898702));
#44970=CARTESIAN_POINT('Ctrl Pts',(-3.74792651696654,-1.,-0.387663020050836));
#44971=CARTESIAN_POINT('Ctrl Pts',(-3.74792651696654,1.,-0.387663020050836));
#44972=CARTESIAN_POINT('Ctrl Pts',(-3.74144965781276,-1.,-0.386519576222251));
#44973=CARTESIAN_POINT('Ctrl Pts',(-3.74144965781276,1.,-0.386519576222251));
#44974=CARTESIAN_POINT('Ctrl Pts',(-3.73621371845318,-1.,-0.385670806454566));
#44975=CARTESIAN_POINT('Ctrl Pts',(-3.73621371845318,1.,-0.385670806454566));
#44976=CARTESIAN_POINT('Ctrl Pts',(-3.73245705638843,-1.,-0.385147887988951));
#44977=CARTESIAN_POINT('Ctrl Pts',(-3.73245705638843,1.,-0.385147887988951));
#44978=CARTESIAN_POINT('Ctrl Pts',(-3.73072465900175,-1.,-0.385001870183213));
#44979=CARTESIAN_POINT('Ctrl Pts',(-3.73072465900175,1.,-0.385001870183213));
#44980=CARTESIAN_POINT('Ctrl Pts',(-3.73015851028356,-1.,-0.385047711603462));
#44981=CARTESIAN_POINT('Ctrl Pts',(-3.73015851028356,1.,-0.385047711603462));
#44982=CARTESIAN_POINT('Ctrl Pts',(-3.73010668803042,-1.,-0.385147278814642));
#44983=CARTESIAN_POINT('Ctrl Pts',(-3.73010668803042,1.,-0.385147278814642));
#44984=CARTESIAN_POINT('Ctrl Pts',(-3.73016218570874,-1.,-0.38521431477633));
#44985=CARTESIAN_POINT('Ctrl Pts',(-3.73016218570874,1.,-0.38521431477633));
#44986=CARTESIAN_POINT('',(-4.15950947128175,1.,-0.581791163835815));
#44987=CARTESIAN_POINT('Ctrl Pts',(-4.15950947128175,1.,-0.581791163835815));
#44988=CARTESIAN_POINT('Ctrl Pts',(-4.1582129171283,1.,-0.580901211463535));
#44989=CARTESIAN_POINT('Ctrl Pts',(-4.15561864788576,1.,-0.579124568914235));
#44990=CARTESIAN_POINT('Ctrl Pts',(-4.151723761217,1.,-0.576469391676688));
#44991=CARTESIAN_POINT('Ctrl Pts',(-4.14652361068081,1.,-0.572948736069522));
#44992=CARTESIAN_POINT('Ctrl Pts',(-4.14001179830547,1.,-0.568580610189774));
#44993=CARTESIAN_POINT('Ctrl Pts',(-4.13348835727104,1.,-0.564245279537148));
#44994=CARTESIAN_POINT('Ctrl Pts',(-4.12695329951961,1.,-0.559942890594773));
#44995=CARTESIAN_POINT('Ctrl Pts',(-4.12040666195664,1.,-0.555673636129977));
#44996=CARTESIAN_POINT('Ctrl Pts',(-4.11384852024721,1.,-0.551437758497032));
#44997=CARTESIAN_POINT('Ctrl Pts',(-4.10727897027977,1.,-0.547235539485637));
#44998=CARTESIAN_POINT('Ctrl Pts',(-4.10069810243979,1.,-0.543067286877757));
#44999=CARTESIAN_POINT('Ctrl Pts',(-4.09410597627,1.,-0.538933321179756));
#45000=CARTESIAN_POINT('Ctrl Pts',(-4.08750259988885,1.,-0.534833963477273));
#45001=CARTESIAN_POINT('Ctrl Pts',(-4.08088789536836,1.,-0.530769518728571));
#45002=CARTESIAN_POINT('Ctrl Pts',(-4.07426172299847,1.,-0.526740277227498));
#45003=CARTESIAN_POINT('Ctrl Pts',(-4.06762394471314,1.,-0.522746528603107));
#45004=CARTESIAN_POINT('Ctrl Pts',(-4.06097448038013,1.,-0.518788572336923));
#45005=CARTESIAN_POINT('Ctrl Pts',(-4.05431335771199,1.,-0.514866728193017));
#45006=CARTESIAN_POINT('Ctrl Pts',(-4.04764078815447,1.,-0.51098134921897));
#45007=CARTESIAN_POINT('Ctrl Pts',(-4.04095715148915,1.,-0.507132823288136));
#45008=CARTESIAN_POINT('Ctrl Pts',(-4.03426284174272,1.,-0.503321556915346));
#45009=CARTESIAN_POINT('Ctrl Pts',(-4.02755813980101,1.,-0.499547962340821));
#45010=CARTESIAN_POINT('Ctrl Pts',(-4.02084308851832,1.,-0.495812444326251));
#45011=CARTESIAN_POINT('Ctrl Pts',(-4.01411733503546,1.,-0.492115383418018));
#45012=CARTESIAN_POINT('Ctrl Pts',(-4.0073800839099,1.,-0.488457130424633));
#45013=CARTESIAN_POINT('Ctrl Pts',(-4.00063045119288,1.,-0.484838042421835));
#45014=CARTESIAN_POINT('Ctrl Pts',(-3.99386775880679,1.,-0.481258512209675));
#45015=CARTESIAN_POINT('Ctrl Pts',(-3.98709184306738,1.,-0.477718999122027));
#45016=CARTESIAN_POINT('Ctrl Pts',(-3.98030338044409,1.,-0.47422006101951));
#45017=CARTESIAN_POINT('Ctrl Pts',(-3.97350414289392,1.,-0.470762379613439));
#45018=CARTESIAN_POINT('Ctrl Pts',(-3.9666962227393,1.,-0.467346690880643));
#45019=CARTESIAN_POINT('Ctrl Pts',(-3.95988133243538,1.,-0.463973722115733));
#45020=CARTESIAN_POINT('Ctrl Pts',(-3.95306005817364,1.,-0.460644124429121));
#45021=CARTESIAN_POINT('Ctrl Pts',(-3.94623117206678,1.,-0.457358410451683));
#45022=CARTESIAN_POINT('Ctrl Pts',(-3.93939080846298,1.,-0.454116879027584));
#45023=CARTESIAN_POINT('Ctrl Pts',(-3.93253407403123,1.,-0.450919768356348));
#45024=CARTESIAN_POINT('Ctrl Pts',(-3.92565674143416,1.,-0.447767416837292));
#45025=CARTESIAN_POINT('Ctrl Pts',(-3.91875701610719,1.,-0.444660430230591));
#45026=CARTESIAN_POINT('Ctrl Pts',(-3.91183704069153,1.,-0.441599824524054));
#45027=CARTESIAN_POINT('Ctrl Pts',(-3.90490512938563,1.,-0.438587235458249));
#45028=CARTESIAN_POINT('Ctrl Pts',(-3.89797256655462,1.,-0.435624629433527));
#45029=CARTESIAN_POINT('Ctrl Pts',(-3.89104947940611,1.,-0.432713929544458));
#45030=CARTESIAN_POINT('Ctrl Pts',(-3.88414070943341,1.,-0.429856640579741));
#45031=CARTESIAN_POINT('Ctrl Pts',(-3.87724240306597,1.,-0.427053541173457));
#45032=CARTESIAN_POINT('Ctrl Pts',(-3.87033643487851,1.,-0.424304173195111));
#45033=CARTESIAN_POINT('Ctrl Pts',(-3.86339652542709,1.,-0.421607423177534));
#45034=CARTESIAN_POINT('Ctrl Pts',(-3.85639825647996,1.,-0.418962468086773));
#45035=CARTESIAN_POINT('Ctrl Pts',(-3.84932864157497,1.,-0.416369678052907));
#45036=CARTESIAN_POINT('Ctrl Pts',(-3.84219403994762,1.,-0.413831367016748));
#45037=CARTESIAN_POINT('Ctrl Pts',(-3.83503345578698,1.,-0.411353038798518));
#45038=CARTESIAN_POINT('Ctrl Pts',(-3.82790724256471,1.,-0.40894237144746));
#45039=CARTESIAN_POINT('Ctrl Pts',(-3.8208730391381,1.,-0.406607038258985));
#45040=CARTESIAN_POINT('Ctrl Pts',(-3.81396374287793,1.,-0.404352694628273));
#45041=CARTESIAN_POINT('Ctrl Pts',(-3.80716881962728,1.,-0.402181320148436));
#45042=CARTESIAN_POINT('Ctrl Pts',(-3.80040370384546,1.,-0.4000883465046));
#45043=CARTESIAN_POINT('Ctrl Pts',(-3.7935288716329,1.,-0.398064818683969));
#45044=CARTESIAN_POINT('Ctrl Pts',(-3.78640521279313,1.,-0.396103205334841));
#45045=CARTESIAN_POINT('Ctrl Pts',(-3.77894173114283,1.,-0.394202481011499));
#45046=CARTESIAN_POINT('Ctrl Pts',(-3.77114011595967,1.,-0.392372786223432));
#45047=CARTESIAN_POINT('Ctrl Pts',(-3.76315635033257,1.,-0.39064207297956));
#45048=CARTESIAN_POINT('Ctrl Pts',(-3.75529302895152,1.,-0.389054775898702));
#45049=CARTESIAN_POINT('Ctrl Pts',(-3.74792651696654,1.,-0.387663020050836));
#45050=CARTESIAN_POINT('Ctrl Pts',(-3.74144965781276,1.,-0.386519576222251));
#45051=CARTESIAN_POINT('Ctrl Pts',(-3.73621371845318,1.,-0.385670806454566));
#45052=CARTESIAN_POINT('Ctrl Pts',(-3.73273893363406,1.,-0.385187124634206));
#45053=CARTESIAN_POINT('Ctrl Pts',(-3.73106082862548,1.,-0.385031656499164));
#45054=CARTESIAN_POINT('Ctrl Pts',(-3.73040527621055,1.,-0.385037797881504));
#45055=CARTESIAN_POINT('Ctrl Pts',(-3.73021431755274,1.,-0.385087139000374));
#45056=CARTESIAN_POINT('Ctrl Pts',(-3.73017266276651,1.,-0.385112848330762));
#45057=CARTESIAN_POINT('',(-4.15950947128175,0.,-0.581791163835815));
#45058=CARTESIAN_POINT('Ctrl Pts',(-3.66663282329846,-1.,-0.7863229229206));
#45059=CARTESIAN_POINT('Ctrl Pts',(-3.66663282329846,1.,-0.7863229229206));
#45060=CARTESIAN_POINT('Ctrl Pts',(-3.66655932661986,-1.,-0.786369528183326));
#45061=CARTESIAN_POINT('Ctrl Pts',(-3.66655932661986,1.,-0.786369528183326));
#45062=CARTESIAN_POINT('Ctrl Pts',(-3.66657784455334,-1.,-0.786480236185696));
#45063=CARTESIAN_POINT('Ctrl Pts',(-3.66657784455334,1.,-0.786480236185696));
#45064=CARTESIAN_POINT('Ctrl Pts',(-3.66710211820482,-1.,-0.786698783542764));
#45065=CARTESIAN_POINT('Ctrl Pts',(-3.66710211820482,1.,-0.786698783542764));
#45066=CARTESIAN_POINT('Ctrl Pts',(-3.66879484801113,-1.,-0.787095252590501));
#45067=CARTESIAN_POINT('Ctrl Pts',(-3.66879484801113,1.,-0.787095252590501));
#45068=CARTESIAN_POINT('Ctrl Pts',(-3.67252923663655,-1.,-0.787758799995742));
#45069=CARTESIAN_POINT('Ctrl Pts',(-3.67252923663655,1.,-0.787758799995742));
#45070=CARTESIAN_POINT('Ctrl Pts',(-3.67777119516252,-1.,-0.788569566220285));
#45071=CARTESIAN_POINT('Ctrl Pts',(-3.67777119516252,1.,-0.788569566220285));
#45072=CARTESIAN_POINT('Ctrl Pts',(-3.68428439783905,-1.,-0.789483546064387));
#45073=CARTESIAN_POINT('Ctrl Pts',(-3.68428439783905,1.,-0.789483546064387));
#45074=CARTESIAN_POINT('Ctrl Pts',(-3.69172044327364,-1.,-0.790436284988787));
#45075=CARTESIAN_POINT('Ctrl Pts',(-3.69172044327364,1.,-0.790436284988787));
#45076=CARTESIAN_POINT('Ctrl Pts',(-3.69968940808721,-1.,-0.79135657569598));
#45077=CARTESIAN_POINT('Ctrl Pts',(-3.69968940808721,1.,-0.79135657569598));
#45078=CARTESIAN_POINT('Ctrl Pts',(-3.70781724021806,-1.,-0.792177688845818));
#45079=CARTESIAN_POINT('Ctrl Pts',(-3.70781724021806,1.,-0.792177688845818));
#45080=CARTESIAN_POINT('Ctrl Pts',(-3.71580242396124,-1.,-0.792848377370287));
#45081=CARTESIAN_POINT('Ctrl Pts',(-3.71580242396124,1.,-0.792848377370287));
#45082=CARTESIAN_POINT('Ctrl Pts',(-3.72348797293734,-1.,-0.793347023784205));
#45083=CARTESIAN_POINT('Ctrl Pts',(-3.72348797293734,1.,-0.793347023784205));
#45084=CARTESIAN_POINT('Ctrl Pts',(-3.73086914695805,-1.,-0.793682750269684));
#45085=CARTESIAN_POINT('Ctrl Pts',(-3.73086914695805,1.,-0.793682750269684));
#45086=CARTESIAN_POINT('Ctrl Pts',(-3.73803280541687,-1.,-0.793882700937017));
#45087=CARTESIAN_POINT('Ctrl Pts',(-3.73803280541687,1.,-0.793882700937017));
#45088=CARTESIAN_POINT('Ctrl Pts',(-3.74511357728861,-1.,-0.793982700459952));
#45089=CARTESIAN_POINT('Ctrl Pts',(-3.74511357728861,1.,-0.793982700459952));
#45090=CARTESIAN_POINT('Ctrl Pts',(-3.75224692493864,-1.,-0.794017347371377));
#45091=CARTESIAN_POINT('Ctrl Pts',(-3.75224692493864,1.,-0.794017347371377));
#45092=CARTESIAN_POINT('Ctrl Pts',(-3.75951468666257,-1.,-0.794008429134907));
#45093=CARTESIAN_POINT('Ctrl Pts',(-3.75951468666257,1.,-0.794008429134907));
#45094=CARTESIAN_POINT('Ctrl Pts',(-3.76692626931111,-1.,-0.793961083688991));
#45095=CARTESIAN_POINT('Ctrl Pts',(-3.76692626931111,1.,-0.793961083688991));
#45096=CARTESIAN_POINT('Ctrl Pts',(-3.77444863801212,-1.,-0.793870523787408));
#45097=CARTESIAN_POINT('Ctrl Pts',(-3.77444863801212,1.,-0.793870523787408));
#45098=CARTESIAN_POINT('Ctrl Pts',(-3.78202460377598,-1.,-0.7937262357813));
#45099=CARTESIAN_POINT('Ctrl Pts',(-3.78202460377598,1.,-0.7937262357813));
#45100=CARTESIAN_POINT('Ctrl Pts',(-3.78959439439235,-1.,-0.793516871680993));
#45101=CARTESIAN_POINT('Ctrl Pts',(-3.78959439439235,1.,-0.793516871680993));
#45102=CARTESIAN_POINT('Ctrl Pts',(-3.79711921389897,-1.,-0.793235612973273));
#45103=CARTESIAN_POINT('Ctrl Pts',(-3.79711921389897,1.,-0.793235612973273));
#45104=CARTESIAN_POINT('Ctrl Pts',(-3.80459229925637,-1.,-0.792882695234778));
#45105=CARTESIAN_POINT('Ctrl Pts',(-3.80459229925637,1.,-0.792882695234778));
#45106=CARTESIAN_POINT('Ctrl Pts',(-3.81202588694756,-1.,-0.792462483517634));
#45107=CARTESIAN_POINT('Ctrl Pts',(-3.81202588694756,1.,-0.792462483517634));
#45108=CARTESIAN_POINT('Ctrl Pts',(-3.81944345442249,-1.,-0.791981740718635));
#45109=CARTESIAN_POINT('Ctrl Pts',(-3.81944345442249,1.,-0.791981740718635));
#45110=CARTESIAN_POINT('Ctrl Pts',(-3.82687033899792,-1.,-0.791447528662369));
#45111=CARTESIAN_POINT('Ctrl Pts',(-3.82687033899792,1.,-0.791447528662369));
#45112=CARTESIAN_POINT('Ctrl Pts',(-3.83432392054786,-1.,-0.790865012705301));
#45113=CARTESIAN_POINT('Ctrl Pts',(-3.83432392054786,1.,-0.790865012705301));
#45114=CARTESIAN_POINT('Ctrl Pts',(-3.84180762342454,-1.,-0.790236124191242));
#45115=CARTESIAN_POINT('Ctrl Pts',(-3.84180762342454,1.,-0.790236124191242));
#45116=CARTESIAN_POINT('Ctrl Pts',(-3.84931637808894,-1.,-0.789560798155582));
#45117=CARTESIAN_POINT('Ctrl Pts',(-3.84931637808894,1.,-0.789560798155582));
#45118=CARTESIAN_POINT('Ctrl Pts',(-3.85683995872529,-1.,-0.788837734090672));
#45119=CARTESIAN_POINT('Ctrl Pts',(-3.85683995872529,1.,-0.788837734090672));
#45120=CARTESIAN_POINT('Ctrl Pts',(-3.86436702561345,-1.,-0.788065315093777));
#45121=CARTESIAN_POINT('Ctrl Pts',(-3.86436702561345,1.,-0.788065315093777));
#45122=CARTESIAN_POINT('Ctrl Pts',(-3.87188916600912,-1.,-0.787242527617999));
#45123=CARTESIAN_POINT('Ctrl Pts',(-3.87188916600912,1.,-0.787242527617999));
#45124=CARTESIAN_POINT('Ctrl Pts',(-3.8794040281819,-1.,-0.786369675812608));
#45125=CARTESIAN_POINT('Ctrl Pts',(-3.8794040281819,1.,-0.786369675812608));
#45126=CARTESIAN_POINT('Ctrl Pts',(-3.88691313167398,-1.,-0.78544789034073));
#45127=CARTESIAN_POINT('Ctrl Pts',(-3.88691313167398,1.,-0.78544789034073));
#45128=CARTESIAN_POINT('Ctrl Pts',(-3.89442039235103,-1.,-0.784478799358336));
#45129=CARTESIAN_POINT('Ctrl Pts',(-3.89442039235103,1.,-0.784478799358336));
#45130=CARTESIAN_POINT('Ctrl Pts',(-3.9019303904397,-1.,-0.783464141529081));
#45131=CARTESIAN_POINT('Ctrl Pts',(-3.9019303904397,1.,-0.783464141529081));
#45132=CARTESIAN_POINT('Ctrl Pts',(-3.90944671004542,-1.,-0.782405395622764));
#45133=CARTESIAN_POINT('Ctrl Pts',(-3.90944671004542,1.,-0.782405395622764));
#45134=CARTESIAN_POINT('Ctrl Pts',(-3.91697036054676,-1.,-0.781303428618366));
#45135=CARTESIAN_POINT('Ctrl Pts',(-3.91697036054676,1.,-0.781303428618366));
#45136=CARTESIAN_POINT('Ctrl Pts',(-3.92450058323823,-1.,-0.780158678615542));
#45137=CARTESIAN_POINT('Ctrl Pts',(-3.92450058323823,1.,-0.780158678615542));
#45138=CARTESIAN_POINT('Ctrl Pts',(-3.93203552473174,-1.,-0.778971308134821));
#45139=CARTESIAN_POINT('Ctrl Pts',(-3.93203552473174,1.,-0.778971308134821));
#45140=CARTESIAN_POINT('Ctrl Pts',(-3.93957296768103,-1.,-0.777741370568558));
#45141=CARTESIAN_POINT('Ctrl Pts',(-3.93957296768103,1.,-0.777741370568558));
#45142=CARTESIAN_POINT('Ctrl Pts',(-3.94711101619447,-1.,-0.776468966697921));
#45143=CARTESIAN_POINT('Ctrl Pts',(-3.94711101619447,1.,-0.776468966697921));
#45144=CARTESIAN_POINT('Ctrl Pts',(-3.9546488545231,-1.,-0.775154418039351));
#45145=CARTESIAN_POINT('Ctrl Pts',(-3.9546488545231,1.,-0.775154418039351));
#45146=CARTESIAN_POINT('Ctrl Pts',(-3.96218649639807,-1.,-0.773798212026565));
#45147=CARTESIAN_POINT('Ctrl Pts',(-3.96218649639807,1.,-0.773798212026565));
#45148=CARTESIAN_POINT('Ctrl Pts',(-3.96972446532772,-1.,-0.772400931772136));
#45149=CARTESIAN_POINT('Ctrl Pts',(-3.96972446532772,1.,-0.772400931772136));
#45150=CARTESIAN_POINT('Ctrl Pts',(-3.97726349165488,-1.,-0.770963190030471));
#45151=CARTESIAN_POINT('Ctrl Pts',(-3.97726349165488,1.,-0.770963190030471));
#45152=CARTESIAN_POINT('Ctrl Pts',(-3.98480422348451,-1.,-0.769485566245544));
#45153=CARTESIAN_POINT('Ctrl Pts',(-3.98480422348451,1.,-0.769485566245544));
#45154=CARTESIAN_POINT('Ctrl Pts',(-3.9923468788101,-1.,-0.767968531377915));
#45155=CARTESIAN_POINT('Ctrl Pts',(-3.9923468788101,1.,-0.767968531377915));
#45156=CARTESIAN_POINT('Ctrl Pts',(-3.99989129179622,-1.,-0.766412457136064));
#45157=CARTESIAN_POINT('Ctrl Pts',(-3.99989129179622,1.,-0.766412457136064));
#45158=CARTESIAN_POINT('Ctrl Pts',(-4.00743706791509,-1.,-0.764817648785197));
#45159=CARTESIAN_POINT('Ctrl Pts',(-4.00743706791509,1.,-0.764817648785197));
#45160=CARTESIAN_POINT('Ctrl Pts',(-4.01498370680496,-1.,-0.763184371182935));
#45161=CARTESIAN_POINT('Ctrl Pts',(-4.01498370680496,1.,-0.763184371182935));
#45162=CARTESIAN_POINT('Ctrl Pts',(-4.02253072741268,-1.,-0.761512875859804));
#45163=CARTESIAN_POINT('Ctrl Pts',(-4.02253072741268,1.,-0.761512875859804));
#45164=CARTESIAN_POINT('Ctrl Pts',(-4.03007781954412,-1.,-0.759803433243752));
#45165=CARTESIAN_POINT('Ctrl Pts',(-4.03007781954412,1.,-0.759803433243752));
#45166=CARTESIAN_POINT('Ctrl Pts',(-4.03762485803119,-1.,-0.758056338884944));
#45167=CARTESIAN_POINT('Ctrl Pts',(-4.03762485803119,1.,-0.758056338884944));
#45168=CARTESIAN_POINT('Ctrl Pts',(-4.04517182653997,-1.,-0.756271902369581));
#45169=CARTESIAN_POINT('Ctrl Pts',(-4.04517182653997,1.,-0.756271902369581));
#45170=CARTESIAN_POINT('Ctrl Pts',(-4.05271876687915,-1.,-0.754450441816078));
#45171=CARTESIAN_POINT('Ctrl Pts',(-4.05271876687915,1.,-0.754450441816078));
#45172=CARTESIAN_POINT('Ctrl Pts',(-4.06026572221515,-1.,-0.752592276483072));
#45173=CARTESIAN_POINT('Ctrl Pts',(-4.06026572221515,1.,-0.752592276483072));
#45174=CARTESIAN_POINT('Ctrl Pts',(-4.06781267242378,-1.,-0.750697720484036));
#45175=CARTESIAN_POINT('Ctrl Pts',(-4.06781267242378,1.,-0.750697720484036));
#45176=CARTESIAN_POINT('Ctrl Pts',(-4.07535951056152,-1.,-0.748767076680557));
#45177=CARTESIAN_POINT('Ctrl Pts',(-4.07535951056152,1.,-0.748767076680557));
#45178=CARTESIAN_POINT('Ctrl Pts',(-4.08290608095642,-1.,-0.746800631492315));
#45179=CARTESIAN_POINT('Ctrl Pts',(-4.08290608095642,1.,-0.746800631492315));
#45180=CARTESIAN_POINT('Ctrl Pts',(-4.09045220253573,-1.,-0.7447986497065));
#45181=CARTESIAN_POINT('Ctrl Pts',(-4.09045220253573,1.,-0.7447986497065));
#45182=CARTESIAN_POINT('Ctrl Pts',(-4.09799769702611,-1.,-0.742761369689841));
#45183=CARTESIAN_POINT('Ctrl Pts',(-4.09799769702611,1.,-0.742761369689841));
#45184=CARTESIAN_POINT('Ctrl Pts',(-4.10554241757547,-1.,-0.740688998553377));
#45185=CARTESIAN_POINT('Ctrl Pts',(-4.10554241757547,1.,-0.740688998553377));
#45186=CARTESIAN_POINT('Ctrl Pts',(-4.11308626951927,-1.,-0.738581708225844));
#45187=CARTESIAN_POINT('Ctrl Pts',(-4.11308626951927,1.,-0.738581708225844));
#45188=CARTESIAN_POINT('Ctrl Pts',(-4.120629196238,-1.,-0.736439634331345));
#45189=CARTESIAN_POINT('Ctrl Pts',(-4.120629196238,1.,-0.736439634331345));
#45190=CARTESIAN_POINT('Ctrl Pts',(-4.12666277570844,-1.,-0.734698226764092));
#45191=CARTESIAN_POINT('Ctrl Pts',(-4.12666277570844,1.,-0.734698226764092));
#45192=CARTESIAN_POINT('Ctrl Pts',(-4.13118752795207,-1.,-0.733376589323546));
#45193=CARTESIAN_POINT('Ctrl Pts',(-4.13118752795207,1.,-0.733376589323546));
#45194=CARTESIAN_POINT('Ctrl Pts',(-4.1342038373684,-1.,-0.732488575135159));
#45195=CARTESIAN_POINT('Ctrl Pts',(-4.1342038373684,1.,-0.732488575135159));
#45196=CARTESIAN_POINT('Ctrl Pts',(-4.13571194405636,-1.,-0.73204283740062));
#45197=CARTESIAN_POINT('Ctrl Pts',(-4.13571194405636,1.,-0.73204283740062));
#45198=CARTESIAN_POINT('',(-3.66661143271685,1.,-0.786422660831985));
#45199=CARTESIAN_POINT('Ctrl Pts',(-3.66661143271685,-1.,-0.786422660831985));
#45200=CARTESIAN_POINT('Ctrl Pts',(-3.66661143271685,-0.666666666666667,
-0.786422660831985));
#45201=CARTESIAN_POINT('Ctrl Pts',(-3.66661143271685,-0.333333333333333,
-0.786422660831985));
#45202=CARTESIAN_POINT('Ctrl Pts',(-3.66661143271685,0.333333333333333,
-0.786422660831985));
#45203=CARTESIAN_POINT('Ctrl Pts',(-3.66661143271685,0.666666666666667,
-0.786422660831985));
#45204=CARTESIAN_POINT('Ctrl Pts',(-3.66661143271685,1.,-0.786422660831985));
#45205=CARTESIAN_POINT('',(-4.13571194405636,1.,-0.73204283740062));
#45206=CARTESIAN_POINT('',(-4.13571194405636,0.,-0.73204283740062));
#45207=CARTESIAN_POINT('Ctrl Pts',(-3.66661143271685,1.,-0.786422660831985));
#45208=CARTESIAN_POINT('Ctrl Pts',(-3.6666431041522,1.,-0.786459983895432));
#45209=CARTESIAN_POINT('Ctrl Pts',(-3.66680946938292,1.,-0.786565919558984));
#45210=CARTESIAN_POINT('Ctrl Pts',(-3.66743103898702,1.,-0.786774337198062));
#45211=CARTESIAN_POINT('Ctrl Pts',(-3.66907505398677,1.,-0.787145041181545));
#45212=CARTESIAN_POINT('Ctrl Pts',(-3.67252923663655,1.,-0.787758799995742));
#45213=CARTESIAN_POINT('Ctrl Pts',(-3.67777119516252,1.,-0.788569566220285));
#45214=CARTESIAN_POINT('Ctrl Pts',(-3.68428439783905,1.,-0.789483546064387));
#45215=CARTESIAN_POINT('Ctrl Pts',(-3.69172044327364,1.,-0.790436284988787));
#45216=CARTESIAN_POINT('Ctrl Pts',(-3.69968940808721,1.,-0.79135657569598));
#45217=CARTESIAN_POINT('Ctrl Pts',(-3.70781724021806,1.,-0.792177688845818));
#45218=CARTESIAN_POINT('Ctrl Pts',(-3.71580242396124,1.,-0.792848377370287));
#45219=CARTESIAN_POINT('Ctrl Pts',(-3.72348797293734,1.,-0.793347023784205));
#45220=CARTESIAN_POINT('Ctrl Pts',(-3.73086914695805,1.,-0.793682750269684));
#45221=CARTESIAN_POINT('Ctrl Pts',(-3.73803280541687,1.,-0.793882700937017));
#45222=CARTESIAN_POINT('Ctrl Pts',(-3.74511357728861,1.,-0.793982700459952));
#45223=CARTESIAN_POINT('Ctrl Pts',(-3.75224692493864,1.,-0.794017347371377));
#45224=CARTESIAN_POINT('Ctrl Pts',(-3.75951468666257,1.,-0.794008429134907));
#45225=CARTESIAN_POINT('Ctrl Pts',(-3.76692626931111,1.,-0.793961083688991));
#45226=CARTESIAN_POINT('Ctrl Pts',(-3.77444863801212,1.,-0.793870523787408));
#45227=CARTESIAN_POINT('Ctrl Pts',(-3.78202460377598,1.,-0.7937262357813));
#45228=CARTESIAN_POINT('Ctrl Pts',(-3.78959439439235,1.,-0.793516871680993));
#45229=CARTESIAN_POINT('Ctrl Pts',(-3.79711921389897,1.,-0.793235612973273));
#45230=CARTESIAN_POINT('Ctrl Pts',(-3.80459229925637,1.,-0.792882695234778));
#45231=CARTESIAN_POINT('Ctrl Pts',(-3.81202588694756,1.,-0.792462483517634));
#45232=CARTESIAN_POINT('Ctrl Pts',(-3.81944345442249,1.,-0.791981740718635));
#45233=CARTESIAN_POINT('Ctrl Pts',(-3.82687033899792,1.,-0.791447528662369));
#45234=CARTESIAN_POINT('Ctrl Pts',(-3.83432392054786,1.,-0.790865012705301));
#45235=CARTESIAN_POINT('Ctrl Pts',(-3.84180762342454,1.,-0.790236124191242));
#45236=CARTESIAN_POINT('Ctrl Pts',(-3.84931637808894,1.,-0.789560798155582));
#45237=CARTESIAN_POINT('Ctrl Pts',(-3.85683995872529,1.,-0.788837734090672));
#45238=CARTESIAN_POINT('Ctrl Pts',(-3.86436702561345,1.,-0.788065315093777));
#45239=CARTESIAN_POINT('Ctrl Pts',(-3.87188916600912,1.,-0.787242527617999));
#45240=CARTESIAN_POINT('Ctrl Pts',(-3.8794040281819,1.,-0.786369675812608));
#45241=CARTESIAN_POINT('Ctrl Pts',(-3.88691313167398,1.,-0.78544789034073));
#45242=CARTESIAN_POINT('Ctrl Pts',(-3.89442039235103,1.,-0.784478799358336));
#45243=CARTESIAN_POINT('Ctrl Pts',(-3.9019303904397,1.,-0.783464141529081));
#45244=CARTESIAN_POINT('Ctrl Pts',(-3.90944671004542,1.,-0.782405395622764));
#45245=CARTESIAN_POINT('Ctrl Pts',(-3.91697036054676,1.,-0.781303428618366));
#45246=CARTESIAN_POINT('Ctrl Pts',(-3.92450058323823,1.,-0.780158678615542));
#45247=CARTESIAN_POINT('Ctrl Pts',(-3.93203552473174,1.,-0.778971308134821));
#45248=CARTESIAN_POINT('Ctrl Pts',(-3.93957296768103,1.,-0.777741370568558));
#45249=CARTESIAN_POINT('Ctrl Pts',(-3.94711101619447,1.,-0.776468966697921));
#45250=CARTESIAN_POINT('Ctrl Pts',(-3.9546488545231,1.,-0.775154418039351));
#45251=CARTESIAN_POINT('Ctrl Pts',(-3.96218649639807,1.,-0.773798212026565));
#45252=CARTESIAN_POINT('Ctrl Pts',(-3.96972446532772,1.,-0.772400931772136));
#45253=CARTESIAN_POINT('Ctrl Pts',(-3.97726349165488,1.,-0.770963190030471));
#45254=CARTESIAN_POINT('Ctrl Pts',(-3.98480422348451,1.,-0.769485566245544));
#45255=CARTESIAN_POINT('Ctrl Pts',(-3.9923468788101,1.,-0.767968531377915));
#45256=CARTESIAN_POINT('Ctrl Pts',(-3.99989129179622,1.,-0.766412457136064));
#45257=CARTESIAN_POINT('Ctrl Pts',(-4.00743706791509,1.,-0.764817648785197));
#45258=CARTESIAN_POINT('Ctrl Pts',(-4.01498370680496,1.,-0.763184371182935));
#45259=CARTESIAN_POINT('Ctrl Pts',(-4.02253072741268,1.,-0.761512875859804));
#45260=CARTESIAN_POINT('Ctrl Pts',(-4.03007781954412,1.,-0.759803433243752));
#45261=CARTESIAN_POINT('Ctrl Pts',(-4.03762485803119,1.,-0.758056338884944));
#45262=CARTESIAN_POINT('Ctrl Pts',(-4.04517182653997,1.,-0.756271902369581));
#45263=CARTESIAN_POINT('Ctrl Pts',(-4.05271876687915,1.,-0.754450441816078));
#45264=CARTESIAN_POINT('Ctrl Pts',(-4.06026572221515,1.,-0.752592276483072));
#45265=CARTESIAN_POINT('Ctrl Pts',(-4.06781267242378,1.,-0.750697720484036));
#45266=CARTESIAN_POINT('Ctrl Pts',(-4.07535951056152,1.,-0.748767076680557));
#45267=CARTESIAN_POINT('Ctrl Pts',(-4.08290608095642,1.,-0.746800631492315));
#45268=CARTESIAN_POINT('Ctrl Pts',(-4.09045220253573,1.,-0.7447986497065));
#45269=CARTESIAN_POINT('Ctrl Pts',(-4.09799769702611,1.,-0.742761369689841));
#45270=CARTESIAN_POINT('Ctrl Pts',(-4.10554241757547,1.,-0.740688998553377));
#45271=CARTESIAN_POINT('Ctrl Pts',(-4.11308626951927,1.,-0.738581708225844));
#45272=CARTESIAN_POINT('Ctrl Pts',(-4.120629196238,1.,-0.736439634331345));
#45273=CARTESIAN_POINT('Ctrl Pts',(-4.12666277570844,1.,-0.734698226764092));
#45274=CARTESIAN_POINT('Ctrl Pts',(-4.13118752795207,1.,-0.733376589323546));
#45275=CARTESIAN_POINT('Ctrl Pts',(-4.1342038373684,1.,-0.732488575135159));
#45276=CARTESIAN_POINT('Ctrl Pts',(-4.13571194405636,1.,-0.73204283740062));
#45277=CARTESIAN_POINT('Origin',(-4.13571194405636,0.,-0.73204283740062));
#45278=CARTESIAN_POINT('',(-4.15950947128175,1.,-0.581791163835815));
#45279=CARTESIAN_POINT('Origin',(0.,0.,0.));
#45280=CARTESIAN_POINT('',(-3.62400312501245,1.,-0.963899035117248));
#45281=CARTESIAN_POINT('Origin',(0.,1.,0.));
#45282=CARTESIAN_POINT('Ctrl Pts',(-3.62400312501245,1.,-0.963899035117249));
#45283=CARTESIAN_POINT('Ctrl Pts',(-3.62400312501245,0.666666666666667,
-0.963899035117249));
#45284=CARTESIAN_POINT('Ctrl Pts',(-3.62400312501245,0.333333333333333,
-0.963899035117249));
#45285=CARTESIAN_POINT('Ctrl Pts',(-3.62400312501245,-0.333333333333333,
-0.963899035117249));
#45286=CARTESIAN_POINT('Ctrl Pts',(-3.62400312501246,-0.666666666666667,
-0.963899035117249));
#45287=CARTESIAN_POINT('Ctrl Pts',(-3.62400312501246,-1.,-0.963899035117249));
#45288=CARTESIAN_POINT('Ctrl Pts',(-4.01728681790024,-1.,-1.22531898815164));
#45289=CARTESIAN_POINT('Ctrl Pts',(-4.01728681790024,1.,-1.22531898815164));
#45290=CARTESIAN_POINT('Ctrl Pts',(-4.0161454457032,-1.,-1.22423716681447));
#45291=CARTESIAN_POINT('Ctrl Pts',(-4.0161454457032,1.,-1.22423716681447));
#45292=CARTESIAN_POINT('Ctrl Pts',(-4.01386104434674,-1.,-1.22207656456199));
#45293=CARTESIAN_POINT('Ctrl Pts',(-4.01386104434674,1.,-1.22207656456199));
#45294=CARTESIAN_POINT('Ctrl Pts',(-4.01042947142681,-1.,-1.21884478244983));
#45295=CARTESIAN_POINT('Ctrl Pts',(-4.01042947142681,1.,-1.21884478244983));
#45296=CARTESIAN_POINT('Ctrl Pts',(-4.00584409524937,-1.,-1.21455398918813));
#45297=CARTESIAN_POINT('Ctrl Pts',(-4.00584409524937,1.,-1.21455398918813));
#45298=CARTESIAN_POINT('Ctrl Pts',(-4.00009577952534,-1.,-1.20922097030107));
#45299=CARTESIAN_POINT('Ctrl Pts',(-4.00009577952534,1.,-1.20922097030107));
#45300=CARTESIAN_POINT('Ctrl Pts',(-3.99433084800649,-1.,-1.2039185237544));
#45301=CARTESIAN_POINT('Ctrl Pts',(-3.99433084800649,1.,-1.2039185237544));
#45302=CARTESIAN_POINT('Ctrl Pts',(-3.98854928957287,-1.,-1.19864679609596));
#45303=CARTESIAN_POINT('Ctrl Pts',(-3.98854928957287,1.,-1.19864679609596));
#45304=CARTESIAN_POINT('Ctrl Pts',(-3.98275111052015,-1.,-1.19340598349307));
#45305=CARTESIAN_POINT('Ctrl Pts',(-3.98275111052015,1.,-1.19340598349307));
#45306=CARTESIAN_POINT('Ctrl Pts',(-3.97693634766926,-1.,-1.18819633715285));
#45307=CARTESIAN_POINT('Ctrl Pts',(-3.97693634766926,1.,-1.18819633715285));
#45308=CARTESIAN_POINT('Ctrl Pts',(-3.9711050516465,-1.,-1.18301815039596));
#45309=CARTESIAN_POINT('Ctrl Pts',(-3.9711050516465,1.,-1.18301815039596));
#45310=CARTESIAN_POINT('Ctrl Pts',(-3.96525726357682,-1.,-1.17787174135445));
#45311=CARTESIAN_POINT('Ctrl Pts',(-3.96525726357682,1.,-1.17787174135445));
#45312=CARTESIAN_POINT('Ctrl Pts',(-3.95939299213164,-1.,-1.17275743590327));
#45313=CARTESIAN_POINT('Ctrl Pts',(-3.95939299213164,1.,-1.17275743590327));
#45314=CARTESIAN_POINT('Ctrl Pts',(-3.95351219510062,-1.,-1.16767555244495));
#45315=CARTESIAN_POINT('Ctrl Pts',(-3.95351219510062,1.,-1.16767555244495));
#45316=CARTESIAN_POINT('Ctrl Pts',(-3.9476147478092,-1.,-1.16262637999261));
#45317=CARTESIAN_POINT('Ctrl Pts',(-3.9476147478092,1.,-1.16262637999261));
#45318=CARTESIAN_POINT('Ctrl Pts',(-3.94170046685542,-1.,-1.1576101834106));
#45319=CARTESIAN_POINT('Ctrl Pts',(-3.94170046685542,1.,-1.1576101834106));
#45320=CARTESIAN_POINT('Ctrl Pts',(-3.9357691705651,-1.,-1.1526272271639));
#45321=CARTESIAN_POINT('Ctrl Pts',(-3.9357691705651,1.,-1.1526272271639));
#45322=CARTESIAN_POINT('Ctrl Pts',(-3.92982073294334,-1.,-1.14767779451147));
#45323=CARTESIAN_POINT('Ctrl Pts',(-3.92982073294334,1.,-1.14767779451147));
#45324=CARTESIAN_POINT('Ctrl Pts',(-3.92385513133937,-1.,-1.14276220561575));
#45325=CARTESIAN_POINT('Ctrl Pts',(-3.92385513133937,1.,-1.14276220561575));
#45326=CARTESIAN_POINT('Ctrl Pts',(-3.91787251936688,-1.,-1.13788084225511));
#45327=CARTESIAN_POINT('Ctrl Pts',(-3.91787251936688,1.,-1.13788084225511));
#45328=CARTESIAN_POINT('Ctrl Pts',(-3.91187321145495,-1.,-1.13303414693849));
#45329=CARTESIAN_POINT('Ctrl Pts',(-3.91187321145495,1.,-1.13303414693849));
#45330=CARTESIAN_POINT('Ctrl Pts',(-3.90585753318622,-1.,-1.12822258281518));
#45331=CARTESIAN_POINT('Ctrl Pts',(-3.90585753318622,1.,-1.12822258281518));
#45332=CARTESIAN_POINT('Ctrl Pts',(-3.89982569749978,-1.,-1.12344660099029));
#45333=CARTESIAN_POINT('Ctrl Pts',(-3.89982569749978,1.,-1.12344660099029));
#45334=CARTESIAN_POINT('Ctrl Pts',(-3.89377768340362,-1.,-1.11870660794609));
#45335=CARTESIAN_POINT('Ctrl Pts',(-3.89377768340362,1.,-1.11870660794609));
#45336=CARTESIAN_POINT('Ctrl Pts',(-3.88771308285229,-1.,-1.11400292434447));
#45337=CARTESIAN_POINT('Ctrl Pts',(-3.88771308285229,1.,-1.11400292434447));
#45338=CARTESIAN_POINT('Ctrl Pts',(-3.88163105531791,-1.,-1.10933577224029));
#45339=CARTESIAN_POINT('Ctrl Pts',(-3.88163105531791,1.,-1.10933577224029));
#45340=CARTESIAN_POINT('Ctrl Pts',(-3.87553067187566,-1.,-1.10470536603303));
#45341=CARTESIAN_POINT('Ctrl Pts',(-3.87553067187566,1.,-1.10470536603303));
#45342=CARTESIAN_POINT('Ctrl Pts',(-3.86941120134872,-1.,-1.10011198761202));
#45343=CARTESIAN_POINT('Ctrl Pts',(-3.86941120134872,1.,-1.10011198761202));
#45344=CARTESIAN_POINT('Ctrl Pts',(-3.86327241021242,-1.,-1.09555606505012));
#45345=CARTESIAN_POINT('Ctrl Pts',(-3.86327241021242,1.,-1.09555606505012));
#45346=CARTESIAN_POINT('Ctrl Pts',(-3.85711487933911,-1.,-1.09103825516288));
#45347=CARTESIAN_POINT('Ctrl Pts',(-3.85711487933911,1.,-1.09103825516288));
#45348=CARTESIAN_POINT('Ctrl Pts',(-3.8509402522269,-1.,-1.08655950846377));
#45349=CARTESIAN_POINT('Ctrl Pts',(-3.8509402522269,1.,-1.08655950846377));
#45350=CARTESIAN_POINT('Ctrl Pts',(-3.84475048030615,-1.,-1.08212087917986));
#45351=CARTESIAN_POINT('Ctrl Pts',(-3.84475048030615,1.,-1.08212087917986));
#45352=CARTESIAN_POINT('Ctrl Pts',(-3.83854714117486,-1.,-1.07772335353856));
#45353=CARTESIAN_POINT('Ctrl Pts',(-3.83854714117486,1.,-1.07772335353856));
#45354=CARTESIAN_POINT('Ctrl Pts',(-3.83233071195145,-1.,-1.0733676663346));
#45355=CARTESIAN_POINT('Ctrl Pts',(-3.83233071195145,1.,-1.0733676663346));
#45356=CARTESIAN_POINT('Ctrl Pts',(-3.82609989967278,-1.,-1.0690541318036));
#45357=CARTESIAN_POINT('Ctrl Pts',(-3.82609989967278,1.,-1.0690541318036));
#45358=CARTESIAN_POINT('Ctrl Pts',(-3.81985083953012,-1.,-1.06478244038931));
#45359=CARTESIAN_POINT('Ctrl Pts',(-3.81985083953012,1.,-1.06478244038931));
#45360=CARTESIAN_POINT('Ctrl Pts',(-3.81357866117485,-1.,-1.06055206187298));
#45361=CARTESIAN_POINT('Ctrl Pts',(-3.81357866117485,1.,-1.06055206187298));
#45362=CARTESIAN_POINT('Ctrl Pts',(-3.80727913637784,-1.,-1.05636266918643));
#45363=CARTESIAN_POINT('Ctrl Pts',(-3.80727913637784,1.,-1.05636266918643));
#45364=CARTESIAN_POINT('Ctrl Pts',(-3.80095039790678,-1.,-1.05221457990015));
#45365=CARTESIAN_POINT('Ctrl Pts',(-3.80095039790678,1.,-1.05221457990015));
#45366=CARTESIAN_POINT('Ctrl Pts',(-3.79459440308793,-1.,-1.04810913267641));
#45367=CARTESIAN_POINT('Ctrl Pts',(-3.79459440308793,1.,-1.04810913267641));
#45368=CARTESIAN_POINT('Ctrl Pts',(-3.78821910787195,-1.,-1.04404924374426));
#45369=CARTESIAN_POINT('Ctrl Pts',(-3.78821910787195,1.,-1.04404924374426));
#45370=CARTESIAN_POINT('Ctrl Pts',(-3.78183535008192,-1.,-1.04003862055804));
#45371=CARTESIAN_POINT('Ctrl Pts',(-3.78183535008192,1.,-1.04003862055804));
#45372=CARTESIAN_POINT('Ctrl Pts',(-3.77545283140445,-1.,-1.03608074678013));
#45373=CARTESIAN_POINT('Ctrl Pts',(-3.77545283140445,1.,-1.03608074678013));
#45374=CARTESIAN_POINT('Ctrl Pts',(-3.76907609832522,-1.,-1.0321778660492));
#45375=CARTESIAN_POINT('Ctrl Pts',(-3.76907609832522,1.,-1.0321778660492));
#45376=CARTESIAN_POINT('Ctrl Pts',(-3.76270122291232,-1.,-1.02833014458181));
#45377=CARTESIAN_POINT('Ctrl Pts',(-3.76270122291232,1.,-1.02833014458181));
#45378=CARTESIAN_POINT('Ctrl Pts',(-3.75631037456194,-1.,-1.0245342944466));
#45379=CARTESIAN_POINT('Ctrl Pts',(-3.75631037456194,1.,-1.0245342944466));
#45380=CARTESIAN_POINT('Ctrl Pts',(-3.74987777155834,-1.,-1.02078510487428));
#45381=CARTESIAN_POINT('Ctrl Pts',(-3.74987777155834,1.,-1.02078510487428));
#45382=CARTESIAN_POINT('Ctrl Pts',(-3.74337942504959,-1.,-1.01707794311079));
#45383=CARTESIAN_POINT('Ctrl Pts',(-3.74337942504959,1.,-1.01707794311079));
#45384=CARTESIAN_POINT('Ctrl Pts',(-3.73680245055734,-1.,-1.01341114319903));
#45385=CARTESIAN_POINT('Ctrl Pts',(-3.73680245055734,1.,-1.01341114319903));
#45386=CARTESIAN_POINT('Ctrl Pts',(-3.73015276704426,-1.,-1.00978798539496));
#45387=CARTESIAN_POINT('Ctrl Pts',(-3.73015276704426,1.,-1.00978798539496));
#45388=CARTESIAN_POINT('Ctrl Pts',(-3.72346803750595,-1.,-1.0062200073571));
#45389=CARTESIAN_POINT('Ctrl Pts',(-3.72346803750595,1.,-1.0062200073571));
#45390=CARTESIAN_POINT('Ctrl Pts',(-3.71680667125118,-1.,-1.00272423396822));
#45391=CARTESIAN_POINT('Ctrl Pts',(-3.71680667125118,1.,-1.00272423396822));
#45392=CARTESIAN_POINT('Ctrl Pts',(-3.71022439713938,-1.,-0.99931726075653));
#45393=CARTESIAN_POINT('Ctrl Pts',(-3.71022439713938,1.,-0.99931726075653));
#45394=CARTESIAN_POINT('Ctrl Pts',(-3.70375282282138,-1.,-0.996009819772518));
#45395=CARTESIAN_POINT('Ctrl Pts',(-3.70375282282138,1.,-0.996009819772518));
#45396=CARTESIAN_POINT('Ctrl Pts',(-3.69738123415662,-1.,-0.99280221833201));
#45397=CARTESIAN_POINT('Ctrl Pts',(-3.69738123415662,1.,-0.99280221833201));
#45398=CARTESIAN_POINT('Ctrl Pts',(-3.69102682138846,-1.,-0.989676715398558));
#45399=CARTESIAN_POINT('Ctrl Pts',(-3.69102682138846,1.,-0.989676715398558));
#45400=CARTESIAN_POINT('Ctrl Pts',(-3.68455317926068,-1.,-0.986602639863837));
#45401=CARTESIAN_POINT('Ctrl Pts',(-3.68455317926068,1.,-0.986602639863837));
#45402=CARTESIAN_POINT('Ctrl Pts',(-3.67782408841715,-1.,-0.983550791470419));
#45403=CARTESIAN_POINT('Ctrl Pts',(-3.67782408841715,1.,-0.983550791470419));
#45404=CARTESIAN_POINT('Ctrl Pts',(-3.67074983340361,-1.,-0.980505922458267));
#45405=CARTESIAN_POINT('Ctrl Pts',(-3.67074983340361,1.,-0.980505922458267));
#45406=CARTESIAN_POINT('Ctrl Pts',(-3.66333049637475,-1.,-0.977478312751618));
#45407=CARTESIAN_POINT('Ctrl Pts',(-3.66333049637475,1.,-0.977478312751618));
#45408=CARTESIAN_POINT('Ctrl Pts',(-3.65571576735126,-1.,-0.974519971354848));
#45409=CARTESIAN_POINT('Ctrl Pts',(-3.65571576735126,1.,-0.974519971354848));
#45410=CARTESIAN_POINT('Ctrl Pts',(-3.64819756447455,-1.,-0.971722122061341));
#45411=CARTESIAN_POINT('Ctrl Pts',(-3.64819756447455,1.,-0.971722122061341));
#45412=CARTESIAN_POINT('Ctrl Pts',(-3.64113946505766,-1.,-0.969195124675865));
#45413=CARTESIAN_POINT('Ctrl Pts',(-3.64113946505766,1.,-0.969195124675865));
#45414=CARTESIAN_POINT('Ctrl Pts',(-3.63492122081143,-1.,-0.967052554541385));
#45415=CARTESIAN_POINT('Ctrl Pts',(-3.63492122081143,1.,-0.967052554541385));
#45416=CARTESIAN_POINT('Ctrl Pts',(-3.62988252139846,-1.,-0.965395153165293));
#45417=CARTESIAN_POINT('Ctrl Pts',(-3.62988252139846,1.,-0.965395153165293));
#45418=CARTESIAN_POINT('Ctrl Pts',(-3.62625391254797,-1.,-0.964291001273287));
#45419=CARTESIAN_POINT('Ctrl Pts',(-3.62625391254797,1.,-0.964291001273287));
#45420=CARTESIAN_POINT('Ctrl Pts',(-3.6245656860652,-1.,-0.963875774530619));
#45421=CARTESIAN_POINT('Ctrl Pts',(-3.6245656860652,1.,-0.963875774530619));
#45422=CARTESIAN_POINT('Ctrl Pts',(-3.62399933639914,-1.,-0.963832486395051));
#45423=CARTESIAN_POINT('Ctrl Pts',(-3.62399933639914,1.,-0.963832486395051));
#45424=CARTESIAN_POINT('Ctrl Pts',(-3.62393257642052,-1.,-0.963922720982193));
#45425=CARTESIAN_POINT('Ctrl Pts',(-3.62393257642052,1.,-0.963922720982193));
#45426=CARTESIAN_POINT('Ctrl Pts',(-3.62397690409552,-1.,-0.963997613369571));
#45427=CARTESIAN_POINT('Ctrl Pts',(-3.62397690409552,1.,-0.963997613369571));
#45428=CARTESIAN_POINT('',(-4.01728681790024,1.,-1.22531898815164));
#45429=CARTESIAN_POINT('Ctrl Pts',(-4.01728681790024,1.,-1.22531898815164));
#45430=CARTESIAN_POINT('Ctrl Pts',(-4.0161454457032,1.,-1.22423716681447));
#45431=CARTESIAN_POINT('Ctrl Pts',(-4.01386104434674,1.,-1.22207656456199));
#45432=CARTESIAN_POINT('Ctrl Pts',(-4.01042947142681,1.,-1.21884478244983));
#45433=CARTESIAN_POINT('Ctrl Pts',(-4.00584409524937,1.,-1.21455398918813));
#45434=CARTESIAN_POINT('Ctrl Pts',(-4.00009577952534,1.,-1.20922097030107));
#45435=CARTESIAN_POINT('Ctrl Pts',(-3.99433084800649,1.,-1.2039185237544));
#45436=CARTESIAN_POINT('Ctrl Pts',(-3.98854928957287,1.,-1.19864679609596));
#45437=CARTESIAN_POINT('Ctrl Pts',(-3.98275111052015,1.,-1.19340598349307));
#45438=CARTESIAN_POINT('Ctrl Pts',(-3.97693634766926,1.,-1.18819633715285));
#45439=CARTESIAN_POINT('Ctrl Pts',(-3.9711050516465,1.,-1.18301815039596));
#45440=CARTESIAN_POINT('Ctrl Pts',(-3.96525726357682,1.,-1.17787174135445));
#45441=CARTESIAN_POINT('Ctrl Pts',(-3.95939299213164,1.,-1.17275743590327));
#45442=CARTESIAN_POINT('Ctrl Pts',(-3.95351219510062,1.,-1.16767555244495));
#45443=CARTESIAN_POINT('Ctrl Pts',(-3.9476147478092,1.,-1.16262637999261));
#45444=CARTESIAN_POINT('Ctrl Pts',(-3.94170046685542,1.,-1.1576101834106));
#45445=CARTESIAN_POINT('Ctrl Pts',(-3.9357691705651,1.,-1.1526272271639));
#45446=CARTESIAN_POINT('Ctrl Pts',(-3.92982073294334,1.,-1.14767779451147));
#45447=CARTESIAN_POINT('Ctrl Pts',(-3.92385513133937,1.,-1.14276220561575));
#45448=CARTESIAN_POINT('Ctrl Pts',(-3.91787251936688,1.,-1.13788084225511));
#45449=CARTESIAN_POINT('Ctrl Pts',(-3.91187321145495,1.,-1.13303414693849));
#45450=CARTESIAN_POINT('Ctrl Pts',(-3.90585753318622,1.,-1.12822258281518));
#45451=CARTESIAN_POINT('Ctrl Pts',(-3.89982569749978,1.,-1.12344660099029));
#45452=CARTESIAN_POINT('Ctrl Pts',(-3.89377768340362,1.,-1.11870660794609));
#45453=CARTESIAN_POINT('Ctrl Pts',(-3.88771308285229,1.,-1.11400292434447));
#45454=CARTESIAN_POINT('Ctrl Pts',(-3.88163105531791,1.,-1.10933577224029));
#45455=CARTESIAN_POINT('Ctrl Pts',(-3.87553067187566,1.,-1.10470536603303));
#45456=CARTESIAN_POINT('Ctrl Pts',(-3.86941120134872,1.,-1.10011198761202));
#45457=CARTESIAN_POINT('Ctrl Pts',(-3.86327241021242,1.,-1.09555606505012));
#45458=CARTESIAN_POINT('Ctrl Pts',(-3.85711487933911,1.,-1.09103825516288));
#45459=CARTESIAN_POINT('Ctrl Pts',(-3.8509402522269,1.,-1.08655950846377));
#45460=CARTESIAN_POINT('Ctrl Pts',(-3.84475048030615,1.,-1.08212087917986));
#45461=CARTESIAN_POINT('Ctrl Pts',(-3.83854714117486,1.,-1.07772335353856));
#45462=CARTESIAN_POINT('Ctrl Pts',(-3.83233071195145,1.,-1.0733676663346));
#45463=CARTESIAN_POINT('Ctrl Pts',(-3.82609989967278,1.,-1.0690541318036));
#45464=CARTESIAN_POINT('Ctrl Pts',(-3.81985083953012,1.,-1.06478244038931));
#45465=CARTESIAN_POINT('Ctrl Pts',(-3.81357866117485,1.,-1.06055206187298));
#45466=CARTESIAN_POINT('Ctrl Pts',(-3.80727913637784,1.,-1.05636266918643));
#45467=CARTESIAN_POINT('Ctrl Pts',(-3.80095039790678,1.,-1.05221457990015));
#45468=CARTESIAN_POINT('Ctrl Pts',(-3.79459440308793,1.,-1.04810913267641));
#45469=CARTESIAN_POINT('Ctrl Pts',(-3.78821910787195,1.,-1.04404924374426));
#45470=CARTESIAN_POINT('Ctrl Pts',(-3.78183535008192,1.,-1.04003862055804));
#45471=CARTESIAN_POINT('Ctrl Pts',(-3.77545283140445,1.,-1.03608074678013));
#45472=CARTESIAN_POINT('Ctrl Pts',(-3.76907609832522,1.,-1.0321778660492));
#45473=CARTESIAN_POINT('Ctrl Pts',(-3.76270122291232,1.,-1.02833014458181));
#45474=CARTESIAN_POINT('Ctrl Pts',(-3.75631037456194,1.,-1.0245342944466));
#45475=CARTESIAN_POINT('Ctrl Pts',(-3.74987777155834,1.,-1.02078510487428));
#45476=CARTESIAN_POINT('Ctrl Pts',(-3.74337942504959,1.,-1.01707794311079));
#45477=CARTESIAN_POINT('Ctrl Pts',(-3.73680245055734,1.,-1.01341114319903));
#45478=CARTESIAN_POINT('Ctrl Pts',(-3.73015276704426,1.,-1.00978798539496));
#45479=CARTESIAN_POINT('Ctrl Pts',(-3.72346803750595,1.,-1.0062200073571));
#45480=CARTESIAN_POINT('Ctrl Pts',(-3.71680667125118,1.,-1.00272423396822));
#45481=CARTESIAN_POINT('Ctrl Pts',(-3.71022439713938,1.,-0.99931726075653));
#45482=CARTESIAN_POINT('Ctrl Pts',(-3.70375282282138,1.,-0.996009819772518));
#45483=CARTESIAN_POINT('Ctrl Pts',(-3.69738123415662,1.,-0.99280221833201));
#45484=CARTESIAN_POINT('Ctrl Pts',(-3.69102682138846,1.,-0.989676715398558));
#45485=CARTESIAN_POINT('Ctrl Pts',(-3.68455317926068,1.,-0.986602639863837));
#45486=CARTESIAN_POINT('Ctrl Pts',(-3.67782408841715,1.,-0.983550791470419));
#45487=CARTESIAN_POINT('Ctrl Pts',(-3.67074983340361,1.,-0.980505922458267));
#45488=CARTESIAN_POINT('Ctrl Pts',(-3.66333049637475,1.,-0.977478312751618));
#45489=CARTESIAN_POINT('Ctrl Pts',(-3.65571576735126,1.,-0.974519971354848));
#45490=CARTESIAN_POINT('Ctrl Pts',(-3.64819756447455,1.,-0.971722122061341));
#45491=CARTESIAN_POINT('Ctrl Pts',(-3.64113946505766,1.,-0.969195124675865));
#45492=CARTESIAN_POINT('Ctrl Pts',(-3.63492122081143,1.,-0.967052554541385));
#45493=CARTESIAN_POINT('Ctrl Pts',(-3.62988252139846,1.,-0.965395153165293));
#45494=CARTESIAN_POINT('Ctrl Pts',(-3.62652618145335,1.,-0.964373850166458));
#45495=CARTESIAN_POINT('Ctrl Pts',(-3.62489305727662,1.,-0.963957782642843));
#45496=CARTESIAN_POINT('Ctrl Pts',(-3.62424461507588,1.,-0.963861297423241));
#45497=CARTESIAN_POINT('Ctrl Pts',(-3.6240482887845,1.,-0.963880158555582));
#45498=CARTESIAN_POINT('Ctrl Pts',(-3.62400312501245,1.,-0.963899035117249));
#45499=CARTESIAN_POINT('',(-4.01728681790024,0.,-1.22531898815164));
#45500=CARTESIAN_POINT('Ctrl Pts',(-3.49848248301936,-1.,-1.35022972712301));
#45501=CARTESIAN_POINT('Ctrl Pts',(-3.49848248301936,1.,-1.35022972712301));
#45502=CARTESIAN_POINT('Ctrl Pts',(-3.4984026005375,-1.,-1.35026426118402));
#45503=CARTESIAN_POINT('Ctrl Pts',(-3.4984026005375,1.,-1.35026426118402));
#45504=CARTESIAN_POINT('Ctrl Pts',(-3.49840357193736,-1.,-1.35037650303019));
#45505=CARTESIAN_POINT('Ctrl Pts',(-3.49840357193736,1.,-1.35037650303019));
#45506=CARTESIAN_POINT('Ctrl Pts',(-3.49888720257132,-1.,-1.35067437417483));
#45507=CARTESIAN_POINT('Ctrl Pts',(-3.49888720257132,1.,-1.35067437417483));
#45508=CARTESIAN_POINT('Ctrl Pts',(-3.5004970706414,-1.,-1.3513307633124));
#45509=CARTESIAN_POINT('Ctrl Pts',(-3.5004970706414,1.,-1.3513307633124));
#45510=CARTESIAN_POINT('Ctrl Pts',(-3.50408168106261,-1.,-1.35257032843486));
#45511=CARTESIAN_POINT('Ctrl Pts',(-3.50408168106261,1.,-1.35257032843486));
#45512=CARTESIAN_POINT('Ctrl Pts',(-3.50913227059999,-1.,-1.35419113575956));
#45513=CARTESIAN_POINT('Ctrl Pts',(-3.50913227059999,1.,-1.35419113575956));
#45514=CARTESIAN_POINT('Ctrl Pts',(-3.51542230699556,-1.,-1.35611275237152));
#45515=CARTESIAN_POINT('Ctrl Pts',(-3.51542230699556,1.,-1.35611275237152));
#45516=CARTESIAN_POINT('Ctrl Pts',(-3.52261776116748,-1.,-1.35821701528836));
#45517=CARTESIAN_POINT('Ctrl Pts',(-3.52261776116748,1.,-1.35821701528836));
#45518=CARTESIAN_POINT('Ctrl Pts',(-3.530344649616,-1.,-1.36037259643734));
#45519=CARTESIAN_POINT('Ctrl Pts',(-3.530344649616,1.,-1.36037259643734));
#45520=CARTESIAN_POINT('Ctrl Pts',(-3.53824396424961,-1.,-1.36245507339307));
#45521=CARTESIAN_POINT('Ctrl Pts',(-3.53824396424961,1.,-1.36245507339307));
#45522=CARTESIAN_POINT('Ctrl Pts',(-3.54602591832973,-1.,-1.36436666257597));
#45523=CARTESIAN_POINT('Ctrl Pts',(-3.54602591832973,1.,-1.36436666257597));
#45524=CARTESIAN_POINT('Ctrl Pts',(-3.55353883995949,-1.,-1.3660614545677));
#45525=CARTESIAN_POINT('Ctrl Pts',(-3.55353883995949,1.,-1.3660614545677));
#45526=CARTESIAN_POINT('Ctrl Pts',(-3.56077662028649,-1.,-1.36754771771233));
#45527=CARTESIAN_POINT('Ctrl Pts',(-3.56077662028649,1.,-1.36754771771233));
#45528=CARTESIAN_POINT('Ctrl Pts',(-3.5678208030466,-1.,-1.36886584973389));
#45529=CARTESIAN_POINT('Ctrl Pts',(-3.5678208030466,1.,-1.36886584973389));
#45530=CARTESIAN_POINT('Ctrl Pts',(-3.57479875549486,-1.,-1.37007229485659));
#45531=CARTESIAN_POINT('Ctrl Pts',(-3.57479875549486,1.,-1.37007229485659));
#45532=CARTESIAN_POINT('Ctrl Pts',(-3.58183885982715,-1.,-1.37122241663062));
#45533=CARTESIAN_POINT('Ctrl Pts',(-3.58183885982715,1.,-1.37122241663062));
#45534=CARTESIAN_POINT('Ctrl Pts',(-3.58901853846365,-1.,-1.37235053660976));
#45535=CARTESIAN_POINT('Ctrl Pts',(-3.58901853846365,1.,-1.37235053660976));
#45536=CARTESIAN_POINT('Ctrl Pts',(-3.59634627869048,-1.,-1.37346320103157));
#45537=CARTESIAN_POINT('Ctrl Pts',(-3.59634627869048,1.,-1.37346320103157));
#45538=CARTESIAN_POINT('Ctrl Pts',(-3.60379020123988,-1.,-1.37455051379623));
#45539=CARTESIAN_POINT('Ctrl Pts',(-3.60379020123988,1.,-1.37455051379623));
#45540=CARTESIAN_POINT('Ctrl Pts',(-3.61129546591064,-1.,-1.37559314436634));
#45541=CARTESIAN_POINT('Ctrl Pts',(-3.61129546591064,1.,-1.37559314436634));
#45542=CARTESIAN_POINT('Ctrl Pts',(-3.6188048116042,-1.,-1.37657053403107));
#45543=CARTESIAN_POINT('Ctrl Pts',(-3.6188048116042,1.,-1.37657053403107));
#45544=CARTESIAN_POINT('Ctrl Pts',(-3.62628098665145,-1.,-1.37746987919881));
#45545=CARTESIAN_POINT('Ctrl Pts',(-3.62628098665145,1.,-1.37746987919881));
#45546=CARTESIAN_POINT('Ctrl Pts',(-3.63371727442486,-1.,-1.37829035457339));
#45547=CARTESIAN_POINT('Ctrl Pts',(-3.63371727442486,1.,-1.37829035457339));
#45548=CARTESIAN_POINT('Ctrl Pts',(-3.64112507791141,-1.,-1.37903818567359));
#45549=CARTESIAN_POINT('Ctrl Pts',(-3.64112507791141,1.,-1.37903818567359));
#45550=CARTESIAN_POINT('Ctrl Pts',(-3.64852652756456,-1.,-1.37972372481603));
#45551=CARTESIAN_POINT('Ctrl Pts',(-3.64852652756456,1.,-1.37972372481603));
#45552=CARTESIAN_POINT('Ctrl Pts',(-3.6559455440439,-1.,-1.38035791051212));
#45553=CARTESIAN_POINT('Ctrl Pts',(-3.6559455440439,1.,-1.38035791051212));
#45554=CARTESIAN_POINT('Ctrl Pts',(-3.66339848520857,-1.,-1.38094856333552));
#45555=CARTESIAN_POINT('Ctrl Pts',(-3.66339848520857,1.,-1.38094856333552));
#45556=CARTESIAN_POINT('Ctrl Pts',(-3.67088843112262,-1.,-1.38149812653868));
#45557=CARTESIAN_POINT('Ctrl Pts',(-3.67088843112262,1.,-1.38149812653868));
#45558=CARTESIAN_POINT('Ctrl Pts',(-3.67841038482414,-1.,-1.3820057429062));
#45559=CARTESIAN_POINT('Ctrl Pts',(-3.67841038482414,1.,-1.3820057429062));
#45560=CARTESIAN_POINT('Ctrl Pts',(-3.68595444983837,-1.,-1.38246852827182));
#45561=CARTESIAN_POINT('Ctrl Pts',(-3.68595444983837,1.,-1.38246852827182));
#45562=CARTESIAN_POINT('Ctrl Pts',(-3.69350967899526,-1.,-1.3828831117165));
#45563=CARTESIAN_POINT('Ctrl Pts',(-3.69350967899526,1.,-1.3828831117165));
#45564=CARTESIAN_POINT('Ctrl Pts',(-3.701067921679,-1.,-1.38324717612865));
#45565=CARTESIAN_POINT('Ctrl Pts',(-3.701067921679,1.,-1.38324717612865));
#45566=CARTESIAN_POINT('Ctrl Pts',(-3.70862680753347,-1.,-1.38356065402124));
#45567=CARTESIAN_POINT('Ctrl Pts',(-3.70862680753347,1.,-1.38356065402124));
#45568=CARTESIAN_POINT('Ctrl Pts',(-3.7161876605181,-1.,-1.38382489984586));
#45569=CARTESIAN_POINT('Ctrl Pts',(-3.7161876605181,1.,-1.38382489984586));
#45570=CARTESIAN_POINT('Ctrl Pts',(-3.72375409358803,-1.,-1.3840421342895));
#45571=CARTESIAN_POINT('Ctrl Pts',(-3.72375409358803,1.,-1.3840421342895));
#45572=CARTESIAN_POINT('Ctrl Pts',(-3.73133035859282,-1.,-1.38421479111531));
#45573=CARTESIAN_POINT('Ctrl Pts',(-3.73133035859282,1.,-1.38421479111531));
#45574=CARTESIAN_POINT('Ctrl Pts',(-3.73891976418104,-1.,-1.38434489156458));
#45575=CARTESIAN_POINT('Ctrl Pts',(-3.73891976418104,1.,-1.38434489156458));
#45576=CARTESIAN_POINT('Ctrl Pts',(-3.74652317167876,-1.,-1.38443344984394));
#45577=CARTESIAN_POINT('Ctrl Pts',(-3.74652317167876,1.,-1.38443344984394));
#45578=CARTESIAN_POINT('Ctrl Pts',(-3.7541397631875,-1.,-1.38448077997163));
#45579=CARTESIAN_POINT('Ctrl Pts',(-3.7541397631875,1.,-1.38448077997163));
#45580=CARTESIAN_POINT('Ctrl Pts',(-3.76176768271367,-1.,-1.3844867525335));
#45581=CARTESIAN_POINT('Ctrl Pts',(-3.76176768271367,1.,-1.3844867525335));
#45582=CARTESIAN_POINT('Ctrl Pts',(-3.76940473185779,-1.,-1.38445107339518));
#45583=CARTESIAN_POINT('Ctrl Pts',(-3.76940473185779,1.,-1.38445107339518));
#45584=CARTESIAN_POINT('Ctrl Pts',(-3.77704902230418,-1.,-1.38437354551428));
#45585=CARTESIAN_POINT('Ctrl Pts',(-3.77704902230418,1.,-1.38437354551428));
#45586=CARTESIAN_POINT('Ctrl Pts',(-3.78469969805082,-1.,-1.38425435883756));
#45587=CARTESIAN_POINT('Ctrl Pts',(-3.78469969805082,1.,-1.38425435883756));
#45588=CARTESIAN_POINT('Ctrl Pts',(-3.79235669640841,-1.,-1.38409399694566));
#45589=CARTESIAN_POINT('Ctrl Pts',(-3.79235669640841,1.,-1.38409399694566));
#45590=CARTESIAN_POINT('Ctrl Pts',(-3.80002044322111,-1.,-1.38389311766682));
#45591=CARTESIAN_POINT('Ctrl Pts',(-3.80002044322111,1.,-1.38389311766682));
#45592=CARTESIAN_POINT('Ctrl Pts',(-3.80769156398411,-1.,-1.3836524404622));
#45593=CARTESIAN_POINT('Ctrl Pts',(-3.80769156398411,1.,-1.3836524404622));
#45594=CARTESIAN_POINT('Ctrl Pts',(-3.81537060817811,-1.,-1.38337263902782));
#45595=CARTESIAN_POINT('Ctrl Pts',(-3.81537060817811,1.,-1.38337263902782));
#45596=CARTESIAN_POINT('Ctrl Pts',(-3.82305771743829,-1.,-1.38305421262763));
#45597=CARTESIAN_POINT('Ctrl Pts',(-3.82305771743829,1.,-1.38305421262763));
#45598=CARTESIAN_POINT('Ctrl Pts',(-3.8307526698229,-1.,-1.38269750245138));
#45599=CARTESIAN_POINT('Ctrl Pts',(-3.8307526698229,1.,-1.38269750245138));
#45600=CARTESIAN_POINT('Ctrl Pts',(-3.83845502790746,-1.,-1.38230274828821));
#45601=CARTESIAN_POINT('Ctrl Pts',(-3.83845502790746,1.,-1.38230274828821));
#45602=CARTESIAN_POINT('Ctrl Pts',(-3.84616425605764,-1.,-1.38187013346109));
#45603=CARTESIAN_POINT('Ctrl Pts',(-3.84616425605764,1.,-1.38187013346109));
#45604=CARTESIAN_POINT('Ctrl Pts',(-3.85387983979481,-1.,-1.38139983115049));
#45605=CARTESIAN_POINT('Ctrl Pts',(-3.85387983979481,1.,-1.38139983115049));
#45606=CARTESIAN_POINT('Ctrl Pts',(-3.86160143043959,-1.,-1.38089205992989));
#45607=CARTESIAN_POINT('Ctrl Pts',(-3.86160143043959,1.,-1.38089205992989));
#45608=CARTESIAN_POINT('Ctrl Pts',(-3.86932885813068,-1.,-1.38034709213014));
#45609=CARTESIAN_POINT('Ctrl Pts',(-3.86932885813068,1.,-1.38034709213014));
#45610=CARTESIAN_POINT('Ctrl Pts',(-3.87706205830532,-1.,-1.37976523097073));
#45611=CARTESIAN_POINT('Ctrl Pts',(-3.87706205830532,1.,-1.37976523097073));
#45612=CARTESIAN_POINT('Ctrl Pts',(-3.88480102249277,-1.,-1.37914679719383));
#45613=CARTESIAN_POINT('Ctrl Pts',(-3.88480102249277,1.,-1.37914679719383));
#45614=CARTESIAN_POINT('Ctrl Pts',(-3.89254574338496,-1.,-1.3784921128802));
#45615=CARTESIAN_POINT('Ctrl Pts',(-3.89254574338496,1.,-1.3784921128802));
#45616=CARTESIAN_POINT('Ctrl Pts',(-3.90029615196727,-1.,-1.37780148512792));
#45617=CARTESIAN_POINT('Ctrl Pts',(-3.90029615196727,1.,-1.37780148512792));
#45618=CARTESIAN_POINT('Ctrl Pts',(-3.90805209523486,-1.,-1.3770751963402));
#45619=CARTESIAN_POINT('Ctrl Pts',(-3.90805209523486,1.,-1.3770751963402));
#45620=CARTESIAN_POINT('Ctrl Pts',(-3.91581337462644,-1.,-1.37631350505797));
#45621=CARTESIAN_POINT('Ctrl Pts',(-3.91581337462644,1.,-1.37631350505797));
#45622=CARTESIAN_POINT('Ctrl Pts',(-3.92357976987672,-1.,-1.37551664448242));
#45623=CARTESIAN_POINT('Ctrl Pts',(-3.92357976987672,1.,-1.37551664448242));
#45624=CARTESIAN_POINT('Ctrl Pts',(-3.93135106761844,-1.,-1.37468482215751));
#45625=CARTESIAN_POINT('Ctrl Pts',(-3.93135106761844,1.,-1.37468482215751));
#45626=CARTESIAN_POINT('Ctrl Pts',(-3.93912709040818,-1.,-1.37381821967165));
#45627=CARTESIAN_POINT('Ctrl Pts',(-3.93912709040818,1.,-1.37381821967165));
#45628=CARTESIAN_POINT('Ctrl Pts',(-3.94690771785133,-1.,-1.37291699202807));
#45629=CARTESIAN_POINT('Ctrl Pts',(-3.94690771785133,1.,-1.37291699202807));
#45630=CARTESIAN_POINT('Ctrl Pts',(-3.95469287280914,-1.,-1.37198126432386));
#45631=CARTESIAN_POINT('Ctrl Pts',(-3.95469287280914,1.,-1.37198126432386));
#45632=CARTESIAN_POINT('Ctrl Pts',(-3.96092458506535,-1.,-1.3712051561502));
#45633=CARTESIAN_POINT('Ctrl Pts',(-3.96092458506535,1.,-1.3712051561502));
#45634=CARTESIAN_POINT('Ctrl Pts',(-3.96560037974645,-1.,-1.37060761745635));
#45635=CARTESIAN_POINT('Ctrl Pts',(-3.96560037974645,1.,-1.37060761745635));
#45636=CARTESIAN_POINT('Ctrl Pts',(-3.9687184694131,-1.,-1.37020239094614));
#45637=CARTESIAN_POINT('Ctrl Pts',(-3.9687184694131,1.,-1.37020239094614));
#45638=CARTESIAN_POINT('Ctrl Pts',(-3.97027773754922,-1.,-1.36999806084572));
#45639=CARTESIAN_POINT('Ctrl Pts',(-3.97027773754922,1.,-1.36999806084572));
#45640=CARTESIAN_POINT('',(-3.4984457533445,1.,-1.35032489087101));
#45641=CARTESIAN_POINT('Ctrl Pts',(-3.4984457533445,-1.,-1.35032489087101));
#45642=CARTESIAN_POINT('Ctrl Pts',(-3.4984457533445,-0.666666666666667,
-1.35032489087101));
#45643=CARTESIAN_POINT('Ctrl Pts',(-3.4984457533445,-0.333333333333333,
-1.35032489087101));
#45644=CARTESIAN_POINT('Ctrl Pts',(-3.4984457533445,0.333333333333333,-1.35032489087101));
#45645=CARTESIAN_POINT('Ctrl Pts',(-3.4984457533445,0.666666666666667,-1.35032489087101));
#45646=CARTESIAN_POINT('Ctrl Pts',(-3.4984457533445,1.,-1.35032489087101));
#45647=CARTESIAN_POINT('',(-3.97027773754922,1.,-1.36999806084572));
#45648=CARTESIAN_POINT('',(-3.97027773754922,0.,-1.36999806084572));
#45649=CARTESIAN_POINT('Ctrl Pts',(-3.4984457533445,1.,-1.35032489087101));
#45650=CARTESIAN_POINT('Ctrl Pts',(-3.49847119623846,1.,-1.35036670892966));
#45651=CARTESIAN_POINT('Ctrl Pts',(-3.49861894124827,1.,-1.35049736560527));
#45652=CARTESIAN_POINT('Ctrl Pts',(-3.49920025459723,1.,-1.35080045218587));
#45653=CARTESIAN_POINT('Ctrl Pts',(-3.5007660381649,1.,-1.35142377279517));
#45654=CARTESIAN_POINT('Ctrl Pts',(-3.50408168106261,1.,-1.35257032843486));
#45655=CARTESIAN_POINT('Ctrl Pts',(-3.50913227059999,1.,-1.35419113575956));
#45656=CARTESIAN_POINT('Ctrl Pts',(-3.51542230699556,1.,-1.35611275237152));
#45657=CARTESIAN_POINT('Ctrl Pts',(-3.52261776116748,1.,-1.35821701528836));
#45658=CARTESIAN_POINT('Ctrl Pts',(-3.530344649616,1.,-1.36037259643734));
#45659=CARTESIAN_POINT('Ctrl Pts',(-3.53824396424961,1.,-1.36245507339307));
#45660=CARTESIAN_POINT('Ctrl Pts',(-3.54602591832973,1.,-1.36436666257597));
#45661=CARTESIAN_POINT('Ctrl Pts',(-3.55353883995949,1.,-1.3660614545677));
#45662=CARTESIAN_POINT('Ctrl Pts',(-3.56077662028649,1.,-1.36754771771233));
#45663=CARTESIAN_POINT('Ctrl Pts',(-3.5678208030466,1.,-1.36886584973389));
#45664=CARTESIAN_POINT('Ctrl Pts',(-3.57479875549486,1.,-1.37007229485659));
#45665=CARTESIAN_POINT('Ctrl Pts',(-3.58183885982715,1.,-1.37122241663062));
#45666=CARTESIAN_POINT('Ctrl Pts',(-3.58901853846365,1.,-1.37235053660976));
#45667=CARTESIAN_POINT('Ctrl Pts',(-3.59634627869048,1.,-1.37346320103157));
#45668=CARTESIAN_POINT('Ctrl Pts',(-3.60379020123988,1.,-1.37455051379623));
#45669=CARTESIAN_POINT('Ctrl Pts',(-3.61129546591064,1.,-1.37559314436634));
#45670=CARTESIAN_POINT('Ctrl Pts',(-3.6188048116042,1.,-1.37657053403107));
#45671=CARTESIAN_POINT('Ctrl Pts',(-3.62628098665145,1.,-1.37746987919881));
#45672=CARTESIAN_POINT('Ctrl Pts',(-3.63371727442486,1.,-1.37829035457339));
#45673=CARTESIAN_POINT('Ctrl Pts',(-3.64112507791141,1.,-1.37903818567359));
#45674=CARTESIAN_POINT('Ctrl Pts',(-3.64852652756456,1.,-1.37972372481603));
#45675=CARTESIAN_POINT('Ctrl Pts',(-3.6559455440439,1.,-1.38035791051212));
#45676=CARTESIAN_POINT('Ctrl Pts',(-3.66339848520857,1.,-1.38094856333552));
#45677=CARTESIAN_POINT('Ctrl Pts',(-3.67088843112262,1.,-1.38149812653868));
#45678=CARTESIAN_POINT('Ctrl Pts',(-3.67841038482414,1.,-1.3820057429062));
#45679=CARTESIAN_POINT('Ctrl Pts',(-3.68595444983837,1.,-1.38246852827182));
#45680=CARTESIAN_POINT('Ctrl Pts',(-3.69350967899526,1.,-1.3828831117165));
#45681=CARTESIAN_POINT('Ctrl Pts',(-3.701067921679,1.,-1.38324717612865));
#45682=CARTESIAN_POINT('Ctrl Pts',(-3.70862680753347,1.,-1.38356065402124));
#45683=CARTESIAN_POINT('Ctrl Pts',(-3.7161876605181,1.,-1.38382489984586));
#45684=CARTESIAN_POINT('Ctrl Pts',(-3.72375409358803,1.,-1.3840421342895));
#45685=CARTESIAN_POINT('Ctrl Pts',(-3.73133035859282,1.,-1.38421479111531));
#45686=CARTESIAN_POINT('Ctrl Pts',(-3.73891976418104,1.,-1.38434489156458));
#45687=CARTESIAN_POINT('Ctrl Pts',(-3.74652317167876,1.,-1.38443344984394));
#45688=CARTESIAN_POINT('Ctrl Pts',(-3.7541397631875,1.,-1.38448077997163));
#45689=CARTESIAN_POINT('Ctrl Pts',(-3.76176768271367,1.,-1.3844867525335));
#45690=CARTESIAN_POINT('Ctrl Pts',(-3.76940473185779,1.,-1.38445107339518));
#45691=CARTESIAN_POINT('Ctrl Pts',(-3.77704902230418,1.,-1.38437354551428));
#45692=CARTESIAN_POINT('Ctrl Pts',(-3.78469969805082,1.,-1.38425435883756));
#45693=CARTESIAN_POINT('Ctrl Pts',(-3.79235669640841,1.,-1.38409399694566));
#45694=CARTESIAN_POINT('Ctrl Pts',(-3.80002044322111,1.,-1.38389311766682));
#45695=CARTESIAN_POINT('Ctrl Pts',(-3.80769156398411,1.,-1.3836524404622));
#45696=CARTESIAN_POINT('Ctrl Pts',(-3.81537060817811,1.,-1.38337263902782));
#45697=CARTESIAN_POINT('Ctrl Pts',(-3.82305771743829,1.,-1.38305421262763));
#45698=CARTESIAN_POINT('Ctrl Pts',(-3.8307526698229,1.,-1.38269750245138));
#45699=CARTESIAN_POINT('Ctrl Pts',(-3.83845502790746,1.,-1.38230274828821));
#45700=CARTESIAN_POINT('Ctrl Pts',(-3.84616425605764,1.,-1.38187013346109));
#45701=CARTESIAN_POINT('Ctrl Pts',(-3.85387983979481,1.,-1.38139983115049));
#45702=CARTESIAN_POINT('Ctrl Pts',(-3.86160143043959,1.,-1.38089205992989));
#45703=CARTESIAN_POINT('Ctrl Pts',(-3.86932885813068,1.,-1.38034709213014));
#45704=CARTESIAN_POINT('Ctrl Pts',(-3.87706205830532,1.,-1.37976523097073));
#45705=CARTESIAN_POINT('Ctrl Pts',(-3.88480102249277,1.,-1.37914679719383));
#45706=CARTESIAN_POINT('Ctrl Pts',(-3.89254574338496,1.,-1.3784921128802));
#45707=CARTESIAN_POINT('Ctrl Pts',(-3.90029615196727,1.,-1.37780148512792));
#45708=CARTESIAN_POINT('Ctrl Pts',(-3.90805209523486,1.,-1.3770751963402));
#45709=CARTESIAN_POINT('Ctrl Pts',(-3.91581337462644,1.,-1.37631350505797));
#45710=CARTESIAN_POINT('Ctrl Pts',(-3.92357976987672,1.,-1.37551664448242));
#45711=CARTESIAN_POINT('Ctrl Pts',(-3.93135106761844,1.,-1.37468482215751));
#45712=CARTESIAN_POINT('Ctrl Pts',(-3.93912709040818,1.,-1.37381821967165));
#45713=CARTESIAN_POINT('Ctrl Pts',(-3.94690771785133,1.,-1.37291699202807));
#45714=CARTESIAN_POINT('Ctrl Pts',(-3.95469287280914,1.,-1.37198126432386));
#45715=CARTESIAN_POINT('Ctrl Pts',(-3.96092458506535,1.,-1.3712051561502));
#45716=CARTESIAN_POINT('Ctrl Pts',(-3.96560037974645,1.,-1.37060761745635));
#45717=CARTESIAN_POINT('Ctrl Pts',(-3.9687184694131,1.,-1.37020239094614));
#45718=CARTESIAN_POINT('Ctrl Pts',(-3.97027773754922,1.,-1.36999806084572));
#45719=CARTESIAN_POINT('Origin',(-3.97027773754922,0.,-1.36999806084572));
#45720=CARTESIAN_POINT('',(-4.01728681790024,1.,-1.22531898815164));
#45721=CARTESIAN_POINT('Origin',(0.,0.,0.));
#45722=CARTESIAN_POINT('',(-3.42859860294378,1.,-1.51895082866166));
#45723=CARTESIAN_POINT('Origin',(0.,1.,0.));
#45724=CARTESIAN_POINT('Ctrl Pts',(-3.42859860294378,1.,-1.51895082866166));
#45725=CARTESIAN_POINT('Ctrl Pts',(-3.42859860294378,0.666666666666667,
-1.51895082866166));
#45726=CARTESIAN_POINT('Ctrl Pts',(-3.42859860294378,0.333333333333333,
-1.51895082866166));
#45727=CARTESIAN_POINT('Ctrl Pts',(-3.42859860294378,-0.333333333333333,
-1.51895082866166));
#45728=CARTESIAN_POINT('Ctrl Pts',(-3.42859860294378,-0.666666666666667,
-1.51895082866166));
#45729=CARTESIAN_POINT('Ctrl Pts',(-3.42859860294378,-1.,-1.51895082866166));
#45730=CARTESIAN_POINT('Ctrl Pts',(-3.77614523045147,-1.,-1.83867539237861));
#45731=CARTESIAN_POINT('Ctrl Pts',(-3.77614523045147,1.,-1.83867539237861));
#45732=CARTESIAN_POINT('Ctrl Pts',(-3.77518714458232,-1.,-1.83742834010821));
#45733=CARTESIAN_POINT('Ctrl Pts',(-3.77518714458232,1.,-1.83742834010821));
#45734=CARTESIAN_POINT('Ctrl Pts',(-3.77326886065484,-1.,-1.83493697935064));
#45735=CARTESIAN_POINT('Ctrl Pts',(-3.77326886065484,1.,-1.83493697935064));
#45736=CARTESIAN_POINT('Ctrl Pts',(-3.77038509819777,-1.,-1.83120816956515));
#45737=CARTESIAN_POINT('Ctrl Pts',(-3.77038509819777,1.,-1.83120816956515));
#45738=CARTESIAN_POINT('Ctrl Pts',(-3.76652740355856,-1.,-1.82625289221933));
#45739=CARTESIAN_POINT('Ctrl Pts',(-3.76652740355856,1.,-1.82625289221933));
#45740=CARTESIAN_POINT('Ctrl Pts',(-3.76168412709652,-1.,-1.82008629694924));
#45741=CARTESIAN_POINT('Ctrl Pts',(-3.76168412709652,1.,-1.82008629694924));
#45742=CARTESIAN_POINT('Ctrl Pts',(-3.75681965683995,-1.,-1.81394729834032));
#45743=CARTESIAN_POINT('Ctrl Pts',(-3.75681965683995,1.,-1.81394729834032));
#45744=CARTESIAN_POINT('Ctrl Pts',(-3.75193395888069,-1.,-1.80783603939662));
#45745=CARTESIAN_POINT('Ctrl Pts',(-3.75193395888069,1.,-1.80783603939662));
#45746=CARTESIAN_POINT('Ctrl Pts',(-3.74702700874954,-1.,-1.80175271485519));
#45747=CARTESIAN_POINT('Ctrl Pts',(-3.74702700874954,1.,-1.80175271485519));
#45748=CARTESIAN_POINT('Ctrl Pts',(-3.74209880351667,-1.,-1.79569757859041));
#45749=CARTESIAN_POINT('Ctrl Pts',(-3.74209880351667,1.,-1.79569757859041));
#45750=CARTESIAN_POINT('Ctrl Pts',(-3.73714934729962,-1.,-1.78967092823139));
#45751=CARTESIAN_POINT('Ctrl Pts',(-3.73714934729962,1.,-1.78967092823139));
#45752=CARTESIAN_POINT('Ctrl Pts',(-3.73217863095022,-1.,-1.78367308442682));
#45753=CARTESIAN_POINT('Ctrl Pts',(-3.73217863095022,1.,-1.78367308442682));
#45754=CARTESIAN_POINT('Ctrl Pts',(-3.72718661205504,-1.,-1.77770437039606));
#45755=CARTESIAN_POINT('Ctrl Pts',(-3.72718661205504,1.,-1.77770437039606));
#45756=CARTESIAN_POINT('Ctrl Pts',(-3.72217319911429,-1.,-1.77176509401846));
#45757=CARTESIAN_POINT('Ctrl Pts',(-3.72217319911429,1.,-1.77176509401846));
#45758=CARTESIAN_POINT('Ctrl Pts',(-3.71713822377675,-1.,-1.76585552124549));
#45759=CARTESIAN_POINT('Ctrl Pts',(-3.71713822377675,1.,-1.76585552124549));
#45760=CARTESIAN_POINT('Ctrl Pts',(-3.71208146346454,-1.,-1.75997588499021));
#45761=CARTESIAN_POINT('Ctrl Pts',(-3.71208146346454,1.,-1.75997588499021));
#45762=CARTESIAN_POINT('Ctrl Pts',(-3.70700269736876,-1.,-1.75412641804148));
#45763=CARTESIAN_POINT('Ctrl Pts',(-3.70700269736876,1.,-1.75412641804148));
#45764=CARTESIAN_POINT('Ctrl Pts',(-3.70190175673422,-1.,-1.74830738046092));
#45765=CARTESIAN_POINT('Ctrl Pts',(-3.70190175673422,1.,-1.74830738046092));
#45766=CARTESIAN_POINT('Ctrl Pts',(-3.6967785691046,-1.,-1.74251908492589));
#45767=CARTESIAN_POINT('Ctrl Pts',(-3.6967785691046,1.,-1.74251908492589));
#45768=CARTESIAN_POINT('Ctrl Pts',(-3.69163322647906,-1.,-1.73676193254493));
#45769=CARTESIAN_POINT('Ctrl Pts',(-3.69163322647906,1.,-1.73676193254493));
#45770=CARTESIAN_POINT('Ctrl Pts',(-3.68646597019188,-1.,-1.73103640956647));
#45771=CARTESIAN_POINT('Ctrl Pts',(-3.68646597019188,1.,-1.73103640956647));
#45772=CARTESIAN_POINT('Ctrl Pts',(-3.68127704936472,-1.,-1.72534302437003));
#45773=CARTESIAN_POINT('Ctrl Pts',(-3.68127704936472,1.,-1.72534302437003));
#45774=CARTESIAN_POINT('Ctrl Pts',(-3.67606660374665,-1.,-1.71968225581787));
#45775=CARTESIAN_POINT('Ctrl Pts',(-3.67606660374665,1.,-1.71968225581787));
#45776=CARTESIAN_POINT('Ctrl Pts',(-3.67083454901629,-1.,-1.71405450210392));
#45777=CARTESIAN_POINT('Ctrl Pts',(-3.67083454901629,1.,-1.71405450210392));
#45778=CARTESIAN_POINT('Ctrl Pts',(-3.6655804319893,-1.,-1.70846001610983));
#45779=CARTESIAN_POINT('Ctrl Pts',(-3.6655804319893,1.,-1.70846001610983));
#45780=CARTESIAN_POINT('Ctrl Pts',(-3.6603033877491,-1.,-1.70289888566904));
#45781=CARTESIAN_POINT('Ctrl Pts',(-3.6603033877491,1.,-1.70289888566904));
#45782=CARTESIAN_POINT('Ctrl Pts',(-3.65500246526798,-1.,-1.69737117722558));
#45783=CARTESIAN_POINT('Ctrl Pts',(-3.65500246526798,1.,-1.69737117722558));
#45784=CARTESIAN_POINT('Ctrl Pts',(-3.64967689827393,-1.,-1.691877054817));
#45785=CARTESIAN_POINT('Ctrl Pts',(-3.64967689827393,1.,-1.691877054817));
#45786=CARTESIAN_POINT('Ctrl Pts',(-3.64432638915199,-1.,-1.68641690471455));
#45787=CARTESIAN_POINT('Ctrl Pts',(-3.64432638915199,1.,-1.68641690471455));
#45788=CARTESIAN_POINT('Ctrl Pts',(-3.63895140887443,-1.,-1.68099146651577));
#45789=CARTESIAN_POINT('Ctrl Pts',(-3.63895140887443,1.,-1.68099146651577));
#45790=CARTESIAN_POINT('Ctrl Pts',(-3.63355343201211,-1.,-1.67560193613145));
#45791=CARTESIAN_POINT('Ctrl Pts',(-3.63355343201211,1.,-1.67560193613145));
#45792=CARTESIAN_POINT('Ctrl Pts',(-3.62813422105257,-1.,-1.67024966008037));
#45793=CARTESIAN_POINT('Ctrl Pts',(-3.62813422105257,1.,-1.67024966008037));
#45794=CARTESIAN_POINT('Ctrl Pts',(-3.62269517989104,-1.,-1.66493585923853));
#45795=CARTESIAN_POINT('Ctrl Pts',(-3.62269517989104,1.,-1.66493585923853));
#45796=CARTESIAN_POINT('Ctrl Pts',(-3.61723666482457,-1.,-1.65966133399186));
#45797=CARTESIAN_POINT('Ctrl Pts',(-3.61723666482457,1.,-1.65966133399186));
#45798=CARTESIAN_POINT('Ctrl Pts',(-3.61175734965129,-1.,-1.65442619244327));
#45799=CARTESIAN_POINT('Ctrl Pts',(-3.61175734965129,1.,-1.65442619244327));
#45800=CARTESIAN_POINT('Ctrl Pts',(-3.60625346556992,-1.,-1.64922952425833));
#45801=CARTESIAN_POINT('Ctrl Pts',(-3.60625346556992,1.,-1.64922952425833));
#45802=CARTESIAN_POINT('Ctrl Pts',(-3.6007202851384,-1.,-1.6440700438558));
#45803=CARTESIAN_POINT('Ctrl Pts',(-3.6007202851384,1.,-1.6440700438558));
#45804=CARTESIAN_POINT('Ctrl Pts',(-3.59515368334887,-1.,-1.63894676675349));
#45805=CARTESIAN_POINT('Ctrl Pts',(-3.59515368334887,1.,-1.63894676675349));
#45806=CARTESIAN_POINT('Ctrl Pts',(-3.58955176627876,-1.,-1.63385971451259));
#45807=CARTESIAN_POINT('Ctrl Pts',(-3.58955176627876,1.,-1.63385971451259));
#45808=CARTESIAN_POINT('Ctrl Pts',(-3.5839162577435,-1.,-1.62881051550748));
#45809=CARTESIAN_POINT('Ctrl Pts',(-3.5839162577435,1.,-1.62881051550748));
#45810=CARTESIAN_POINT('Ctrl Pts',(-3.57825455954405,-1.,-1.62380329464851));
#45811=CARTESIAN_POINT('Ctrl Pts',(-3.57825455954405,1.,-1.62380329464851));
#45812=CARTESIAN_POINT('Ctrl Pts',(-3.57257679609826,-1.,-1.61884340915412));
#45813=CARTESIAN_POINT('Ctrl Pts',(-3.57257679609826,1.,-1.61884340915412));
#45814=CARTESIAN_POINT('Ctrl Pts',(-3.56689200468404,-1.,-1.61393581747522));
#45815=CARTESIAN_POINT('Ctrl Pts',(-3.56689200468404,1.,-1.61393581747522));
#45816=CARTESIAN_POINT('Ctrl Pts',(-3.56120432482986,-1.,-1.60908344685459));
#45817=CARTESIAN_POINT('Ctrl Pts',(-3.56120432482986,1.,-1.60908344685459));
#45818=CARTESIAN_POINT('Ctrl Pts',(-3.55550985096117,-1.,-1.60428584699848));
#45819=CARTESIAN_POINT('Ctrl Pts',(-3.55550985096117,1.,-1.60428584699848));
#45820=CARTESIAN_POINT('Ctrl Pts',(-3.54979148634426,-1.,-1.59953698113444));
#45821=CARTESIAN_POINT('Ctrl Pts',(-3.54979148634426,1.,-1.59953698113444));
#45822=CARTESIAN_POINT('Ctrl Pts',(-3.544024581823,-1.,-1.5948276694975));
#45823=CARTESIAN_POINT('Ctrl Pts',(-3.544024581823,1.,-1.5948276694975));
#45824=CARTESIAN_POINT('Ctrl Pts',(-3.53818616861045,-1.,-1.59014958368725));
#45825=CARTESIAN_POINT('Ctrl Pts',(-3.53818616861045,1.,-1.59014958368725));
#45826=CARTESIAN_POINT('Ctrl Pts',(-3.53226378147068,-1.,-1.58549906268083));
#45827=CARTESIAN_POINT('Ctrl Pts',(-3.53226378147068,1.,-1.58549906268083));
#45828=CARTESIAN_POINT('Ctrl Pts',(-3.52626275334899,-1.,-1.58088027227856));
#45829=CARTESIAN_POINT('Ctrl Pts',(-3.52626275334899,1.,-1.58088027227856));
#45830=CARTESIAN_POINT('Ctrl Pts',(-3.52021847865961,-1.,-1.5763104998818));
#45831=CARTESIAN_POINT('Ctrl Pts',(-3.52021847865961,1.,-1.5763104998818));
#45832=CARTESIAN_POINT('Ctrl Pts',(-3.51418598431733,-1.,-1.57181569799774));
#45833=CARTESIAN_POINT('Ctrl Pts',(-3.51418598431733,1.,-1.57181569799774));
#45834=CARTESIAN_POINT('Ctrl Pts',(-3.50821771695427,-1.,-1.56742097575041));
#45835=CARTESIAN_POINT('Ctrl Pts',(-3.50821771695427,1.,-1.56742097575041));
#45836=CARTESIAN_POINT('Ctrl Pts',(-3.50234321621607,-1.,-1.56314187758689));
#45837=CARTESIAN_POINT('Ctrl Pts',(-3.50234321621607,1.,-1.56314187758689));
#45838=CARTESIAN_POINT('Ctrl Pts',(-3.49655185179623,-1.,-1.55897703097859));
#45839=CARTESIAN_POINT('Ctrl Pts',(-3.49655185179623,1.,-1.55897703097859));
#45840=CARTESIAN_POINT('Ctrl Pts',(-3.49076460877317,-1.,-1.5548959590107));
#45841=CARTESIAN_POINT('Ctrl Pts',(-3.49076460877317,1.,-1.5548959590107));
#45842=CARTESIAN_POINT('Ctrl Pts',(-3.48485155928414,-1.,-1.55084702970382));
#45843=CARTESIAN_POINT('Ctrl Pts',(-3.48485155928414,1.,-1.55084702970382));
#45844=CARTESIAN_POINT('Ctrl Pts',(-3.47868272898599,-1.,-1.54678009290206));
#45845=CARTESIAN_POINT('Ctrl Pts',(-3.47868272898599,1.,-1.54678009290206));
#45846=CARTESIAN_POINT('Ctrl Pts',(-3.47217189224576,-1.,-1.54266605398152));
#45847=CARTESIAN_POINT('Ctrl Pts',(-3.47217189224576,1.,-1.54266605398152));
#45848=CARTESIAN_POINT('Ctrl Pts',(-3.46531752207222,-1.,-1.53851507915533));
#45849=CARTESIAN_POINT('Ctrl Pts',(-3.46531752207222,1.,-1.53851507915533));
#45850=CARTESIAN_POINT('Ctrl Pts',(-3.45825932955273,-1.,-1.53440195378902));
#45851=CARTESIAN_POINT('Ctrl Pts',(-3.45825932955273,1.,-1.53440195378902));
#45852=CARTESIAN_POINT('Ctrl Pts',(-3.45127136828667,-1.,-1.530462444618));
#45853=CARTESIAN_POINT('Ctrl Pts',(-3.45127136828667,1.,-1.530462444618));
#45854=CARTESIAN_POINT('Ctrl Pts',(-3.44469547527,-1.,-1.52686242875717));
#45855=CARTESIAN_POINT('Ctrl Pts',(-3.44469547527,1.,-1.52686242875717));
#45856=CARTESIAN_POINT('Ctrl Pts',(-3.43888895974182,-1.,-1.52377348950429));
#45857=CARTESIAN_POINT('Ctrl Pts',(-3.43888895974182,1.,-1.52377348950429));
#45858=CARTESIAN_POINT('Ctrl Pts',(-3.43417156977749,-1.,-1.52134826724227));
#45859=CARTESIAN_POINT('Ctrl Pts',(-3.43417156977749,1.,-1.52134826724227));
#45860=CARTESIAN_POINT('Ctrl Pts',(-3.43076036253384,-1.,-1.51969006980792));
#45861=CARTESIAN_POINT('Ctrl Pts',(-3.43076036253384,1.,-1.51969006980792));
#45862=CARTESIAN_POINT('Ctrl Pts',(-3.42915787669388,-1.,-1.51901585838879));
#45863=CARTESIAN_POINT('Ctrl Pts',(-3.42915787669388,1.,-1.51901585838879));
#45864=CARTESIAN_POINT('Ctrl Pts',(-3.42860527148835,-1.,-1.51888450659497));
#45865=CARTESIAN_POINT('Ctrl Pts',(-3.42860527148835,1.,-1.51888450659497));
#45866=CARTESIAN_POINT('Ctrl Pts',(-3.42852521763648,-1.,-1.51896318668306));
#45867=CARTESIAN_POINT('Ctrl Pts',(-3.42852521763648,1.,-1.51896318668306));
#45868=CARTESIAN_POINT('Ctrl Pts',(-3.42855728381368,-1.,-1.519044091397));
#45869=CARTESIAN_POINT('Ctrl Pts',(-3.42855728381368,1.,-1.519044091397));
#45870=CARTESIAN_POINT('',(-3.77614523045147,1.,-1.83867539237861));
#45871=CARTESIAN_POINT('Ctrl Pts',(-3.77614523045147,1.,-1.83867539237861));
#45872=CARTESIAN_POINT('Ctrl Pts',(-3.77518714458232,1.,-1.83742834010821));
#45873=CARTESIAN_POINT('Ctrl Pts',(-3.77326886065484,1.,-1.83493697935064));
#45874=CARTESIAN_POINT('Ctrl Pts',(-3.77038509819777,1.,-1.83120816956515));
#45875=CARTESIAN_POINT('Ctrl Pts',(-3.76652740355856,1.,-1.82625289221933));
#45876=CARTESIAN_POINT('Ctrl Pts',(-3.76168412709652,1.,-1.82008629694924));
#45877=CARTESIAN_POINT('Ctrl Pts',(-3.75681965683995,1.,-1.81394729834032));
#45878=CARTESIAN_POINT('Ctrl Pts',(-3.75193395888069,1.,-1.80783603939662));
#45879=CARTESIAN_POINT('Ctrl Pts',(-3.74702700874954,1.,-1.80175271485519));
#45880=CARTESIAN_POINT('Ctrl Pts',(-3.74209880351667,1.,-1.79569757859041));
#45881=CARTESIAN_POINT('Ctrl Pts',(-3.73714934729962,1.,-1.78967092823139));
#45882=CARTESIAN_POINT('Ctrl Pts',(-3.73217863095022,1.,-1.78367308442682));
#45883=CARTESIAN_POINT('Ctrl Pts',(-3.72718661205504,1.,-1.77770437039606));
#45884=CARTESIAN_POINT('Ctrl Pts',(-3.72217319911429,1.,-1.77176509401846));
#45885=CARTESIAN_POINT('Ctrl Pts',(-3.71713822377675,1.,-1.76585552124549));
#45886=CARTESIAN_POINT('Ctrl Pts',(-3.71208146346454,1.,-1.75997588499021));
#45887=CARTESIAN_POINT('Ctrl Pts',(-3.70700269736876,1.,-1.75412641804148));
#45888=CARTESIAN_POINT('Ctrl Pts',(-3.70190175673422,1.,-1.74830738046092));
#45889=CARTESIAN_POINT('Ctrl Pts',(-3.6967785691046,1.,-1.74251908492589));
#45890=CARTESIAN_POINT('Ctrl Pts',(-3.69163322647906,1.,-1.73676193254493));
#45891=CARTESIAN_POINT('Ctrl Pts',(-3.68646597019188,1.,-1.73103640956647));
#45892=CARTESIAN_POINT('Ctrl Pts',(-3.68127704936472,1.,-1.72534302437003));
#45893=CARTESIAN_POINT('Ctrl Pts',(-3.67606660374665,1.,-1.71968225581787));
#45894=CARTESIAN_POINT('Ctrl Pts',(-3.67083454901629,1.,-1.71405450210392));
#45895=CARTESIAN_POINT('Ctrl Pts',(-3.6655804319893,1.,-1.70846001610983));
#45896=CARTESIAN_POINT('Ctrl Pts',(-3.6603033877491,1.,-1.70289888566904));
#45897=CARTESIAN_POINT('Ctrl Pts',(-3.65500246526798,1.,-1.69737117722558));
#45898=CARTESIAN_POINT('Ctrl Pts',(-3.64967689827393,1.,-1.691877054817));
#45899=CARTESIAN_POINT('Ctrl Pts',(-3.64432638915199,1.,-1.68641690471455));
#45900=CARTESIAN_POINT('Ctrl Pts',(-3.63895140887443,1.,-1.68099146651577));
#45901=CARTESIAN_POINT('Ctrl Pts',(-3.63355343201211,1.,-1.67560193613145));
#45902=CARTESIAN_POINT('Ctrl Pts',(-3.62813422105257,1.,-1.67024966008037));
#45903=CARTESIAN_POINT('Ctrl Pts',(-3.62269517989104,1.,-1.66493585923853));
#45904=CARTESIAN_POINT('Ctrl Pts',(-3.61723666482457,1.,-1.65966133399186));
#45905=CARTESIAN_POINT('Ctrl Pts',(-3.61175734965129,1.,-1.65442619244327));
#45906=CARTESIAN_POINT('Ctrl Pts',(-3.60625346556992,1.,-1.64922952425833));
#45907=CARTESIAN_POINT('Ctrl Pts',(-3.6007202851384,1.,-1.6440700438558));
#45908=CARTESIAN_POINT('Ctrl Pts',(-3.59515368334887,1.,-1.63894676675349));
#45909=CARTESIAN_POINT('Ctrl Pts',(-3.58955176627876,1.,-1.63385971451259));
#45910=CARTESIAN_POINT('Ctrl Pts',(-3.5839162577435,1.,-1.62881051550748));
#45911=CARTESIAN_POINT('Ctrl Pts',(-3.57825455954405,1.,-1.62380329464851));
#45912=CARTESIAN_POINT('Ctrl Pts',(-3.57257679609826,1.,-1.61884340915412));
#45913=CARTESIAN_POINT('Ctrl Pts',(-3.56689200468404,1.,-1.61393581747522));
#45914=CARTESIAN_POINT('Ctrl Pts',(-3.56120432482986,1.,-1.60908344685459));
#45915=CARTESIAN_POINT('Ctrl Pts',(-3.55550985096117,1.,-1.60428584699848));
#45916=CARTESIAN_POINT('Ctrl Pts',(-3.54979148634426,1.,-1.59953698113444));
#45917=CARTESIAN_POINT('Ctrl Pts',(-3.544024581823,1.,-1.5948276694975));
#45918=CARTESIAN_POINT('Ctrl Pts',(-3.53818616861045,1.,-1.59014958368725));
#45919=CARTESIAN_POINT('Ctrl Pts',(-3.53226378147068,1.,-1.58549906268083));
#45920=CARTESIAN_POINT('Ctrl Pts',(-3.52626275334899,1.,-1.58088027227856));
#45921=CARTESIAN_POINT('Ctrl Pts',(-3.52021847865961,1.,-1.5763104998818));
#45922=CARTESIAN_POINT('Ctrl Pts',(-3.51418598431733,1.,-1.57181569799774));
#45923=CARTESIAN_POINT('Ctrl Pts',(-3.50821771695427,1.,-1.56742097575041));
#45924=CARTESIAN_POINT('Ctrl Pts',(-3.50234321621607,1.,-1.56314187758689));
#45925=CARTESIAN_POINT('Ctrl Pts',(-3.49655185179623,1.,-1.55897703097859));
#45926=CARTESIAN_POINT('Ctrl Pts',(-3.49076460877317,1.,-1.5548959590107));
#45927=CARTESIAN_POINT('Ctrl Pts',(-3.48485155928414,1.,-1.55084702970382));
#45928=CARTESIAN_POINT('Ctrl Pts',(-3.47868272898599,1.,-1.54678009290206));
#45929=CARTESIAN_POINT('Ctrl Pts',(-3.47217189224576,1.,-1.54266605398152));
#45930=CARTESIAN_POINT('Ctrl Pts',(-3.46531752207222,1.,-1.53851507915533));
#45931=CARTESIAN_POINT('Ctrl Pts',(-3.45825932955273,1.,-1.53440195378902));
#45932=CARTESIAN_POINT('Ctrl Pts',(-3.45127136828667,1.,-1.530462444618));
#45933=CARTESIAN_POINT('Ctrl Pts',(-3.44469547527,1.,-1.52686242875717));
#45934=CARTESIAN_POINT('Ctrl Pts',(-3.43888895974182,1.,-1.52377348950429));
#45935=CARTESIAN_POINT('Ctrl Pts',(-3.43417156977749,1.,-1.52134826724227));
#45936=CARTESIAN_POINT('Ctrl Pts',(-3.43101631893491,1.,-1.5198144909343));
#45937=CARTESIAN_POINT('Ctrl Pts',(-3.42946838852728,1.,-1.51914806898539));
#45938=CARTESIAN_POINT('Ctrl Pts',(-3.42884302333978,1.,-1.51895133295017));
#45939=CARTESIAN_POINT('Ctrl Pts',(-3.42864616361967,1.,-1.51893924967231));
#45940=CARTESIAN_POINT('Ctrl Pts',(-3.42859860294378,1.,-1.51895082866166));
#45941=CARTESIAN_POINT('',(-3.77614523045147,0.,-1.83867539237861));
#45942=CARTESIAN_POINT('Ctrl Pts',(-3.24418789321065,-1.,-1.8808893942881));
#45943=CARTESIAN_POINT('Ctrl Pts',(-3.24418789321065,1.,-1.8808893942881));
#45944=CARTESIAN_POINT('Ctrl Pts',(-3.24410359189733,-1.,-1.8809110068042));
#45945=CARTESIAN_POINT('Ctrl Pts',(-3.24410359189733,1.,-1.8809110068042));
#45946=CARTESIAN_POINT('Ctrl Pts',(-3.24408699284449,-1.,-1.8810220187274));
#45947=CARTESIAN_POINT('Ctrl Pts',(-3.24408699284449,1.,-1.8810220187274));
#45948=CARTESIAN_POINT('Ctrl Pts',(-3.24451807186964,-1.,-1.88139187908347));
#45949=CARTESIAN_POINT('Ctrl Pts',(-3.24451807186964,1.,-1.88139187908347));
#45950=CARTESIAN_POINT('Ctrl Pts',(-3.24600543790876,-1.,-1.88229202583187));
#45951=CARTESIAN_POINT('Ctrl Pts',(-3.24600543790876,1.,-1.88229202583187));
#45952=CARTESIAN_POINT('Ctrl Pts',(-3.24935200512055,-1.,-1.88407708646435));
#45953=CARTESIAN_POINT('Ctrl Pts',(-3.24935200512055,1.,-1.88407708646435));
#45954=CARTESIAN_POINT('Ctrl Pts',(-3.25408686339298,-1.,-1.88646802523372));
#45955=CARTESIAN_POINT('Ctrl Pts',(-3.25408686339298,1.,-1.88646802523372));
#45956=CARTESIAN_POINT('Ctrl Pts',(-3.2599988519361,-1.,-1.88934996203508));
#45957=CARTESIAN_POINT('Ctrl Pts',(-3.2599988519361,1.,-1.88934996203508));
#45958=CARTESIAN_POINT('Ctrl Pts',(-3.2667765388833,-1.,-1.89255393500769));
#45959=CARTESIAN_POINT('Ctrl Pts',(-3.2667765388833,1.,-1.89255393500769));
#45960=CARTESIAN_POINT('Ctrl Pts',(-3.27407108932908,-1.,-1.89589172903662));
#45961=CARTESIAN_POINT('Ctrl Pts',(-3.27407108932908,1.,-1.89589172903662));
#45962=CARTESIAN_POINT('Ctrl Pts',(-3.28154737912287,-1.,-1.89918429230424));
#45963=CARTESIAN_POINT('Ctrl Pts',(-3.28154737912287,1.,-1.89918429230424));
#45964=CARTESIAN_POINT('Ctrl Pts',(-3.28893448600364,-1.,-1.9022897124757));
#45965=CARTESIAN_POINT('Ctrl Pts',(-3.28893448600364,1.,-1.9022897124757));
#45966=CARTESIAN_POINT('Ctrl Pts',(-3.29608978722258,-1.,-1.9051389186417));
#45967=CARTESIAN_POINT('Ctrl Pts',(-3.29608978722258,1.,-1.9051389186417));
#45968=CARTESIAN_POINT('Ctrl Pts',(-3.30300595568341,-1.,-1.90773912171424));
#45969=CARTESIAN_POINT('Ctrl Pts',(-3.30300595568341,1.,-1.90773912171424));
#45970=CARTESIAN_POINT('Ctrl Pts',(-3.30975721158694,-1.,-1.91014297830502));
#45971=CARTESIAN_POINT('Ctrl Pts',(-3.30975721158694,1.,-1.91014297830502));
#45972=CARTESIAN_POINT('Ctrl Pts',(-3.31646052426395,-1.,-1.91242616234459));
#45973=CARTESIAN_POINT('Ctrl Pts',(-3.31646052426395,1.,-1.91242616234459));
#45974=CARTESIAN_POINT('Ctrl Pts',(-3.32323403454507,-1.,-1.91466343916612));
#45975=CARTESIAN_POINT('Ctrl Pts',(-3.32323403454507,1.,-1.91466343916612));
#45976=CARTESIAN_POINT('Ctrl Pts',(-3.33014884257812,-1.,-1.91690081930297));
#45977=CARTESIAN_POINT('Ctrl Pts',(-3.33014884257812,1.,-1.91690081930297));
#45978=CARTESIAN_POINT('Ctrl Pts',(-3.33721230709948,-1.,-1.91914609610173));
#45979=CARTESIAN_POINT('Ctrl Pts',(-3.33721230709948,1.,-1.91914609610173));
#45980=CARTESIAN_POINT('Ctrl Pts',(-3.34439448941915,-1.,-1.92138450828378));
#45981=CARTESIAN_POINT('Ctrl Pts',(-3.34439448941915,1.,-1.92138450828378));
#45982=CARTESIAN_POINT('Ctrl Pts',(-3.35164424847206,-1.,-1.92358838440518));
#45983=CARTESIAN_POINT('Ctrl Pts',(-3.35164424847206,1.,-1.92358838440518));
#45984=CARTESIAN_POINT('Ctrl Pts',(-3.35890824422976,-1.,-1.92572846125763));
#45985=CARTESIAN_POINT('Ctrl Pts',(-3.35890824422976,1.,-1.92572846125763));
#45986=CARTESIAN_POINT('Ctrl Pts',(-3.36615168657597,-1.,-1.92778626543803));
#45987=CARTESIAN_POINT('Ctrl Pts',(-3.36615168657597,1.,-1.92778626543803));
#45988=CARTESIAN_POINT('Ctrl Pts',(-3.37336807068078,-1.,-1.92975993109897));
#45989=CARTESIAN_POINT('Ctrl Pts',(-3.37336807068078,1.,-1.92975993109897));
#45990=CARTESIAN_POINT('Ctrl Pts',(-3.38056768525577,-1.,-1.93165739093292));
#45991=CARTESIAN_POINT('Ctrl Pts',(-3.38056768525577,1.,-1.93165739093292));
#45992=CARTESIAN_POINT('Ctrl Pts',(-3.38777076883267,-1.,-1.93349233176794));
#45993=CARTESIAN_POINT('Ctrl Pts',(-3.38777076883267,1.,-1.93349233176794));
#45994=CARTESIAN_POINT('Ctrl Pts',(-3.39499923640789,-1.,-1.93527929945982));
#45995=CARTESIAN_POINT('Ctrl Pts',(-3.39499923640789,1.,-1.93527929945982));
#45996=CARTESIAN_POINT('Ctrl Pts',(-3.40226802104093,-1.,-1.93702857723089));
#45997=CARTESIAN_POINT('Ctrl Pts',(-3.40226802104093,1.,-1.93702857723089));
#45998=CARTESIAN_POINT('Ctrl Pts',(-3.40957978266622,-1.,-1.93874306008132));
#45999=CARTESIAN_POINT('Ctrl Pts',(-3.40957978266622,1.,-1.93874306008132));
#46000=CARTESIAN_POINT('Ctrl Pts',(-3.41692971994082,-1.,-1.94042111965237));
#46001=CARTESIAN_POINT('Ctrl Pts',(-3.41692971994082,1.,-1.94042111965237));
#46002=CARTESIAN_POINT('Ctrl Pts',(-3.42430850941497,-1.,-1.94205835913692));
#46003=CARTESIAN_POINT('Ctrl Pts',(-3.42430850941497,1.,-1.94205835913692));
#46004=CARTESIAN_POINT('Ctrl Pts',(-3.43170586602436,-1.,-1.94364973660285));
#46005=CARTESIAN_POINT('Ctrl Pts',(-3.43170586602436,1.,-1.94364973660285));
#46006=CARTESIAN_POINT('Ctrl Pts',(-3.43911410197693,-1.,-1.94519168842883));
#46007=CARTESIAN_POINT('Ctrl Pts',(-3.43911410197693,1.,-1.94519168842883));
#46008=CARTESIAN_POINT('Ctrl Pts',(-3.44653088665685,-1.,-1.94668377715332));
#46009=CARTESIAN_POINT('Ctrl Pts',(-3.44653088665685,1.,-1.94668377715332));
#46010=CARTESIAN_POINT('Ctrl Pts',(-3.45395731584051,-1.,-1.94812754766524));
#46011=CARTESIAN_POINT('Ctrl Pts',(-3.45395731584051,1.,-1.94812754766524));
#46012=CARTESIAN_POINT('Ctrl Pts',(-3.46139661060959,-1.,-1.94952575850196));
#46013=CARTESIAN_POINT('Ctrl Pts',(-3.46139661060959,1.,-1.94952575850196));
#46014=CARTESIAN_POINT('Ctrl Pts',(-3.4688525897419,-1.,-1.95088147859876));
#46015=CARTESIAN_POINT('Ctrl Pts',(-3.4688525897419,1.,-1.95088147859876));
#46016=CARTESIAN_POINT('Ctrl Pts',(-3.47632820495926,-1.,-1.95219722189878));
#46017=CARTESIAN_POINT('Ctrl Pts',(-3.47632820495926,1.,-1.95219722189878));
#46018=CARTESIAN_POINT('Ctrl Pts',(-3.48382414832648,-1.,-1.95347412486316));
#46019=CARTESIAN_POINT('Ctrl Pts',(-3.48382414832648,1.,-1.95347412486316));
#46020=CARTESIAN_POINT('Ctrl Pts',(-3.49133956289154,-1.,-1.95471236969653));
#46021=CARTESIAN_POINT('Ctrl Pts',(-3.49133956289154,1.,-1.95471236969653));
#46022=CARTESIAN_POINT('Ctrl Pts',(-3.49887263575602,-1.,-1.9559115382367));
#46023=CARTESIAN_POINT('Ctrl Pts',(-3.49887263575602,1.,-1.9559115382367));
#46024=CARTESIAN_POINT('Ctrl Pts',(-3.50642124159913,-1.,-1.95707099606513));
#46025=CARTESIAN_POINT('Ctrl Pts',(-3.50642124159913,1.,-1.95707099606513));
#46026=CARTESIAN_POINT('Ctrl Pts',(-3.51398354617772,-1.,-1.95819025316768));
#46027=CARTESIAN_POINT('Ctrl Pts',(-3.51398354617772,1.,-1.95819025316768));
#46028=CARTESIAN_POINT('Ctrl Pts',(-3.52155867431438,-1.,-1.95926936324436));
#46029=CARTESIAN_POINT('Ctrl Pts',(-3.52155867431438,1.,-1.95926936324436));
#46030=CARTESIAN_POINT('Ctrl Pts',(-3.52914648844289,-1.,-1.96030879411534));
#46031=CARTESIAN_POINT('Ctrl Pts',(-3.52914648844289,1.,-1.96030879411534));
#46032=CARTESIAN_POINT('Ctrl Pts',(-3.53674730625759,-1.,-1.96130926212661));
#46033=CARTESIAN_POINT('Ctrl Pts',(-3.53674730625759,1.,-1.96130926212661));
#46034=CARTESIAN_POINT('Ctrl Pts',(-3.54436163300425,-1.,-1.96227157573058));
#46035=CARTESIAN_POINT('Ctrl Pts',(-3.54436163300425,1.,-1.96227157573058));
#46036=CARTESIAN_POINT('Ctrl Pts',(-3.55198990600929,-1.,-1.96319648628667));
#46037=CARTESIAN_POINT('Ctrl Pts',(-3.55198990600929,1.,-1.96319648628667));
#46038=CARTESIAN_POINT('Ctrl Pts',(-3.55963218706201,-1.,-1.96408450906868));
#46039=CARTESIAN_POINT('Ctrl Pts',(-3.55963218706201,1.,-1.96408450906868));
#46040=CARTESIAN_POINT('Ctrl Pts',(-3.56728820357933,-1.,-1.96493594634643));
#46041=CARTESIAN_POINT('Ctrl Pts',(-3.56728820357933,1.,-1.96493594634643));
#46042=CARTESIAN_POINT('Ctrl Pts',(-3.57495748601088,-1.,-1.96575096652857));
#46043=CARTESIAN_POINT('Ctrl Pts',(-3.57495748601088,1.,-1.96575096652857));
#46044=CARTESIAN_POINT('Ctrl Pts',(-3.58263947663884,-1.,-1.9665296668894));
#46045=CARTESIAN_POINT('Ctrl Pts',(-3.58263947663884,1.,-1.9665296668894));
#46046=CARTESIAN_POINT('Ctrl Pts',(-3.5903336402273,-1.,-1.96727213799507));
#46047=CARTESIAN_POINT('Ctrl Pts',(-3.5903336402273,1.,-1.96727213799507));
#46048=CARTESIAN_POINT('Ctrl Pts',(-3.59803959819725,-1.,-1.96797854118257));
#46049=CARTESIAN_POINT('Ctrl Pts',(-3.59803959819725,1.,-1.96797854118257));
#46050=CARTESIAN_POINT('Ctrl Pts',(-3.60575714017676,-1.,-1.96864911885775));
#46051=CARTESIAN_POINT('Ctrl Pts',(-3.60575714017676,1.,-1.96864911885775));
#46052=CARTESIAN_POINT('Ctrl Pts',(-3.61348615496393,-1.,-1.96928416040712));
#46053=CARTESIAN_POINT('Ctrl Pts',(-3.61348615496393,1.,-1.96928416040712));
#46054=CARTESIAN_POINT('Ctrl Pts',(-3.62122658401722,-1.,-1.96988398129888));
#46055=CARTESIAN_POINT('Ctrl Pts',(-3.62122658401722,1.,-1.96988398129888));
#46056=CARTESIAN_POINT('Ctrl Pts',(-3.62897836973397,-1.,-1.97044889850518));
#46057=CARTESIAN_POINT('Ctrl Pts',(-3.62897836973397,1.,-1.97044889850518));
#46058=CARTESIAN_POINT('Ctrl Pts',(-3.63674139590853,-1.,-1.97097920454698));
#46059=CARTESIAN_POINT('Ctrl Pts',(-3.63674139590853,1.,-1.97097920454698));
#46060=CARTESIAN_POINT('Ctrl Pts',(-3.64451546724221,-1.,-1.97147515441539));
#46061=CARTESIAN_POINT('Ctrl Pts',(-3.64451546724221,1.,-1.97147515441539));
#46062=CARTESIAN_POINT('Ctrl Pts',(-3.65230034717364,-1.,-1.97193697240645));
#46063=CARTESIAN_POINT('Ctrl Pts',(-3.65230034717364,1.,-1.97193697240645));
#46064=CARTESIAN_POINT('Ctrl Pts',(-3.66009578166865,-1.,-1.97236485439317));
#46065=CARTESIAN_POINT('Ctrl Pts',(-3.66009578166865,1.,-1.97236485439317));
#46066=CARTESIAN_POINT('Ctrl Pts',(-3.66790152751984,-1.,-1.9727589719863));
#46067=CARTESIAN_POINT('Ctrl Pts',(-3.66790152751984,1.,-1.9727589719863));
#46068=CARTESIAN_POINT('Ctrl Pts',(-3.67571738106175,-1.,-1.97311947678035));
#46069=CARTESIAN_POINT('Ctrl Pts',(-3.67571738106175,1.,-1.97311947678035));
#46070=CARTESIAN_POINT('Ctrl Pts',(-3.68354319913416,-1.,-1.9734465030363));
#46071=CARTESIAN_POINT('Ctrl Pts',(-3.68354319913416,1.,-1.9734465030363));
#46072=CARTESIAN_POINT('Ctrl Pts',(-3.69137888597855,-1.,-1.97374016224397));
#46073=CARTESIAN_POINT('Ctrl Pts',(-3.69137888597855,1.,-1.97374016224397));
#46074=CARTESIAN_POINT('Ctrl Pts',(-3.69765528558292,-1.,-1.97394846382288));
#46075=CARTESIAN_POINT('Ctrl Pts',(-3.69765528558292,1.,-1.97394846382288));
#46076=CARTESIAN_POINT('Ctrl Pts',(-3.70236698911837,-1.,-1.97408973726149));
#46077=CARTESIAN_POINT('Ctrl Pts',(-3.70236698911837,1.,-1.97408973726149));
#46078=CARTESIAN_POINT('Ctrl Pts',(-3.7055100813194,-1.,-1.974177276451));
#46079=CARTESIAN_POINT('Ctrl Pts',(-3.7055100813194,1.,-1.974177276451));
#46080=CARTESIAN_POINT('Ctrl Pts',(-3.70708211654725,-1.,-1.97421938526992));
#46081=CARTESIAN_POINT('Ctrl Pts',(-3.70708211654725,1.,-1.97421938526992));
#46082=CARTESIAN_POINT('',(-3.24413672884902,1.,-1.88097764062542));
#46083=CARTESIAN_POINT('Ctrl Pts',(-3.24413672884902,-1.,-1.88097764062542));
#46084=CARTESIAN_POINT('Ctrl Pts',(-3.24413672884902,-0.666666666666667,
-1.88097764062542));
#46085=CARTESIAN_POINT('Ctrl Pts',(-3.24413672884902,-0.333333333333333,
-1.88097764062542));
#46086=CARTESIAN_POINT('Ctrl Pts',(-3.24413672884902,0.333333333333333,
-1.88097764062542));
#46087=CARTESIAN_POINT('Ctrl Pts',(-3.24413672884902,0.666666666666667,
-1.88097764062542));
#46088=CARTESIAN_POINT('Ctrl Pts',(-3.24413672884902,1.,-1.88097764062542));
#46089=CARTESIAN_POINT('',(-3.70708211654725,1.,-1.97421938526992));
#46090=CARTESIAN_POINT('',(-3.70708211654725,0.,-1.97421938526992));
#46091=CARTESIAN_POINT('Ctrl Pts',(-3.24413672884902,1.,-1.88097764062542));
#46092=CARTESIAN_POINT('Ctrl Pts',(-3.24415531671311,1.,-1.88102292397987));
#46093=CARTESIAN_POINT('Ctrl Pts',(-3.24428080352952,1.,-1.88117508446657));
#46094=CARTESIAN_POINT('Ctrl Pts',(-3.24480754675942,1.,-1.88156537699118));
#46095=CARTESIAN_POINT('Ctrl Pts',(-3.24625654410705,1.,-1.88242596600422));
#46096=CARTESIAN_POINT('Ctrl Pts',(-3.24935200512055,1.,-1.88407708646435));
#46097=CARTESIAN_POINT('Ctrl Pts',(-3.25408686339298,1.,-1.88646802523372));
#46098=CARTESIAN_POINT('Ctrl Pts',(-3.2599988519361,1.,-1.88934996203508));
#46099=CARTESIAN_POINT('Ctrl Pts',(-3.2667765388833,1.,-1.89255393500769));
#46100=CARTESIAN_POINT('Ctrl Pts',(-3.27407108932908,1.,-1.89589172903662));
#46101=CARTESIAN_POINT('Ctrl Pts',(-3.28154737912287,1.,-1.89918429230424));
#46102=CARTESIAN_POINT('Ctrl Pts',(-3.28893448600364,1.,-1.9022897124757));
#46103=CARTESIAN_POINT('Ctrl Pts',(-3.29608978722258,1.,-1.9051389186417));
#46104=CARTESIAN_POINT('Ctrl Pts',(-3.30300595568341,1.,-1.90773912171424));
#46105=CARTESIAN_POINT('Ctrl Pts',(-3.30975721158694,1.,-1.91014297830502));
#46106=CARTESIAN_POINT('Ctrl Pts',(-3.31646052426395,1.,-1.91242616234459));
#46107=CARTESIAN_POINT('Ctrl Pts',(-3.32323403454507,1.,-1.91466343916612));
#46108=CARTESIAN_POINT('Ctrl Pts',(-3.33014884257812,1.,-1.91690081930297));
#46109=CARTESIAN_POINT('Ctrl Pts',(-3.33721230709948,1.,-1.91914609610173));
#46110=CARTESIAN_POINT('Ctrl Pts',(-3.34439448941915,1.,-1.92138450828378));
#46111=CARTESIAN_POINT('Ctrl Pts',(-3.35164424847206,1.,-1.92358838440518));
#46112=CARTESIAN_POINT('Ctrl Pts',(-3.35890824422976,1.,-1.92572846125763));
#46113=CARTESIAN_POINT('Ctrl Pts',(-3.36615168657597,1.,-1.92778626543803));
#46114=CARTESIAN_POINT('Ctrl Pts',(-3.37336807068078,1.,-1.92975993109897));
#46115=CARTESIAN_POINT('Ctrl Pts',(-3.38056768525577,1.,-1.93165739093292));
#46116=CARTESIAN_POINT('Ctrl Pts',(-3.38777076883267,1.,-1.93349233176794));
#46117=CARTESIAN_POINT('Ctrl Pts',(-3.39499923640789,1.,-1.93527929945982));
#46118=CARTESIAN_POINT('Ctrl Pts',(-3.40226802104093,1.,-1.93702857723089));
#46119=CARTESIAN_POINT('Ctrl Pts',(-3.40957978266622,1.,-1.93874306008132));
#46120=CARTESIAN_POINT('Ctrl Pts',(-3.41692971994082,1.,-1.94042111965237));
#46121=CARTESIAN_POINT('Ctrl Pts',(-3.42430850941497,1.,-1.94205835913692));
#46122=CARTESIAN_POINT('Ctrl Pts',(-3.43170586602436,1.,-1.94364973660285));
#46123=CARTESIAN_POINT('Ctrl Pts',(-3.43911410197693,1.,-1.94519168842883));
#46124=CARTESIAN_POINT('Ctrl Pts',(-3.44653088665685,1.,-1.94668377715332));
#46125=CARTESIAN_POINT('Ctrl Pts',(-3.45395731584051,1.,-1.94812754766524));
#46126=CARTESIAN_POINT('Ctrl Pts',(-3.46139661060959,1.,-1.94952575850196));
#46127=CARTESIAN_POINT('Ctrl Pts',(-3.4688525897419,1.,-1.95088147859876));
#46128=CARTESIAN_POINT('Ctrl Pts',(-3.47632820495926,1.,-1.95219722189878));
#46129=CARTESIAN_POINT('Ctrl Pts',(-3.48382414832648,1.,-1.95347412486316));
#46130=CARTESIAN_POINT('Ctrl Pts',(-3.49133956289154,1.,-1.95471236969653));
#46131=CARTESIAN_POINT('Ctrl Pts',(-3.49887263575602,1.,-1.9559115382367));
#46132=CARTESIAN_POINT('Ctrl Pts',(-3.50642124159913,1.,-1.95707099606513));
#46133=CARTESIAN_POINT('Ctrl Pts',(-3.51398354617772,1.,-1.95819025316768));
#46134=CARTESIAN_POINT('Ctrl Pts',(-3.52155867431438,1.,-1.95926936324436));
#46135=CARTESIAN_POINT('Ctrl Pts',(-3.52914648844289,1.,-1.96030879411534));
#46136=CARTESIAN_POINT('Ctrl Pts',(-3.53674730625759,1.,-1.96130926212661));
#46137=CARTESIAN_POINT('Ctrl Pts',(-3.54436163300425,1.,-1.96227157573058));
#46138=CARTESIAN_POINT('Ctrl Pts',(-3.55198990600929,1.,-1.96319648628667));
#46139=CARTESIAN_POINT('Ctrl Pts',(-3.55963218706201,1.,-1.96408450906868));
#46140=CARTESIAN_POINT('Ctrl Pts',(-3.56728820357933,1.,-1.96493594634643));
#46141=CARTESIAN_POINT('Ctrl Pts',(-3.57495748601088,1.,-1.96575096652857));
#46142=CARTESIAN_POINT('Ctrl Pts',(-3.58263947663884,1.,-1.9665296668894));
#46143=CARTESIAN_POINT('Ctrl Pts',(-3.5903336402273,1.,-1.96727213799507));
#46144=CARTESIAN_POINT('Ctrl Pts',(-3.59803959819725,1.,-1.96797854118257));
#46145=CARTESIAN_POINT('Ctrl Pts',(-3.60575714017676,1.,-1.96864911885775));
#46146=CARTESIAN_POINT('Ctrl Pts',(-3.61348615496393,1.,-1.96928416040712));
#46147=CARTESIAN_POINT('Ctrl Pts',(-3.62122658401722,1.,-1.96988398129888));
#46148=CARTESIAN_POINT('Ctrl Pts',(-3.62897836973397,1.,-1.97044889850518));
#46149=CARTESIAN_POINT('Ctrl Pts',(-3.63674139590853,1.,-1.97097920454698));
#46150=CARTESIAN_POINT('Ctrl Pts',(-3.64451546724221,1.,-1.97147515441539));
#46151=CARTESIAN_POINT('Ctrl Pts',(-3.65230034717364,1.,-1.97193697240645));
#46152=CARTESIAN_POINT('Ctrl Pts',(-3.66009578166865,1.,-1.97236485439317));
#46153=CARTESIAN_POINT('Ctrl Pts',(-3.66790152751984,1.,-1.9727589719863));
#46154=CARTESIAN_POINT('Ctrl Pts',(-3.67571738106175,1.,-1.97311947678035));
#46155=CARTESIAN_POINT('Ctrl Pts',(-3.68354319913416,1.,-1.9734465030363));
#46156=CARTESIAN_POINT('Ctrl Pts',(-3.69137888597855,1.,-1.97374016224397));
#46157=CARTESIAN_POINT('Ctrl Pts',(-3.69765528558292,1.,-1.97394846382288));
#46158=CARTESIAN_POINT('Ctrl Pts',(-3.70236698911837,1.,-1.97408973726149));
#46159=CARTESIAN_POINT('Ctrl Pts',(-3.7055100813194,1.,-1.974177276451));
#46160=CARTESIAN_POINT('Ctrl Pts',(-3.70708211654725,1.,-1.97421938526992));
#46161=CARTESIAN_POINT('Origin',(-3.70708211654725,0.,-1.97421938526992));
#46162=CARTESIAN_POINT('',(-3.77614523045147,1.,-1.83867539237861));
#46163=CARTESIAN_POINT('Origin',(0.,0.,0.));
#46164=CARTESIAN_POINT('',(-3.14877060440425,1.,-2.03660101169564));
#46165=CARTESIAN_POINT('Origin',(0.,1.,0.));
#46166=CARTESIAN_POINT('Ctrl Pts',(-3.14877060440425,1.,-2.03660101169564));
#46167=CARTESIAN_POINT('Ctrl Pts',(-3.14877060440425,0.666666666666667,
-2.03660101169564));
#46168=CARTESIAN_POINT('Ctrl Pts',(-3.14877060440425,0.333333333333333,
-2.03660101169564));
#46169=CARTESIAN_POINT('Ctrl Pts',(-3.14877060440425,-0.333333333333333,
-2.03660101169564));
#46170=CARTESIAN_POINT('Ctrl Pts',(-3.14877060440425,-0.666666666666667,
-2.03660101169564));
#46171=CARTESIAN_POINT('Ctrl Pts',(-3.14877060440425,-1.,-2.03660101169564));
#46172=CARTESIAN_POINT('Ctrl Pts',(-3.44202241512147,-1.,-2.40675750623143));
#46173=CARTESIAN_POINT('Ctrl Pts',(-3.44202241512147,1.,-2.40675750623143));
#46174=CARTESIAN_POINT('Ctrl Pts',(-3.44127120683402,-1.,-2.40537592959345));
#46175=CARTESIAN_POINT('Ctrl Pts',(-3.44127120683402,1.,-2.40537592959345));
#46176=CARTESIAN_POINT('Ctrl Pts',(-3.43976627485223,-1.,-2.40261515590099));
#46177=CARTESIAN_POINT('Ctrl Pts',(-3.43976627485223,1.,-2.40261515590099));
#46178=CARTESIAN_POINT('Ctrl Pts',(-3.43750133066036,-1.,-2.39848113411429));
#46179=CARTESIAN_POINT('Ctrl Pts',(-3.43750133066036,1.,-2.39848113411429));
#46180=CARTESIAN_POINT('Ctrl Pts',(-3.43446630680436,-1.,-2.39298338805823));
#46181=CARTESIAN_POINT('Ctrl Pts',(-3.43446630680436,1.,-2.39298338805823));
#46182=CARTESIAN_POINT('Ctrl Pts',(-3.43064732714472,-1.,-2.38613505844641));
#46183=CARTESIAN_POINT('Ctrl Pts',(-3.43064732714472,1.,-2.38613505844641));
#46184=CARTESIAN_POINT('Ctrl Pts',(-3.42680309755241,-1.,-2.37931067029517));
#46185=CARTESIAN_POINT('Ctrl Pts',(-3.42680309755241,1.,-2.37931067029517));
#46186=CARTESIAN_POINT('Ctrl Pts',(-3.42293356216595,-1.,-2.37251035954351));
#46187=CARTESIAN_POINT('Ctrl Pts',(-3.42293356216595,1.,-2.37251035954351));
#46188=CARTESIAN_POINT('Ctrl Pts',(-3.41903866635384,-1.,-2.36573431470314));
#46189=CARTESIAN_POINT('Ctrl Pts',(-3.41903866635384,1.,-2.36573431470314));
#46190=CARTESIAN_POINT('Ctrl Pts',(-3.4151183675076,-1.,-2.35898278606449));
#46191=CARTESIAN_POINT('Ctrl Pts',(-3.4151183675076,1.,-2.35898278606449));
#46192=CARTESIAN_POINT('Ctrl Pts',(-3.41117262313464,-1.,-2.35225606823649));
#46193=CARTESIAN_POINT('Ctrl Pts',(-3.41117262313464,1.,-2.35225606823649));
#46194=CARTESIAN_POINT('Ctrl Pts',(-3.40720137403888,-1.,-2.34555447648901));
#46195=CARTESIAN_POINT('Ctrl Pts',(-3.40720137403888,1.,-2.34555447648901));
#46196=CARTESIAN_POINT('Ctrl Pts',(-3.40320452776646,-1.,-2.33887832342715));
#46197=CARTESIAN_POINT('Ctrl Pts',(-3.40320452776646,1.,-2.33887832342715));
#46198=CARTESIAN_POINT('Ctrl Pts',(-3.39918194578115,-1.,-2.33222789882601));
#46199=CARTESIAN_POINT('Ctrl Pts',(-3.39918194578115,1.,-2.33222789882601));
#46200=CARTESIAN_POINT('Ctrl Pts',(-3.39513342020045,-1.,-2.32560343902683));
#46201=CARTESIAN_POINT('Ctrl Pts',(-3.39513342020045,1.,-2.32560343902683));
#46202=CARTESIAN_POINT('Ctrl Pts',(-3.39105869475112,-1.,-2.31900513925627));
#46203=CARTESIAN_POINT('Ctrl Pts',(-3.39105869475112,1.,-2.31900513925627));
#46204=CARTESIAN_POINT('Ctrl Pts',(-3.38695751492659,-1.,-2.31243319489505));
#46205=CARTESIAN_POINT('Ctrl Pts',(-3.38695751492659,1.,-2.31243319489505));
#46206=CARTESIAN_POINT('Ctrl Pts',(-3.38282967336676,-1.,-2.30588783640389));
#46207=CARTESIAN_POINT('Ctrl Pts',(-3.38282967336676,1.,-2.30588783640389));
#46208=CARTESIAN_POINT('Ctrl Pts',(-3.37867504959382,-1.,-2.29936936127588));
#46209=CARTESIAN_POINT('Ctrl Pts',(-3.37867504959382,1.,-2.29936936127588));
#46210=CARTESIAN_POINT('Ctrl Pts',(-3.37449367172707,-1.,-2.2928781800731));
#46211=CARTESIAN_POINT('Ctrl Pts',(-3.37449367172707,1.,-2.2928781800731));
#46212=CARTESIAN_POINT('Ctrl Pts',(-3.37028570206357,-1.,-2.28641481081045));
#46213=CARTESIAN_POINT('Ctrl Pts',(-3.37028570206357,1.,-2.28641481081045));
#46214=CARTESIAN_POINT('Ctrl Pts',(-3.36605130712978,-1.,-2.27997979457968));
#46215=CARTESIAN_POINT('Ctrl Pts',(-3.36605130712978,1.,-2.27997979457968));
#46216=CARTESIAN_POINT('Ctrl Pts',(-3.36179055004369,-1.,-2.27357362620902));
#46217=CARTESIAN_POINT('Ctrl Pts',(-3.36179055004369,1.,-2.27357362620902));
#46218=CARTESIAN_POINT('Ctrl Pts',(-3.35750328523077,-1.,-2.26719668579921));
#46219=CARTESIAN_POINT('Ctrl Pts',(-3.35750328523077,1.,-2.26719668579921));
#46220=CARTESIAN_POINT('Ctrl Pts',(-3.35318902552676,-1.,-2.26084915222484));
#46221=CARTESIAN_POINT('Ctrl Pts',(-3.35318902552676,1.,-2.26084915222484));
#46222=CARTESIAN_POINT('Ctrl Pts',(-3.34884690292342,-1.,-2.25453097693524));
#46223=CARTESIAN_POINT('Ctrl Pts',(-3.34884690292342,1.,-2.25453097693524));
#46224=CARTESIAN_POINT('Ctrl Pts',(-3.34447596770768,-1.,-2.24824207678288));
#46225=CARTESIAN_POINT('Ctrl Pts',(-3.34447596770768,1.,-2.24824207678288));
#46226=CARTESIAN_POINT('Ctrl Pts',(-3.34007543738044,-1.,-2.24198249391437));
#46227=CARTESIAN_POINT('Ctrl Pts',(-3.34007543738044,1.,-2.24198249391437));
#46228=CARTESIAN_POINT('Ctrl Pts',(-3.33564495756478,-1.,-2.2357525632881));
#46229=CARTESIAN_POINT('Ctrl Pts',(-3.33564495756478,1.,-2.2357525632881));
#46230=CARTESIAN_POINT('Ctrl Pts',(-3.33118487773593,-1.,-2.22955308907221));
#46231=CARTESIAN_POINT('Ctrl Pts',(-3.33118487773593,1.,-2.22955308907221));
#46232=CARTESIAN_POINT('Ctrl Pts',(-3.32669646722871,-1.,-2.22338548312758));
#46233=CARTESIAN_POINT('Ctrl Pts',(-3.32669646722871,1.,-2.22338548312758));
#46234=CARTESIAN_POINT('Ctrl Pts',(-3.32218125618955,-1.,-2.21725135110889));
#46235=CARTESIAN_POINT('Ctrl Pts',(-3.32218125618955,1.,-2.21725135110889));
#46236=CARTESIAN_POINT('Ctrl Pts',(-3.31764044024231,-1.,-2.21115211847872));
#46237=CARTESIAN_POINT('Ctrl Pts',(-3.31764044024231,1.,-2.21115211847872));
#46238=CARTESIAN_POINT('Ctrl Pts',(-3.3130742460895,-1.,-2.20508863150608));
#46239=CARTESIAN_POINT('Ctrl Pts',(-3.3130742460895,1.,-2.20508863150608));
#46240=CARTESIAN_POINT('Ctrl Pts',(-3.30848134694596,-1.,-2.19906078949924));
#46241=CARTESIAN_POINT('Ctrl Pts',(-3.30848134694596,1.,-2.19906078949924));
#46242=CARTESIAN_POINT('Ctrl Pts',(-3.30385816281831,-1.,-2.19306710376112));
#46243=CARTESIAN_POINT('Ctrl Pts',(-3.30385816281831,1.,-2.19306710376112));
#46244=CARTESIAN_POINT('Ctrl Pts',(-3.29920022557635,-1.,-2.18710556500325));
#46245=CARTESIAN_POINT('Ctrl Pts',(-3.29920022557635,1.,-2.18710556500325));
#46246=CARTESIAN_POINT('Ctrl Pts',(-3.29450361500484,-1.,-2.18117455557062));
#46247=CARTESIAN_POINT('Ctrl Pts',(-3.29450361500484,1.,-2.18117455557062));
#46248=CARTESIAN_POINT('Ctrl Pts',(-3.28976645712566,-1.,-2.17527380048422));
#46249=CARTESIAN_POINT('Ctrl Pts',(-3.28976645712566,1.,-2.17527380048422));
#46250=CARTESIAN_POINT('Ctrl Pts',(-3.2849901997973,-1.,-2.16940517773459));
#46251=CARTESIAN_POINT('Ctrl Pts',(-3.2849901997973,1.,-2.16940517773459));
#46252=CARTESIAN_POINT('Ctrl Pts',(-3.28018150841414,-1.,-2.16357391934434));
#46253=CARTESIAN_POINT('Ctrl Pts',(-3.28018150841414,1.,-2.16357391934434));
#46254=CARTESIAN_POINT('Ctrl Pts',(-3.27534954469206,-1.,-2.15778690038359));
#46255=CARTESIAN_POINT('Ctrl Pts',(-3.27534954469206,1.,-2.15778690038359));
#46256=CARTESIAN_POINT('Ctrl Pts',(-3.27050245897244,-1.,-2.15205043199818));
#46257=CARTESIAN_POINT('Ctrl Pts',(-3.27050245897244,1.,-2.15205043199818));
#46258=CARTESIAN_POINT('Ctrl Pts',(-3.26564388189764,-1.,-2.14636805295663));
#46259=CARTESIAN_POINT('Ctrl Pts',(-3.26564388189764,1.,-2.14636805295663));
#46260=CARTESIAN_POINT('Ctrl Pts',(-3.26077002641868,-1.,-2.14073870754257));
#46261=CARTESIAN_POINT('Ctrl Pts',(-3.26077002641868,1.,-2.14073870754257));
#46262=CARTESIAN_POINT('Ctrl Pts',(-3.25586495065027,-1.,-2.13515375878786));
#46263=CARTESIAN_POINT('Ctrl Pts',(-3.25586495065027,1.,-2.13515375878786));
#46264=CARTESIAN_POINT('Ctrl Pts',(-3.25090574493994,-1.,-2.1296002839681));
#46265=CARTESIAN_POINT('Ctrl Pts',(-3.25090574493994,1.,-2.1296002839681));
#46266=CARTESIAN_POINT('Ctrl Pts',(-3.24587102613347,-1.,-2.12406646410943));
#46267=CARTESIAN_POINT('Ctrl Pts',(-3.24587102613347,1.,-2.12406646410943));
#46268=CARTESIAN_POINT('Ctrl Pts',(-3.24074905517282,-1.,-2.11854673326972));
#46269=CARTESIAN_POINT('Ctrl Pts',(-3.24074905517282,1.,-2.11854673326972));
#46270=CARTESIAN_POINT('Ctrl Pts',(-3.23554444767115,-1.,-2.11304604021784));
#46271=CARTESIAN_POINT('Ctrl Pts',(-3.23554444767115,1.,-2.11304604021784));
#46272=CARTESIAN_POINT('Ctrl Pts',(-3.23028945793334,-1.,-2.1075869964248));
#46273=CARTESIAN_POINT('Ctrl Pts',(-3.23028945793334,1.,-2.1075869964248));
#46274=CARTESIAN_POINT('Ctrl Pts',(-3.22503437553496,-1.,-2.10220384298533));
#46275=CARTESIAN_POINT('Ctrl Pts',(-3.22503437553496,1.,-2.10220384298533));
#46276=CARTESIAN_POINT('Ctrl Pts',(-3.21982707347067,-1.,-2.09692958434933));
#46277=CARTESIAN_POINT('Ctrl Pts',(-3.21982707347067,1.,-2.09692958434933));
#46278=CARTESIAN_POINT('Ctrl Pts',(-3.2146942960168,-1.,-2.0917841946046));
#46279=CARTESIAN_POINT('Ctrl Pts',(-3.2146942960168,1.,-2.0917841946046));
#46280=CARTESIAN_POINT('Ctrl Pts',(-3.20962575845433,-1.,-2.08676465517435));
#46281=CARTESIAN_POINT('Ctrl Pts',(-3.20962575845433,1.,-2.08676465517435));
#46282=CARTESIAN_POINT('Ctrl Pts',(-3.20454818630635,-1.,-2.08182850370816));
#46283=CARTESIAN_POINT('Ctrl Pts',(-3.20454818630635,1.,-2.08182850370816));
#46284=CARTESIAN_POINT('Ctrl Pts',(-3.19934132835879,-1.,-2.0769044187063));
#46285=CARTESIAN_POINT('Ctrl Pts',(-3.19934132835879,1.,-2.0769044187063));
#46286=CARTESIAN_POINT('Ctrl Pts',(-3.19388465568113,-1.,-2.07192253497765));
#46287=CARTESIAN_POINT('Ctrl Pts',(-3.19388465568113,1.,-2.07192253497765));
#46288=CARTESIAN_POINT('Ctrl Pts',(-3.18809755562297,-1.,-2.06684062744065));
#46289=CARTESIAN_POINT('Ctrl Pts',(-3.18809755562297,1.,-2.06684062744065));
#46290=CARTESIAN_POINT('Ctrl Pts',(-3.18197692964677,-1.,-2.06166849827143));
#46291=CARTESIAN_POINT('Ctrl Pts',(-3.18197692964677,1.,-2.06166849827143));
#46292=CARTESIAN_POINT('Ctrl Pts',(-3.17564906975592,-1.,-2.05650186773279));
#46293=CARTESIAN_POINT('Ctrl Pts',(-3.17564906975592,1.,-2.05650186773279));
#46294=CARTESIAN_POINT('Ctrl Pts',(-3.16936341689859,-1.,-2.05151770247452));
#46295=CARTESIAN_POINT('Ctrl Pts',(-3.16936341689859,1.,-2.05151770247452));
#46296=CARTESIAN_POINT('Ctrl Pts',(-3.16343165059235,-1.,-2.0469333124766));
#46297=CARTESIAN_POINT('Ctrl Pts',(-3.16343165059235,1.,-2.0469333124766));
#46298=CARTESIAN_POINT('Ctrl Pts',(-3.15817983946525,-1.,-2.04297406404132));
#46299=CARTESIAN_POINT('Ctrl Pts',(-3.15817983946525,1.,-2.04297406404132));
#46300=CARTESIAN_POINT('Ctrl Pts',(-3.1538999167466,-1.,-2.03984073791432));
#46301=CARTESIAN_POINT('Ctrl Pts',(-3.1538999167466,1.,-2.03984073791432));
#46302=CARTESIAN_POINT('Ctrl Pts',(-3.15079010635326,-1.,-2.03766932526171));
#46303=CARTESIAN_POINT('Ctrl Pts',(-3.15079010635326,1.,-2.03766932526171));
#46304=CARTESIAN_POINT('Ctrl Pts',(-3.14931281967585,-1.,-2.03675273048882));
#46305=CARTESIAN_POINT('Ctrl Pts',(-3.14931281967585,1.,-2.03675273048882));
#46306=CARTESIAN_POINT('Ctrl Pts',(-3.14878756590499,-1.,-2.03653654935384));
#46307=CARTESIAN_POINT('Ctrl Pts',(-3.14878756590499,1.,-2.03653654935384));
#46308=CARTESIAN_POINT('Ctrl Pts',(-3.14869618937138,-1.,-2.036601737578));
#46309=CARTESIAN_POINT('Ctrl Pts',(-3.14869618937138,1.,-2.036601737578));
#46310=CARTESIAN_POINT('Ctrl Pts',(-3.1487152044751,-1.,-2.03668666247593));
#46311=CARTESIAN_POINT('Ctrl Pts',(-3.1487152044751,1.,-2.03668666247593));
#46312=CARTESIAN_POINT('',(-3.44202241512147,1.,-2.40675750623143));
#46313=CARTESIAN_POINT('Ctrl Pts',(-3.44202241512147,1.,-2.40675750623143));
#46314=CARTESIAN_POINT('Ctrl Pts',(-3.44127120683402,1.,-2.40537592959345));
#46315=CARTESIAN_POINT('Ctrl Pts',(-3.43976627485223,1.,-2.40261515590099));
#46316=CARTESIAN_POINT('Ctrl Pts',(-3.43750133066036,1.,-2.39848113411429));
#46317=CARTESIAN_POINT('Ctrl Pts',(-3.43446630680436,1.,-2.39298338805823));
#46318=CARTESIAN_POINT('Ctrl Pts',(-3.43064732714472,1.,-2.38613505844641));
#46319=CARTESIAN_POINT('Ctrl Pts',(-3.42680309755241,1.,-2.37931067029517));
#46320=CARTESIAN_POINT('Ctrl Pts',(-3.42293356216595,1.,-2.37251035954351));
#46321=CARTESIAN_POINT('Ctrl Pts',(-3.41903866635384,1.,-2.36573431470314));
#46322=CARTESIAN_POINT('Ctrl Pts',(-3.4151183675076,1.,-2.35898278606449));
#46323=CARTESIAN_POINT('Ctrl Pts',(-3.41117262313464,1.,-2.35225606823649));
#46324=CARTESIAN_POINT('Ctrl Pts',(-3.40720137403888,1.,-2.34555447648901));
#46325=CARTESIAN_POINT('Ctrl Pts',(-3.40320452776646,1.,-2.33887832342715));
#46326=CARTESIAN_POINT('Ctrl Pts',(-3.39918194578115,1.,-2.33222789882601));
#46327=CARTESIAN_POINT('Ctrl Pts',(-3.39513342020045,1.,-2.32560343902683));
#46328=CARTESIAN_POINT('Ctrl Pts',(-3.39105869475112,1.,-2.31900513925627));
#46329=CARTESIAN_POINT('Ctrl Pts',(-3.38695751492659,1.,-2.31243319489505));
#46330=CARTESIAN_POINT('Ctrl Pts',(-3.38282967336676,1.,-2.30588783640389));
#46331=CARTESIAN_POINT('Ctrl Pts',(-3.37867504959382,1.,-2.29936936127588));
#46332=CARTESIAN_POINT('Ctrl Pts',(-3.37449367172707,1.,-2.2928781800731));
#46333=CARTESIAN_POINT('Ctrl Pts',(-3.37028570206357,1.,-2.28641481081045));
#46334=CARTESIAN_POINT('Ctrl Pts',(-3.36605130712978,1.,-2.27997979457968));
#46335=CARTESIAN_POINT('Ctrl Pts',(-3.36179055004369,1.,-2.27357362620902));
#46336=CARTESIAN_POINT('Ctrl Pts',(-3.35750328523077,1.,-2.26719668579921));
#46337=CARTESIAN_POINT('Ctrl Pts',(-3.35318902552676,1.,-2.26084915222484));
#46338=CARTESIAN_POINT('Ctrl Pts',(-3.34884690292342,1.,-2.25453097693524));
#46339=CARTESIAN_POINT('Ctrl Pts',(-3.34447596770768,1.,-2.24824207678288));
#46340=CARTESIAN_POINT('Ctrl Pts',(-3.34007543738044,1.,-2.24198249391437));
#46341=CARTESIAN_POINT('Ctrl Pts',(-3.33564495756478,1.,-2.2357525632881));
#46342=CARTESIAN_POINT('Ctrl Pts',(-3.33118487773593,1.,-2.22955308907221));
#46343=CARTESIAN_POINT('Ctrl Pts',(-3.32669646722871,1.,-2.22338548312758));
#46344=CARTESIAN_POINT('Ctrl Pts',(-3.32218125618955,1.,-2.21725135110889));
#46345=CARTESIAN_POINT('Ctrl Pts',(-3.31764044024231,1.,-2.21115211847872));
#46346=CARTESIAN_POINT('Ctrl Pts',(-3.3130742460895,1.,-2.20508863150608));
#46347=CARTESIAN_POINT('Ctrl Pts',(-3.30848134694596,1.,-2.19906078949924));
#46348=CARTESIAN_POINT('Ctrl Pts',(-3.30385816281831,1.,-2.19306710376112));
#46349=CARTESIAN_POINT('Ctrl Pts',(-3.29920022557635,1.,-2.18710556500325));
#46350=CARTESIAN_POINT('Ctrl Pts',(-3.29450361500484,1.,-2.18117455557062));
#46351=CARTESIAN_POINT('Ctrl Pts',(-3.28976645712566,1.,-2.17527380048422));
#46352=CARTESIAN_POINT('Ctrl Pts',(-3.2849901997973,1.,-2.16940517773459));
#46353=CARTESIAN_POINT('Ctrl Pts',(-3.28018150841414,1.,-2.16357391934434));
#46354=CARTESIAN_POINT('Ctrl Pts',(-3.27534954469206,1.,-2.15778690038359));
#46355=CARTESIAN_POINT('Ctrl Pts',(-3.27050245897244,1.,-2.15205043199818));
#46356=CARTESIAN_POINT('Ctrl Pts',(-3.26564388189764,1.,-2.14636805295663));
#46357=CARTESIAN_POINT('Ctrl Pts',(-3.26077002641868,1.,-2.14073870754257));
#46358=CARTESIAN_POINT('Ctrl Pts',(-3.25586495065027,1.,-2.13515375878786));
#46359=CARTESIAN_POINT('Ctrl Pts',(-3.25090574493994,1.,-2.1296002839681));
#46360=CARTESIAN_POINT('Ctrl Pts',(-3.24587102613347,1.,-2.12406646410943));
#46361=CARTESIAN_POINT('Ctrl Pts',(-3.24074905517282,1.,-2.11854673326972));
#46362=CARTESIAN_POINT('Ctrl Pts',(-3.23554444767115,1.,-2.11304604021784));
#46363=CARTESIAN_POINT('Ctrl Pts',(-3.23028945793334,1.,-2.1075869964248));
#46364=CARTESIAN_POINT('Ctrl Pts',(-3.22503437553496,1.,-2.10220384298533));
#46365=CARTESIAN_POINT('Ctrl Pts',(-3.21982707347067,1.,-2.09692958434933));
#46366=CARTESIAN_POINT('Ctrl Pts',(-3.2146942960168,1.,-2.0917841946046));
#46367=CARTESIAN_POINT('Ctrl Pts',(-3.20962575845433,1.,-2.08676465517435));
#46368=CARTESIAN_POINT('Ctrl Pts',(-3.20454818630635,1.,-2.08182850370816));
#46369=CARTESIAN_POINT('Ctrl Pts',(-3.19934132835879,1.,-2.0769044187063));
#46370=CARTESIAN_POINT('Ctrl Pts',(-3.19388465568113,1.,-2.07192253497765));
#46371=CARTESIAN_POINT('Ctrl Pts',(-3.18809755562297,1.,-2.06684062744065));
#46372=CARTESIAN_POINT('Ctrl Pts',(-3.18197692964677,1.,-2.06166849827143));
#46373=CARTESIAN_POINT('Ctrl Pts',(-3.17564906975592,1.,-2.05650186773279));
#46374=CARTESIAN_POINT('Ctrl Pts',(-3.16936341689859,1.,-2.05151770247452));
#46375=CARTESIAN_POINT('Ctrl Pts',(-3.16343165059235,1.,-2.0469333124766));
#46376=CARTESIAN_POINT('Ctrl Pts',(-3.15817983946525,1.,-2.04297406404132));
#46377=CARTESIAN_POINT('Ctrl Pts',(-3.1538999167466,1.,-2.03984073791432));
#46378=CARTESIAN_POINT('Ctrl Pts',(-3.15102344775396,1.,-2.03783225496023));
#46379=CARTESIAN_POINT('Ctrl Pts',(-3.14959882629936,1.,-2.03693188810614));
#46380=CARTESIAN_POINT('Ctrl Pts',(-3.14901193669147,1.,-2.03663974554941));
#46381=CARTESIAN_POINT('Ctrl Pts',(-3.1488193908823,1.,-2.03659701539175));
#46382=CARTESIAN_POINT('Ctrl Pts',(-3.14877060440425,1.,-2.03660101169564));
#46383=CARTESIAN_POINT('',(-3.44202241512147,0.,-2.40675750623143));
#46384=CARTESIAN_POINT('Ctrl Pts',(-2.91001063062876,-1.,-2.36523532225181));
#46385=CARTESIAN_POINT('Ctrl Pts',(-2.91001063062876,1.,-2.36523532225181));
#46386=CARTESIAN_POINT('Ctrl Pts',(-2.90992398626211,-1.,-2.36524348105112));
#46387=CARTESIAN_POINT('Ctrl Pts',(-2.90992398626211,1.,-2.36524348105112));
#46388=CARTESIAN_POINT('Ctrl Pts',(-2.90989022548032,-1.,-2.36535052956938));
#46389=CARTESIAN_POINT('Ctrl Pts',(-2.90989022548032,1.,-2.36535052956938));
#46390=CARTESIAN_POINT('Ctrl Pts',(-2.91025813830041,-1.,-2.36578327194741));
#46391=CARTESIAN_POINT('Ctrl Pts',(-2.91025813830041,1.,-2.36578327194741));
#46392=CARTESIAN_POINT('Ctrl Pts',(-2.9115863784204,-1.,-2.36690501170627));
#46393=CARTESIAN_POINT('Ctrl Pts',(-2.9115863784204,1.,-2.36690501170627));
#46394=CARTESIAN_POINT('Ctrl Pts',(-2.9146124988314,-1.,-2.36919161373173));
#46395=CARTESIAN_POINT('Ctrl Pts',(-2.9146124988314,1.,-2.36919161373173));
#46396=CARTESIAN_POINT('Ctrl Pts',(-2.91891503791411,-1.,-2.37229381109821));
#46397=CARTESIAN_POINT('Ctrl Pts',(-2.91891503791411,1.,-2.37229381109821));
#46398=CARTESIAN_POINT('Ctrl Pts',(-2.92430340582608,-1.,-2.3760651052403));
#46399=CARTESIAN_POINT('Ctrl Pts',(-2.92430340582608,1.,-2.3760651052403));
#46400=CARTESIAN_POINT('Ctrl Pts',(-2.93049643640206,-1.,-2.38028989582073));
#46401=CARTESIAN_POINT('Ctrl Pts',(-2.93049643640206,1.,-2.38028989582073));
#46402=CARTESIAN_POINT('Ctrl Pts',(-2.93717903280391,-1.,-2.38472771516311));
#46403=CARTESIAN_POINT('Ctrl Pts',(-2.93717903280391,1.,-2.38472771516311));
#46404=CARTESIAN_POINT('Ctrl Pts',(-2.94404820669076,-1.,-2.38914929090759));
#46405=CARTESIAN_POINT('Ctrl Pts',(-2.94404820669076,1.,-2.38914929090759));
#46406=CARTESIAN_POINT('Ctrl Pts',(-2.95085857128439,-1.,-2.39337207631667));
#46407=CARTESIAN_POINT('Ctrl Pts',(-2.95085857128439,1.,-2.39337207631667));
#46408=CARTESIAN_POINT('Ctrl Pts',(-2.95748006482942,-1.,-2.39730553974517));
#46409=CARTESIAN_POINT('Ctrl Pts',(-2.95748006482942,1.,-2.39730553974517));
#46410=CARTESIAN_POINT('Ctrl Pts',(-2.96390432240312,-1.,-2.4009556571164));
#46411=CARTESIAN_POINT('Ctrl Pts',(-2.96390432240312,1.,-2.4009556571164));
#46412=CARTESIAN_POINT('Ctrl Pts',(-2.9701964131236,-1.,-2.40438604734919));
#46413=CARTESIAN_POINT('Ctrl Pts',(-2.9701964131236,1.,-2.40438604734919));
#46414=CARTESIAN_POINT('Ctrl Pts',(-2.97646002822422,-1.,-2.40768975073713));
#46415=CARTESIAN_POINT('Ctrl Pts',(-2.97646002822422,1.,-2.40768975073713));
#46416=CARTESIAN_POINT('Ctrl Pts',(-2.98280015815107,-1.,-2.41095909342571));
#46417=CARTESIAN_POINT('Ctrl Pts',(-2.98280015815107,1.,-2.41095909342571));
#46418=CARTESIAN_POINT('Ctrl Pts',(-2.98927983005796,-1.,-2.41425064199586));
#46419=CARTESIAN_POINT('Ctrl Pts',(-2.98927983005796,1.,-2.41425064199586));
#46420=CARTESIAN_POINT('Ctrl Pts',(-2.99590509293503,-1.,-2.41757324500514));
#46421=CARTESIAN_POINT('Ctrl Pts',(-2.99590509293503,1.,-2.41757324500514));
#46422=CARTESIAN_POINT('Ctrl Pts',(-3.00264868585996,-1.,-2.42090763946779));
#46423=CARTESIAN_POINT('Ctrl Pts',(-3.00264868585996,1.,-2.42090763946779));
#46424=CARTESIAN_POINT('Ctrl Pts',(-3.00946442616658,-1.,-2.42421849439613));
#46425=CARTESIAN_POINT('Ctrl Pts',(-3.00946442616658,1.,-2.42421849439613));
#46426=CARTESIAN_POINT('Ctrl Pts',(-3.01630420830504,-1.,-2.42746856264168));
#46427=CARTESIAN_POINT('Ctrl Pts',(-3.01630420830504,1.,-2.42746856264168));
#46428=CARTESIAN_POINT('Ctrl Pts',(-3.02313656036004,-1.,-2.43063415586637));
#46429=CARTESIAN_POINT('Ctrl Pts',(-3.02313656036004,1.,-2.43063415586637));
#46430=CARTESIAN_POINT('Ctrl Pts',(-3.02995534946978,-1.,-2.43371241361488));
#46431=CARTESIAN_POINT('Ctrl Pts',(-3.02995534946978,1.,-2.43371241361488));
#46432=CARTESIAN_POINT('Ctrl Pts',(-3.03676949672821,-1.,-2.43671278042414));
#46433=CARTESIAN_POINT('Ctrl Pts',(-3.03676949672821,1.,-2.43671278042414));
#46434=CARTESIAN_POINT('Ctrl Pts',(-3.04359685040555,-1.,-2.43965194061857));
#46435=CARTESIAN_POINT('Ctrl Pts',(-3.04359685040555,1.,-2.43965194061857));
#46436=CARTESIAN_POINT('Ctrl Pts',(-3.05045678021504,-1.,-2.44254768923105));
#46437=CARTESIAN_POINT('Ctrl Pts',(-3.05045678021504,1.,-2.44254768923105));
#46438=CARTESIAN_POINT('Ctrl Pts',(-3.05736242671506,-1.,-2.44541251892556));
#46439=CARTESIAN_POINT('Ctrl Pts',(-3.05736242671506,1.,-2.44541251892556));
#46440=CARTESIAN_POINT('Ctrl Pts',(-3.06431596421405,-1.,-2.44824970516544));
#46441=CARTESIAN_POINT('Ctrl Pts',(-3.06431596421405,1.,-2.44824970516544));
#46442=CARTESIAN_POINT('Ctrl Pts',(-3.07131290521297,-1.,-2.45105688854422));
#46443=CARTESIAN_POINT('Ctrl Pts',(-3.07131290521297,1.,-2.45105688854422));
#46444=CARTESIAN_POINT('Ctrl Pts',(-3.07834472886139,-1.,-2.4538282678779));
#46445=CARTESIAN_POINT('Ctrl Pts',(-3.07834472886139,1.,-2.4538282678779));
#46446=CARTESIAN_POINT('Ctrl Pts',(-3.08540206545315,-1.,-2.45655725437039));
#46447=CARTESIAN_POINT('Ctrl Pts',(-3.08540206545315,1.,-2.45655725437039));
#46448=CARTESIAN_POINT('Ctrl Pts',(-3.09247787931887,-1.,-2.4592391256388));
#46449=CARTESIAN_POINT('Ctrl Pts',(-3.09247787931887,1.,-2.4592391256388));
#46450=CARTESIAN_POINT('Ctrl Pts',(-3.09956993697052,-1.,-2.46187308501884));
#46451=CARTESIAN_POINT('Ctrl Pts',(-3.09956993697052,1.,-2.46187308501884));
#46452=CARTESIAN_POINT('Ctrl Pts',(-3.1066790790198,-1.,-2.46446082979646));
#46453=CARTESIAN_POINT('Ctrl Pts',(-3.1066790790198,1.,-2.46446082979646));
#46454=CARTESIAN_POINT('Ctrl Pts',(-3.11380805536122,-1.,-2.46700558843506));
#46455=CARTESIAN_POINT('Ctrl Pts',(-3.11380805536122,1.,-2.46700558843506));
#46456=CARTESIAN_POINT('Ctrl Pts',(-3.12096015766983,-1.,-2.46951098947469));
#46457=CARTESIAN_POINT('Ctrl Pts',(-3.12096015766983,1.,-2.46951098947469));
#46458=CARTESIAN_POINT('Ctrl Pts',(-3.12813790805952,-1.,-2.47197997765871));
#46459=CARTESIAN_POINT('Ctrl Pts',(-3.12813790805952,1.,-2.47197997765871));
#46460=CARTESIAN_POINT('Ctrl Pts',(-3.13534181229295,-1.,-2.47441378371932));
#46461=CARTESIAN_POINT('Ctrl Pts',(-3.13534181229295,1.,-2.47441378371932));
#46462=CARTESIAN_POINT('Ctrl Pts',(-3.1425709954655,-1.,-2.47681245356109));
#46463=CARTESIAN_POINT('Ctrl Pts',(-3.1425709954655,1.,-2.47681245356109));
#46464=CARTESIAN_POINT('Ctrl Pts',(-3.14982373241352,-1.,-2.47917529057029));
#46465=CARTESIAN_POINT('Ctrl Pts',(-3.14982373241352,1.,-2.47917529057029));
#46466=CARTESIAN_POINT('Ctrl Pts',(-3.15709802322739,-1.,-2.48150133566571));
#46467=CARTESIAN_POINT('Ctrl Pts',(-3.15709802322739,1.,-2.48150133566571));
#46468=CARTESIAN_POINT('Ctrl Pts',(-3.16439213290161,-1.,-2.48378981792725));
#46469=CARTESIAN_POINT('Ctrl Pts',(-3.16439213290161,1.,-2.48378981792725));
#46470=CARTESIAN_POINT('Ctrl Pts',(-3.17170518863313,-1.,-2.48604065348587));
#46471=CARTESIAN_POINT('Ctrl Pts',(-3.17170518863313,1.,-2.48604065348587));
#46472=CARTESIAN_POINT('Ctrl Pts',(-3.17903698136622,-1.,-2.48825428288201));
#46473=CARTESIAN_POINT('Ctrl Pts',(-3.17903698136622,1.,-2.48825428288201));
#46474=CARTESIAN_POINT('Ctrl Pts',(-3.18638771282266,-1.,-2.49043146334059));
#46475=CARTESIAN_POINT('Ctrl Pts',(-3.18638771282266,1.,-2.49043146334059));
#46476=CARTESIAN_POINT('Ctrl Pts',(-3.19375775555798,-1.,-2.49257307239848));
#46477=CARTESIAN_POINT('Ctrl Pts',(-3.19375775555798,1.,-2.49257307239848));
#46478=CARTESIAN_POINT('Ctrl Pts',(-3.20114742397588,-1.,-2.49467992057755));
#46479=CARTESIAN_POINT('Ctrl Pts',(-3.20114742397588,1.,-2.49467992057755));
#46480=CARTESIAN_POINT('Ctrl Pts',(-3.20855669849836,-1.,-2.4967525264737));
#46481=CARTESIAN_POINT('Ctrl Pts',(-3.20855669849836,1.,-2.4967525264737));
#46482=CARTESIAN_POINT('Ctrl Pts',(-3.21598526261286,-1.,-2.4987911459939));
#46483=CARTESIAN_POINT('Ctrl Pts',(-3.21598526261286,1.,-2.4987911459939));
#46484=CARTESIAN_POINT('Ctrl Pts',(-3.22343262620503,-1.,-2.50079587201957));
#46485=CARTESIAN_POINT('Ctrl Pts',(-3.22343262620503,1.,-2.50079587201957));
#46486=CARTESIAN_POINT('Ctrl Pts',(-3.23089822320646,-1.,-2.50276671338111));
#46487=CARTESIAN_POINT('Ctrl Pts',(-3.23089822320646,1.,-2.50276671338111));
#46488=CARTESIAN_POINT('Ctrl Pts',(-3.23838151080319,-1.,-2.5047036758003));
#46489=CARTESIAN_POINT('Ctrl Pts',(-3.23838151080319,1.,-2.5047036758003));
#46490=CARTESIAN_POINT('Ctrl Pts',(-3.24588208983849,-1.,-2.506606859405));
#46491=CARTESIAN_POINT('Ctrl Pts',(-3.24588208983849,1.,-2.506606859405));
#46492=CARTESIAN_POINT('Ctrl Pts',(-3.25339971460982,-1.,-2.50847647070723));
#46493=CARTESIAN_POINT('Ctrl Pts',(-3.25339971460982,1.,-2.50847647070723));
#46494=CARTESIAN_POINT('Ctrl Pts',(-3.26093423001434,-1.,-2.51031277813486));
#46495=CARTESIAN_POINT('Ctrl Pts',(-3.26093423001434,1.,-2.51031277813486));
#46496=CARTESIAN_POINT('Ctrl Pts',(-3.26848552888115,-1.,-2.51211608411423));
#46497=CARTESIAN_POINT('Ctrl Pts',(-3.26848552888115,1.,-2.51211608411423));
#46498=CARTESIAN_POINT('Ctrl Pts',(-3.27605350473142,-1.,-2.513886692704));
#46499=CARTESIAN_POINT('Ctrl Pts',(-3.27605350473142,1.,-2.513886692704));
#46500=CARTESIAN_POINT('Ctrl Pts',(-3.28363799702982,-1.,-2.51562487464514));
#46501=CARTESIAN_POINT('Ctrl Pts',(-3.28363799702982,1.,-2.51562487464514));
#46502=CARTESIAN_POINT('Ctrl Pts',(-3.2912387729927,-1.,-2.51733085123797));
#46503=CARTESIAN_POINT('Ctrl Pts',(-3.2912387729927,1.,-2.51733085123797));
#46504=CARTESIAN_POINT('Ctrl Pts',(-3.29885556388352,-1.,-2.51900480701069));
#46505=CARTESIAN_POINT('Ctrl Pts',(-3.29885556388352,1.,-2.51900480701069));
#46506=CARTESIAN_POINT('Ctrl Pts',(-3.30648808815442,-1.,-2.52064689568511));
#46507=CARTESIAN_POINT('Ctrl Pts',(-3.30648808815442,1.,-2.52064689568511));
#46508=CARTESIAN_POINT('Ctrl Pts',(-3.31413607874645,-1.,-2.52225724871313));
#46509=CARTESIAN_POINT('Ctrl Pts',(-3.31413607874645,1.,-2.52225724871313));
#46510=CARTESIAN_POINT('Ctrl Pts',(-3.32179931078699,-1.,-2.5238359839626));
#46511=CARTESIAN_POINT('Ctrl Pts',(-3.32179931078699,1.,-2.5238359839626));
#46512=CARTESIAN_POINT('Ctrl Pts',(-3.32947762187533,-1.,-2.52538321164634));
#46513=CARTESIAN_POINT('Ctrl Pts',(-3.32947762187533,1.,-2.52538321164634));
#46514=CARTESIAN_POINT('Ctrl Pts',(-3.33717089999103,-1.,-2.52689902690158));
#46515=CARTESIAN_POINT('Ctrl Pts',(-3.33717089999103,1.,-2.52689902690158));
#46516=CARTESIAN_POINT('Ctrl Pts',(-3.34333744115511,-1.,-2.52808660915689));
#46517=CARTESIAN_POINT('Ctrl Pts',(-3.34333744115511,1.,-2.52808660915689));
#46518=CARTESIAN_POINT('Ctrl Pts',(-3.34796903576663,-1.,-2.52896321610703));
#46519=CARTESIAN_POINT('Ctrl Pts',(-3.34796903576663,1.,-2.52896321610703));
#46520=CARTESIAN_POINT('Ctrl Pts',(-3.35105973714071,-1.,-2.5295413654909));
#46521=CARTESIAN_POINT('Ctrl Pts',(-3.35105973714071,1.,-2.5295413654909));
#46522=CARTESIAN_POINT('Ctrl Pts',(-3.35260583073571,-1.,-2.52982887637028));
#46523=CARTESIAN_POINT('Ctrl Pts',(-3.35260583073571,1.,-2.52982887637028));
#46524=CARTESIAN_POINT('',(-2.90994629141676,1.,-2.36531447826073));
#46525=CARTESIAN_POINT('Ctrl Pts',(-2.90994629141676,-1.,-2.36531447826074));
#46526=CARTESIAN_POINT('Ctrl Pts',(-2.90994629141676,-0.666666666666667,
-2.36531447826074));
#46527=CARTESIAN_POINT('Ctrl Pts',(-2.90994629141676,-0.333333333333333,
-2.36531447826074));
#46528=CARTESIAN_POINT('Ctrl Pts',(-2.90994629141676,0.333333333333333,
-2.36531447826074));
#46529=CARTESIAN_POINT('Ctrl Pts',(-2.90994629141676,0.666666666666667,
-2.36531447826074));
#46530=CARTESIAN_POINT('Ctrl Pts',(-2.90994629141676,1.,-2.36531447826074));
#46531=CARTESIAN_POINT('',(-3.35260583073571,1.,-2.52982887637028));
#46532=CARTESIAN_POINT('',(-3.35260583073571,0.,-2.52982887637028));
#46533=CARTESIAN_POINT('Ctrl Pts',(-2.90994629141676,1.,-2.36531447826073));
#46534=CARTESIAN_POINT('Ctrl Pts',(-2.90995756655606,1.,-2.36536211188453));
#46535=CARTESIAN_POINT('Ctrl Pts',(-2.91005770527719,1.,-2.36553202948613));
#46536=CARTESIAN_POINT('Ctrl Pts',(-2.91051690822156,1.,-2.36599991765749));
#46537=CARTESIAN_POINT('Ctrl Pts',(-2.91181344022549,1.,-2.36707658451664));
#46538=CARTESIAN_POINT('Ctrl Pts',(-2.9146124988314,1.,-2.36919161373173));
#46539=CARTESIAN_POINT('Ctrl Pts',(-2.91891503791411,1.,-2.37229381109821));
#46540=CARTESIAN_POINT('Ctrl Pts',(-2.92430340582608,1.,-2.3760651052403));
#46541=CARTESIAN_POINT('Ctrl Pts',(-2.93049643640206,1.,-2.38028989582073));
#46542=CARTESIAN_POINT('Ctrl Pts',(-2.93717903280391,1.,-2.38472771516311));
#46543=CARTESIAN_POINT('Ctrl Pts',(-2.94404820669076,1.,-2.38914929090759));
#46544=CARTESIAN_POINT('Ctrl Pts',(-2.95085857128439,1.,-2.39337207631667));
#46545=CARTESIAN_POINT('Ctrl Pts',(-2.95748006482942,1.,-2.39730553974517));
#46546=CARTESIAN_POINT('Ctrl Pts',(-2.96390432240312,1.,-2.4009556571164));
#46547=CARTESIAN_POINT('Ctrl Pts',(-2.9701964131236,1.,-2.40438604734919));
#46548=CARTESIAN_POINT('Ctrl Pts',(-2.97646002822422,1.,-2.40768975073713));
#46549=CARTESIAN_POINT('Ctrl Pts',(-2.98280015815107,1.,-2.41095909342571));
#46550=CARTESIAN_POINT('Ctrl Pts',(-2.98927983005796,1.,-2.41425064199586));
#46551=CARTESIAN_POINT('Ctrl Pts',(-2.99590509293503,1.,-2.41757324500514));
#46552=CARTESIAN_POINT('Ctrl Pts',(-3.00264868585996,1.,-2.42090763946779));
#46553=CARTESIAN_POINT('Ctrl Pts',(-3.00946442616658,1.,-2.42421849439613));
#46554=CARTESIAN_POINT('Ctrl Pts',(-3.01630420830504,1.,-2.42746856264168));
#46555=CARTESIAN_POINT('Ctrl Pts',(-3.02313656036004,1.,-2.43063415586637));
#46556=CARTESIAN_POINT('Ctrl Pts',(-3.02995534946978,1.,-2.43371241361488));
#46557=CARTESIAN_POINT('Ctrl Pts',(-3.03676949672821,1.,-2.43671278042414));
#46558=CARTESIAN_POINT('Ctrl Pts',(-3.04359685040555,1.,-2.43965194061857));
#46559=CARTESIAN_POINT('Ctrl Pts',(-3.05045678021504,1.,-2.44254768923105));
#46560=CARTESIAN_POINT('Ctrl Pts',(-3.05736242671506,1.,-2.44541251892556));
#46561=CARTESIAN_POINT('Ctrl Pts',(-3.06431596421405,1.,-2.44824970516544));
#46562=CARTESIAN_POINT('Ctrl Pts',(-3.07131290521297,1.,-2.45105688854422));
#46563=CARTESIAN_POINT('Ctrl Pts',(-3.07834472886139,1.,-2.4538282678779));
#46564=CARTESIAN_POINT('Ctrl Pts',(-3.08540206545315,1.,-2.45655725437039));
#46565=CARTESIAN_POINT('Ctrl Pts',(-3.09247787931887,1.,-2.4592391256388));
#46566=CARTESIAN_POINT('Ctrl Pts',(-3.09956993697052,1.,-2.46187308501884));
#46567=CARTESIAN_POINT('Ctrl Pts',(-3.1066790790198,1.,-2.46446082979646));
#46568=CARTESIAN_POINT('Ctrl Pts',(-3.11380805536122,1.,-2.46700558843506));
#46569=CARTESIAN_POINT('Ctrl Pts',(-3.12096015766983,1.,-2.46951098947469));
#46570=CARTESIAN_POINT('Ctrl Pts',(-3.12813790805952,1.,-2.47197997765871));
#46571=CARTESIAN_POINT('Ctrl Pts',(-3.13534181229295,1.,-2.47441378371932));
#46572=CARTESIAN_POINT('Ctrl Pts',(-3.1425709954655,1.,-2.47681245356109));
#46573=CARTESIAN_POINT('Ctrl Pts',(-3.14982373241352,1.,-2.47917529057029));
#46574=CARTESIAN_POINT('Ctrl Pts',(-3.15709802322739,1.,-2.48150133566571));
#46575=CARTESIAN_POINT('Ctrl Pts',(-3.16439213290161,1.,-2.48378981792725));
#46576=CARTESIAN_POINT('Ctrl Pts',(-3.17170518863313,1.,-2.48604065348587));
#46577=CARTESIAN_POINT('Ctrl Pts',(-3.17903698136622,1.,-2.48825428288201));
#46578=CARTESIAN_POINT('Ctrl Pts',(-3.18638771282266,1.,-2.49043146334059));
#46579=CARTESIAN_POINT('Ctrl Pts',(-3.19375775555798,1.,-2.49257307239848));
#46580=CARTESIAN_POINT('Ctrl Pts',(-3.20114742397588,1.,-2.49467992057755));
#46581=CARTESIAN_POINT('Ctrl Pts',(-3.20855669849836,1.,-2.4967525264737));
#46582=CARTESIAN_POINT('Ctrl Pts',(-3.21598526261286,1.,-2.4987911459939));
#46583=CARTESIAN_POINT('Ctrl Pts',(-3.22343262620503,1.,-2.50079587201957));
#46584=CARTESIAN_POINT('Ctrl Pts',(-3.23089822320646,1.,-2.50276671338111));
#46585=CARTESIAN_POINT('Ctrl Pts',(-3.23838151080319,1.,-2.5047036758003));
#46586=CARTESIAN_POINT('Ctrl Pts',(-3.24588208983849,1.,-2.506606859405));
#46587=CARTESIAN_POINT('Ctrl Pts',(-3.25339971460982,1.,-2.50847647070723));
#46588=CARTESIAN_POINT('Ctrl Pts',(-3.26093423001434,1.,-2.51031277813486));
#46589=CARTESIAN_POINT('Ctrl Pts',(-3.26848552888115,1.,-2.51211608411423));
#46590=CARTESIAN_POINT('Ctrl Pts',(-3.27605350473142,1.,-2.513886692704));
#46591=CARTESIAN_POINT('Ctrl Pts',(-3.28363799702982,1.,-2.51562487464514));
#46592=CARTESIAN_POINT('Ctrl Pts',(-3.2912387729927,1.,-2.51733085123797));
#46593=CARTESIAN_POINT('Ctrl Pts',(-3.29885556388352,1.,-2.51900480701069));
#46594=CARTESIAN_POINT('Ctrl Pts',(-3.30648808815442,1.,-2.52064689568511));
#46595=CARTESIAN_POINT('Ctrl Pts',(-3.31413607874645,1.,-2.52225724871313));
#46596=CARTESIAN_POINT('Ctrl Pts',(-3.32179931078699,1.,-2.5238359839626));
#46597=CARTESIAN_POINT('Ctrl Pts',(-3.32947762187533,1.,-2.52538321164634));
#46598=CARTESIAN_POINT('Ctrl Pts',(-3.33717089999103,1.,-2.52689902690158));
#46599=CARTESIAN_POINT('Ctrl Pts',(-3.34333744115511,1.,-2.52808660915689));
#46600=CARTESIAN_POINT('Ctrl Pts',(-3.34796903576663,1.,-2.52896321610703));
#46601=CARTESIAN_POINT('Ctrl Pts',(-3.35105973714071,1.,-2.5295413654909));
#46602=CARTESIAN_POINT('Ctrl Pts',(-3.35260583073571,1.,-2.52982887637028));
#46603=CARTESIAN_POINT('Origin',(-3.35260583073571,0.,-2.52982887637028));
#46604=CARTESIAN_POINT('',(-3.44202241512147,1.,-2.40675750623143));
#46605=CARTESIAN_POINT('Origin',(0.,0.,0.));
#46606=CARTESIAN_POINT('',(-2.79140942341378,1.,-2.50410331873042));
#46607=CARTESIAN_POINT('Origin',(0.,1.,0.));
#46608=CARTESIAN_POINT('Ctrl Pts',(-2.79140942341378,1.,-2.50410331873042));
#46609=CARTESIAN_POINT('Ctrl Pts',(-2.79140942341378,0.666666666666667,
-2.50410331873042));
#46610=CARTESIAN_POINT('Ctrl Pts',(-2.79140942341378,0.333333333333333,
-2.50410331873042));
#46611=CARTESIAN_POINT('Ctrl Pts',(-2.79140942341378,-0.333333333333333,
-2.50410331873042));
#46612=CARTESIAN_POINT('Ctrl Pts',(-2.79140942341378,-0.666666666666667,
-2.50410331873042));
#46613=CARTESIAN_POINT('Ctrl Pts',(-2.79140942341378,-1.,-2.50410331873042));
#46614=CARTESIAN_POINT('Ctrl Pts',(-3.02314558451372,-1.,-2.91557726271063));
#46615=CARTESIAN_POINT('Ctrl Pts',(-3.02314558451372,1.,-2.91557726271063));
#46616=CARTESIAN_POINT('Ctrl Pts',(-3.02261975104912,-1.,-2.91409518070707));
#46617=CARTESIAN_POINT('Ctrl Pts',(-3.02261975104912,1.,-2.91409518070707));
#46618=CARTESIAN_POINT('Ctrl Pts',(-3.02156522743299,-1.,-2.91113297349052));
#46619=CARTESIAN_POINT('Ctrl Pts',(-3.02156522743299,1.,-2.91113297349052));
#46620=CARTESIAN_POINT('Ctrl Pts',(-3.01997487194926,-1.,-2.90669553303902));
#46621=CARTESIAN_POINT('Ctrl Pts',(-3.01997487194926,1.,-2.90669553303902));
#46622=CARTESIAN_POINT('Ctrl Pts',(-3.01783725123646,-1.,-2.90079069102661));
#46623=CARTESIAN_POINT('Ctrl Pts',(-3.01783725123646,1.,-2.90079069102661));
#46624=CARTESIAN_POINT('Ctrl Pts',(-3.01513660433291,-1.,-2.8934292556764));
#46625=CARTESIAN_POINT('Ctrl Pts',(-3.01513660433291,1.,-2.8934292556764));
#46626=CARTESIAN_POINT('Ctrl Pts',(-3.01240727309568,-1.,-2.88608751706796));
#46627=CARTESIAN_POINT('Ctrl Pts',(-3.01240727309568,1.,-2.88608751706796));
#46628=CARTESIAN_POINT('Ctrl Pts',(-3.0096491810855,-1.,-2.87876560072799));
#46629=CARTESIAN_POINT('Ctrl Pts',(-3.0096491810855,1.,-2.87876560072799));
#46630=CARTESIAN_POINT('Ctrl Pts',(-3.00686224485374,-1.,-2.87146368430104));
#46631=CARTESIAN_POINT('Ctrl Pts',(-3.00686224485374,1.,-2.87146368430104));
#46632=CARTESIAN_POINT('Ctrl Pts',(-3.00404638316245,-1.,-2.86418200833065));
#46633=CARTESIAN_POINT('Ctrl Pts',(-3.00404638316245,1.,-2.86418200833065));
#46634=CARTESIAN_POINT('Ctrl Pts',(-3.0012015079552,-1.,-2.85692085715129));
#46635=CARTESIAN_POINT('Ctrl Pts',(-3.0012015079552,1.,-2.85692085715129));
#46636=CARTESIAN_POINT('Ctrl Pts',(-2.99832751144566,-1.,-2.84968053289104));
#46637=CARTESIAN_POINT('Ctrl Pts',(-2.99832751144566,1.,-2.84968053289104));
#46638=CARTESIAN_POINT('Ctrl Pts',(-2.995424253416,-1.,-2.84246132984334));
#46639=CARTESIAN_POINT('Ctrl Pts',(-2.995424253416,1.,-2.84246132984334));
#46640=CARTESIAN_POINT('Ctrl Pts',(-2.99249155170479,-1.,-2.83526351254383));
#46641=CARTESIAN_POINT('Ctrl Pts',(-2.99249155170479,1.,-2.83526351254383));
#46642=CARTESIAN_POINT('Ctrl Pts',(-2.98952916401699,-1.,-2.82808728190402));
#46643=CARTESIAN_POINT('Ctrl Pts',(-2.98952916401699,1.,-2.82808728190402));
#46644=CARTESIAN_POINT('Ctrl Pts',(-2.98653680669434,-1.,-2.82093279065704));
#46645=CARTESIAN_POINT('Ctrl Pts',(-2.98653680669434,1.,-2.82093279065704));
#46646=CARTESIAN_POINT('Ctrl Pts',(-2.9835141977994,-1.,-2.81380019196454));
#46647=CARTESIAN_POINT('Ctrl Pts',(-2.9835141977994,1.,-2.81380019196454));
#46648=CARTESIAN_POINT('Ctrl Pts',(-2.98046109647299,-1.,-2.80668968101162));
#46649=CARTESIAN_POINT('Ctrl Pts',(-2.98046109647299,1.,-2.80668968101162));
#46650=CARTESIAN_POINT('Ctrl Pts',(-2.97737733718242,-1.,-2.79960153278186));
#46651=CARTESIAN_POINT('Ctrl Pts',(-2.97737733718242,1.,-2.79960153278186));
#46652=CARTESIAN_POINT('Ctrl Pts',(-2.97426288347475,-1.,-2.79253615718147));
#46653=CARTESIAN_POINT('Ctrl Pts',(-2.97426288347475,1.,-2.79253615718147));
#46654=CARTESIAN_POINT('Ctrl Pts',(-2.97111781461349,-1.,-2.78549409123657));
#46655=CARTESIAN_POINT('Ctrl Pts',(-2.97111781461349,1.,-2.78549409123657));
#46656=CARTESIAN_POINT('Ctrl Pts',(-2.9679422104295,-1.,-2.77847589542767));
#46657=CARTESIAN_POINT('Ctrl Pts',(-2.9679422104295,1.,-2.77847589542767));
#46658=CARTESIAN_POINT('Ctrl Pts',(-2.96473605585548,-1.,-2.77148206836464));
#46659=CARTESIAN_POINT('Ctrl Pts',(-2.96473605585548,1.,-2.77148206836464));
#46660=CARTESIAN_POINT('Ctrl Pts',(-2.96149914764832,-1.,-2.76451296269571));
#46661=CARTESIAN_POINT('Ctrl Pts',(-2.96149914764832,1.,-2.76451296269571));
#46662=CARTESIAN_POINT('Ctrl Pts',(-2.9582309766594,-1.,-2.75756867888393));
#46663=CARTESIAN_POINT('Ctrl Pts',(-2.9582309766594,1.,-2.75756867888393));
#46664=CARTESIAN_POINT('Ctrl Pts',(-2.95493069316211,-1.,-2.75064903318996));
#46665=CARTESIAN_POINT('Ctrl Pts',(-2.95493069316211,1.,-2.75064903318996));
#46666=CARTESIAN_POINT('Ctrl Pts',(-2.95159737214305,-1.,-2.7437537949221));
#46667=CARTESIAN_POINT('Ctrl Pts',(-2.95159737214305,1.,-2.7437537949221));
#46668=CARTESIAN_POINT('Ctrl Pts',(-2.94823023414381,-1.,-2.73688288329825));
#46669=CARTESIAN_POINT('Ctrl Pts',(-2.94823023414381,1.,-2.73688288329825));
#46670=CARTESIAN_POINT('Ctrl Pts',(-2.94482887675139,-1.,-2.73003657371613));
#46671=CARTESIAN_POINT('Ctrl Pts',(-2.94482887675139,1.,-2.73003657371613));
#46672=CARTESIAN_POINT('Ctrl Pts',(-2.94139351933882,-1.,-2.72321571511322));
#46673=CARTESIAN_POINT('Ctrl Pts',(-2.94139351933882,1.,-2.72321571511322));
#46674=CARTESIAN_POINT('Ctrl Pts',(-2.93792519474955,-1.,-2.71642190053575));
#46675=CARTESIAN_POINT('Ctrl Pts',(-2.93792519474955,1.,-2.71642190053575));
#46676=CARTESIAN_POINT('Ctrl Pts',(-2.93442516311168,-1.,-2.70965695523776));
#46677=CARTESIAN_POINT('Ctrl Pts',(-2.93442516311168,1.,-2.70965695523776));
#46678=CARTESIAN_POINT('Ctrl Pts',(-2.93089438233746,-1.,-2.70292247416881));
#46679=CARTESIAN_POINT('Ctrl Pts',(-2.93089438233746,1.,-2.70292247416881));
#46680=CARTESIAN_POINT('Ctrl Pts',(-2.92733294395268,-1.,-2.69621932864302));
#46681=CARTESIAN_POINT('Ctrl Pts',(-2.92733294395268,1.,-2.69621932864302));
#46682=CARTESIAN_POINT('Ctrl Pts',(-2.92373955325876,-1.,-2.68954721165342));
#46683=CARTESIAN_POINT('Ctrl Pts',(-2.92373955325876,1.,-2.68954721165342));
#46684=CARTESIAN_POINT('Ctrl Pts',(-2.92011090722152,-1.,-2.68290409279689));
#46685=CARTESIAN_POINT('Ctrl Pts',(-2.92011090722152,1.,-2.68290409279689));
#46686=CARTESIAN_POINT('Ctrl Pts',(-2.91644290704281,-1.,-2.67628728855309));
#46687=CARTESIAN_POINT('Ctrl Pts',(-2.91644290704281,1.,-2.67628728855309));
#46688=CARTESIAN_POINT('Ctrl Pts',(-2.91273193382876,-1.,-2.66969458792627));
#46689=CARTESIAN_POINT('Ctrl Pts',(-2.91273193382876,1.,-2.66969458792627));
#46690=CARTESIAN_POINT('Ctrl Pts',(-2.90897617968921,-1.,-2.66312542616808));
#46691=CARTESIAN_POINT('Ctrl Pts',(-2.90897617968921,1.,-2.66312542616808));
#46692=CARTESIAN_POINT('Ctrl Pts',(-2.90517678087467,-1.,-2.65658188464287));
#46693=CARTESIAN_POINT('Ctrl Pts',(-2.90517678087467,1.,-2.65658188464287));
#46694=CARTESIAN_POINT('Ctrl Pts',(-2.90133950224879,-1.,-2.65007017365576));
#46695=CARTESIAN_POINT('Ctrl Pts',(-2.90133950224879,1.,-2.65007017365576));
#46696=CARTESIAN_POINT('Ctrl Pts',(-2.89747231723361,-1.,-2.64359851684146));
#46697=CARTESIAN_POINT('Ctrl Pts',(-2.89747231723361,1.,-2.64359851684146));
#46698=CARTESIAN_POINT('Ctrl Pts',(-2.89358228854557,-1.,-2.63717442263944));
#46699=CARTESIAN_POINT('Ctrl Pts',(-2.89358228854557,1.,-2.63717442263944));
#46700=CARTESIAN_POINT('Ctrl Pts',(-2.88967244854243,-1.,-2.63080195420771));
#46701=CARTESIAN_POINT('Ctrl Pts',(-2.88967244854243,1.,-2.63080195420771));
#46702=CARTESIAN_POINT('Ctrl Pts',(-2.88573922195049,-1.,-2.62447947640253));
#46703=CARTESIAN_POINT('Ctrl Pts',(-2.88573922195049,1.,-2.62447947640253));
#46704=CARTESIAN_POINT('Ctrl Pts',(-2.88176821427502,-1.,-2.61819596473087));
#46705=CARTESIAN_POINT('Ctrl Pts',(-2.88176821427502,1.,-2.61819596473087));
#46706=CARTESIAN_POINT('Ctrl Pts',(-2.87773881947885,-1.,-2.61193507170928));
#46707=CARTESIAN_POINT('Ctrl Pts',(-2.87773881947885,1.,-2.61193507170928));
#46708=CARTESIAN_POINT('Ctrl Pts',(-2.87363176656475,-1.,-2.6056817788128));
#46709=CARTESIAN_POINT('Ctrl Pts',(-2.87363176656475,1.,-2.6056817788128));
#46710=CARTESIAN_POINT('Ctrl Pts',(-2.86943633170712,-1.,-2.59942875223202));
#46711=CARTESIAN_POINT('Ctrl Pts',(-2.86943633170712,1.,-2.59942875223202));
#46712=CARTESIAN_POINT('Ctrl Pts',(-2.86515629953528,-1.,-2.59318160184921));
#46713=CARTESIAN_POINT('Ctrl Pts',(-2.86515629953528,1.,-2.59318160184921));
#46714=CARTESIAN_POINT('Ctrl Pts',(-2.86081999003668,-1.,-2.5869677064356));
#46715=CARTESIAN_POINT('Ctrl Pts',(-2.86081999003668,1.,-2.5869677064356));
#46716=CARTESIAN_POINT('Ctrl Pts',(-2.85647171715147,-1.,-2.58082875254407));
#46717=CARTESIAN_POINT('Ctrl Pts',(-2.85647171715147,1.,-2.58082875254407));
#46718=CARTESIAN_POINT('Ctrl Pts',(-2.85215360144483,-1.,-2.57480482727128));
#46719=CARTESIAN_POINT('Ctrl Pts',(-2.85215360144483,1.,-2.57480482727128));
#46720=CARTESIAN_POINT('Ctrl Pts',(-2.84788893329091,-1.,-2.56891984251743));
#46721=CARTESIAN_POINT('Ctrl Pts',(-2.84788893329091,1.,-2.56891984251743));
#46722=CARTESIAN_POINT('Ctrl Pts',(-2.84366802680211,-1.,-2.56316920798489));
#46723=CARTESIAN_POINT('Ctrl Pts',(-2.84366802680211,1.,-2.56316920798489));
#46724=CARTESIAN_POINT('Ctrl Pts',(-2.83942515220699,-1.,-2.55749952145165));
#46725=CARTESIAN_POINT('Ctrl Pts',(-2.83942515220699,1.,-2.55749952145165));
#46726=CARTESIAN_POINT('Ctrl Pts',(-2.83505269592412,-1.,-2.55182152806964));
#46727=CARTESIAN_POINT('Ctrl Pts',(-2.83505269592412,1.,-2.55182152806964));
#46728=CARTESIAN_POINT('Ctrl Pts',(-2.83044254225794,-1.,-2.54604736792542));
#46729=CARTESIAN_POINT('Ctrl Pts',(-2.83044254225794,1.,-2.54604736792542));
#46730=CARTESIAN_POINT('Ctrl Pts',(-2.82552167649157,-1.,-2.54012272520141));
#46731=CARTESIAN_POINT('Ctrl Pts',(-2.82552167649157,1.,-2.54012272520141));
#46732=CARTESIAN_POINT('Ctrl Pts',(-2.82028550483744,-1.,-2.53405679667463));
#46733=CARTESIAN_POINT('Ctrl Pts',(-2.82028550483744,1.,-2.53405679667463));
#46734=CARTESIAN_POINT('Ctrl Pts',(-2.8148437904867,-1.,-2.52796388055457));
#46735=CARTESIAN_POINT('Ctrl Pts',(-2.8148437904867,1.,-2.52796388055457));
#46736=CARTESIAN_POINT('Ctrl Pts',(-2.80941521967234,-1.,-2.52205778589922));
#46737=CARTESIAN_POINT('Ctrl Pts',(-2.80941521967234,1.,-2.52205778589922));
#46738=CARTESIAN_POINT('Ctrl Pts',(-2.80427363984939,-1.,-2.51660190466067));
#46739=CARTESIAN_POINT('Ctrl Pts',(-2.80427363984939,1.,-2.51660190466067));
#46740=CARTESIAN_POINT('Ctrl Pts',(-2.79970585014308,-1.,-2.51186983687947));
#46741=CARTESIAN_POINT('Ctrl Pts',(-2.79970585014308,1.,-2.51186983687947));
#46742=CARTESIAN_POINT('Ctrl Pts',(-2.7959687805717,-1.,-2.50810555977564));
#46743=CARTESIAN_POINT('Ctrl Pts',(-2.7959687805717,1.,-2.50810555977564));
#46744=CARTESIAN_POINT('Ctrl Pts',(-2.79323694088143,-1.,-2.50547439929077));
#46745=CARTESIAN_POINT('Ctrl Pts',(-2.79323694088143,1.,-2.50547439929077));
#46746=CARTESIAN_POINT('Ctrl Pts',(-2.79192122906739,-1.,-2.50433799076945));
#46747=CARTESIAN_POINT('Ctrl Pts',(-2.79192122906739,1.,-2.50433799076945));
#46748=CARTESIAN_POINT('Ctrl Pts',(-2.79143626022225,-1.,-2.50404230339032));
#46749=CARTESIAN_POINT('Ctrl Pts',(-2.79143626022225,1.,-2.50404230339032));
#46750=CARTESIAN_POINT('Ctrl Pts',(-2.79133581100044,-1.,-2.50409239460011));
#46751=CARTESIAN_POINT('Ctrl Pts',(-2.79133581100044,1.,-2.50409239460011));
#46752=CARTESIAN_POINT('Ctrl Pts',(-2.79134130681569,-1.,-2.50417924854921));
#46753=CARTESIAN_POINT('Ctrl Pts',(-2.79134130681569,1.,-2.50417924854921));
#46754=CARTESIAN_POINT('',(-3.02314558451372,1.,-2.91557726271063));
#46755=CARTESIAN_POINT('Ctrl Pts',(-3.02314558451372,1.,-2.91557726271063));
#46756=CARTESIAN_POINT('Ctrl Pts',(-3.02261975104912,1.,-2.91409518070707));
#46757=CARTESIAN_POINT('Ctrl Pts',(-3.02156522743299,1.,-2.91113297349052));
#46758=CARTESIAN_POINT('Ctrl Pts',(-3.01997487194926,1.,-2.90669553303902));
#46759=CARTESIAN_POINT('Ctrl Pts',(-3.01783725123646,1.,-2.90079069102661));
#46760=CARTESIAN_POINT('Ctrl Pts',(-3.01513660433291,1.,-2.8934292556764));
#46761=CARTESIAN_POINT('Ctrl Pts',(-3.01240727309568,1.,-2.88608751706796));
#46762=CARTESIAN_POINT('Ctrl Pts',(-3.0096491810855,1.,-2.87876560072799));
#46763=CARTESIAN_POINT('Ctrl Pts',(-3.00686224485374,1.,-2.87146368430104));
#46764=CARTESIAN_POINT('Ctrl Pts',(-3.00404638316245,1.,-2.86418200833065));
#46765=CARTESIAN_POINT('Ctrl Pts',(-3.0012015079552,1.,-2.85692085715129));
#46766=CARTESIAN_POINT('Ctrl Pts',(-2.99832751144566,1.,-2.84968053289104));
#46767=CARTESIAN_POINT('Ctrl Pts',(-2.995424253416,1.,-2.84246132984334));
#46768=CARTESIAN_POINT('Ctrl Pts',(-2.99249155170479,1.,-2.83526351254383));
#46769=CARTESIAN_POINT('Ctrl Pts',(-2.98952916401699,1.,-2.82808728190402));
#46770=CARTESIAN_POINT('Ctrl Pts',(-2.98653680669434,1.,-2.82093279065704));
#46771=CARTESIAN_POINT('Ctrl Pts',(-2.9835141977994,1.,-2.81380019196454));
#46772=CARTESIAN_POINT('Ctrl Pts',(-2.98046109647299,1.,-2.80668968101162));
#46773=CARTESIAN_POINT('Ctrl Pts',(-2.97737733718242,1.,-2.79960153278186));
#46774=CARTESIAN_POINT('Ctrl Pts',(-2.97426288347475,1.,-2.79253615718147));
#46775=CARTESIAN_POINT('Ctrl Pts',(-2.97111781461349,1.,-2.78549409123657));
#46776=CARTESIAN_POINT('Ctrl Pts',(-2.9679422104295,1.,-2.77847589542767));
#46777=CARTESIAN_POINT('Ctrl Pts',(-2.96473605585548,1.,-2.77148206836464));
#46778=CARTESIAN_POINT('Ctrl Pts',(-2.96149914764832,1.,-2.76451296269571));
#46779=CARTESIAN_POINT('Ctrl Pts',(-2.9582309766594,1.,-2.75756867888393));
#46780=CARTESIAN_POINT('Ctrl Pts',(-2.95493069316211,1.,-2.75064903318996));
#46781=CARTESIAN_POINT('Ctrl Pts',(-2.95159737214305,1.,-2.7437537949221));
#46782=CARTESIAN_POINT('Ctrl Pts',(-2.94823023414381,1.,-2.73688288329825));
#46783=CARTESIAN_POINT('Ctrl Pts',(-2.94482887675139,1.,-2.73003657371613));
#46784=CARTESIAN_POINT('Ctrl Pts',(-2.94139351933882,1.,-2.72321571511322));
#46785=CARTESIAN_POINT('Ctrl Pts',(-2.93792519474955,1.,-2.71642190053575));
#46786=CARTESIAN_POINT('Ctrl Pts',(-2.93442516311168,1.,-2.70965695523776));
#46787=CARTESIAN_POINT('Ctrl Pts',(-2.93089438233746,1.,-2.70292247416881));
#46788=CARTESIAN_POINT('Ctrl Pts',(-2.92733294395268,1.,-2.69621932864302));
#46789=CARTESIAN_POINT('Ctrl Pts',(-2.92373955325876,1.,-2.68954721165342));
#46790=CARTESIAN_POINT('Ctrl Pts',(-2.92011090722152,1.,-2.68290409279689));
#46791=CARTESIAN_POINT('Ctrl Pts',(-2.91644290704281,1.,-2.67628728855309));
#46792=CARTESIAN_POINT('Ctrl Pts',(-2.91273193382876,1.,-2.66969458792627));
#46793=CARTESIAN_POINT('Ctrl Pts',(-2.90897617968921,1.,-2.66312542616808));
#46794=CARTESIAN_POINT('Ctrl Pts',(-2.90517678087467,1.,-2.65658188464287));
#46795=CARTESIAN_POINT('Ctrl Pts',(-2.90133950224879,1.,-2.65007017365576));
#46796=CARTESIAN_POINT('Ctrl Pts',(-2.89747231723361,1.,-2.64359851684146));
#46797=CARTESIAN_POINT('Ctrl Pts',(-2.89358228854557,1.,-2.63717442263944));
#46798=CARTESIAN_POINT('Ctrl Pts',(-2.88967244854243,1.,-2.63080195420771));
#46799=CARTESIAN_POINT('Ctrl Pts',(-2.88573922195049,1.,-2.62447947640253));
#46800=CARTESIAN_POINT('Ctrl Pts',(-2.88176821427502,1.,-2.61819596473087));
#46801=CARTESIAN_POINT('Ctrl Pts',(-2.87773881947885,1.,-2.61193507170928));
#46802=CARTESIAN_POINT('Ctrl Pts',(-2.87363176656475,1.,-2.6056817788128));
#46803=CARTESIAN_POINT('Ctrl Pts',(-2.86943633170712,1.,-2.59942875223202));
#46804=CARTESIAN_POINT('Ctrl Pts',(-2.86515629953528,1.,-2.59318160184921));
#46805=CARTESIAN_POINT('Ctrl Pts',(-2.86081999003668,1.,-2.5869677064356));
#46806=CARTESIAN_POINT('Ctrl Pts',(-2.85647171715147,1.,-2.58082875254407));
#46807=CARTESIAN_POINT('Ctrl Pts',(-2.85215360144483,1.,-2.57480482727128));
#46808=CARTESIAN_POINT('Ctrl Pts',(-2.84788893329091,1.,-2.56891984251743));
#46809=CARTESIAN_POINT('Ctrl Pts',(-2.84366802680211,1.,-2.56316920798489));
#46810=CARTESIAN_POINT('Ctrl Pts',(-2.83942515220699,1.,-2.55749952145165));
#46811=CARTESIAN_POINT('Ctrl Pts',(-2.83505269592412,1.,-2.55182152806964));
#46812=CARTESIAN_POINT('Ctrl Pts',(-2.83044254225794,1.,-2.54604736792542));
#46813=CARTESIAN_POINT('Ctrl Pts',(-2.82552167649157,1.,-2.54012272520141));
#46814=CARTESIAN_POINT('Ctrl Pts',(-2.82028550483744,1.,-2.53405679667463));
#46815=CARTESIAN_POINT('Ctrl Pts',(-2.8148437904867,1.,-2.52796388055457));
#46816=CARTESIAN_POINT('Ctrl Pts',(-2.80941521967234,1.,-2.52205778589922));
#46817=CARTESIAN_POINT('Ctrl Pts',(-2.80427363984939,1.,-2.51660190466067));
#46818=CARTESIAN_POINT('Ctrl Pts',(-2.79970585014308,1.,-2.51186983687947));
#46819=CARTESIAN_POINT('Ctrl Pts',(-2.7959687805717,1.,-2.50810555977564));
#46820=CARTESIAN_POINT('Ctrl Pts',(-2.79344192164204,1.,-2.50567182569153));
#46821=CARTESIAN_POINT('Ctrl Pts',(-2.79217568804874,1.,-2.50455968395235));
#46822=CARTESIAN_POINT('Ctrl Pts',(-2.79164172519039,1.,-2.50417932839344));
#46823=CARTESIAN_POINT('Ctrl Pts',(-2.79145823440899,1.,-2.50410700351427));
#46824=CARTESIAN_POINT('Ctrl Pts',(-2.79140942341378,1.,-2.50410331873043));
#46825=CARTESIAN_POINT('',(-3.02314558451372,0.,-2.91557726271063));
#46826=CARTESIAN_POINT('Ctrl Pts',(-2.50417924854921,-1.,-2.79134130681569));
#46827=CARTESIAN_POINT('Ctrl Pts',(-2.50417924854921,1.,-2.79134130681569));
#46828=CARTESIAN_POINT('Ctrl Pts',(-2.50409239460108,-1.,-2.7913358110015));
#46829=CARTESIAN_POINT('Ctrl Pts',(-2.50409239460108,1.,-2.7913358110015));
#46830=CARTESIAN_POINT('Ctrl Pts',(-2.50404230339286,-1.,-2.79143626022503));
#46831=CARTESIAN_POINT('Ctrl Pts',(-2.50404230339286,1.,-2.79143626022503));
#46832=CARTESIAN_POINT('Ctrl Pts',(-2.5043379907732,-1.,-2.79192122907148));
#46833=CARTESIAN_POINT('Ctrl Pts',(-2.5043379907732,1.,-2.79192122907148));
#46834=CARTESIAN_POINT('Ctrl Pts',(-2.50547439929414,-1.,-2.7932369408851));
#46835=CARTESIAN_POINT('Ctrl Pts',(-2.50547439929414,1.,-2.7932369408851));
#46836=CARTESIAN_POINT('Ctrl Pts',(-2.50810555977671,-1.,-2.79596878057287));
#46837=CARTESIAN_POINT('Ctrl Pts',(-2.50810555977671,1.,-2.79596878057287));
#46838=CARTESIAN_POINT('Ctrl Pts',(-2.51186983687818,-1.,-2.79970585014168));
#46839=CARTESIAN_POINT('Ctrl Pts',(-2.51186983687818,1.,-2.79970585014168));
#46840=CARTESIAN_POINT('Ctrl Pts',(-2.51660190465805,-1.,-2.80427363984653));
#46841=CARTESIAN_POINT('Ctrl Pts',(-2.51660190465805,1.,-2.80427363984653));
#46842=CARTESIAN_POINT('Ctrl Pts',(-2.52205778589653,-1.,-2.80941521966941));
#46843=CARTESIAN_POINT('Ctrl Pts',(-2.52205778589653,1.,-2.80941521966941));
#46844=CARTESIAN_POINT('Ctrl Pts',(-2.52796388055278,-1.,-2.81484379048475));
#46845=CARTESIAN_POINT('Ctrl Pts',(-2.52796388055278,1.,-2.81484379048475));
#46846=CARTESIAN_POINT('Ctrl Pts',(-2.53405679667412,-1.,-2.82028550483689));
#46847=CARTESIAN_POINT('Ctrl Pts',(-2.53405679667412,1.,-2.82028550483689));
#46848=CARTESIAN_POINT('Ctrl Pts',(-2.54012272520199,-1.,-2.8255216764922));
#46849=CARTESIAN_POINT('Ctrl Pts',(-2.54012272520199,1.,-2.8255216764922));
#46850=CARTESIAN_POINT('Ctrl Pts',(-2.54604736792655,-1.,-2.83044254225917));
#46851=CARTESIAN_POINT('Ctrl Pts',(-2.54604736792655,1.,-2.83044254225917));
#46852=CARTESIAN_POINT('Ctrl Pts',(-2.55182152807077,-1.,-2.83505269592536));
#46853=CARTESIAN_POINT('Ctrl Pts',(-2.55182152807077,1.,-2.83505269592536));
#46854=CARTESIAN_POINT('Ctrl Pts',(-2.55749952145241,-1.,-2.83942515220782));
#46855=CARTESIAN_POINT('Ctrl Pts',(-2.55749952145241,1.,-2.83942515220782));
#46856=CARTESIAN_POINT('Ctrl Pts',(-2.56316920798513,-1.,-2.84366802680237));
#46857=CARTESIAN_POINT('Ctrl Pts',(-2.56316920798513,1.,-2.84366802680237));
#46858=CARTESIAN_POINT('Ctrl Pts',(-2.56891984251721,-1.,-2.84788893329067));
#46859=CARTESIAN_POINT('Ctrl Pts',(-2.56891984251721,1.,-2.84788893329067));
#46860=CARTESIAN_POINT('Ctrl Pts',(-2.57480482727081,-1.,-2.85215360144431));
#46861=CARTESIAN_POINT('Ctrl Pts',(-2.57480482727081,1.,-2.85215360144431));
#46862=CARTESIAN_POINT('Ctrl Pts',(-2.58082875254357,-1.,-2.85647171715092));
#46863=CARTESIAN_POINT('Ctrl Pts',(-2.58082875254357,1.,-2.85647171715092));
#46864=CARTESIAN_POINT('Ctrl Pts',(-2.58696770643524,-1.,-2.86081999003629));
#46865=CARTESIAN_POINT('Ctrl Pts',(-2.58696770643524,1.,-2.86081999003629));
#46866=CARTESIAN_POINT('Ctrl Pts',(-2.59318160184908,-1.,-2.86515629953513));
#46867=CARTESIAN_POINT('Ctrl Pts',(-2.59318160184908,1.,-2.86515629953513));
#46868=CARTESIAN_POINT('Ctrl Pts',(-2.5994287522321,-1.,-2.86943633170722));
#46869=CARTESIAN_POINT('Ctrl Pts',(-2.5994287522321,1.,-2.86943633170722));
#46870=CARTESIAN_POINT('Ctrl Pts',(-2.60568177881303,-1.,-2.87363176656501));
#46871=CARTESIAN_POINT('Ctrl Pts',(-2.60568177881303,1.,-2.87363176656501));
#46872=CARTESIAN_POINT('Ctrl Pts',(-2.61193507170955,-1.,-2.87773881947915));
#46873=CARTESIAN_POINT('Ctrl Pts',(-2.61193507170955,1.,-2.87773881947915));
#46874=CARTESIAN_POINT('Ctrl Pts',(-2.61819596473108,-1.,-2.88176821427525));
#46875=CARTESIAN_POINT('Ctrl Pts',(-2.61819596473108,1.,-2.88176821427525));
#46876=CARTESIAN_POINT('Ctrl Pts',(-2.62447947640262,-1.,-2.88573922195059));
#46877=CARTESIAN_POINT('Ctrl Pts',(-2.62447947640262,1.,-2.88573922195059));
#46878=CARTESIAN_POINT('Ctrl Pts',(-2.63080195420767,-1.,-2.88967244854239));
#46879=CARTESIAN_POINT('Ctrl Pts',(-2.63080195420767,1.,-2.88967244854239));
#46880=CARTESIAN_POINT('Ctrl Pts',(-2.63717442263932,-1.,-2.89358228854544));
#46881=CARTESIAN_POINT('Ctrl Pts',(-2.63717442263932,1.,-2.89358228854544));
#46882=CARTESIAN_POINT('Ctrl Pts',(-2.64359851684131,-1.,-2.89747231723345));
#46883=CARTESIAN_POINT('Ctrl Pts',(-2.64359851684131,1.,-2.89747231723345));
#46884=CARTESIAN_POINT('Ctrl Pts',(-2.65007017365564,-1.,-2.90133950224867));
#46885=CARTESIAN_POINT('Ctrl Pts',(-2.65007017365564,1.,-2.90133950224867));
#46886=CARTESIAN_POINT('Ctrl Pts',(-2.65658188464282,-1.,-2.90517678087461));
#46887=CARTESIAN_POINT('Ctrl Pts',(-2.65658188464282,1.,-2.90517678087461));
#46888=CARTESIAN_POINT('Ctrl Pts',(-2.6631254261681,-1.,-2.90897617968923));
#46889=CARTESIAN_POINT('Ctrl Pts',(-2.6631254261681,1.,-2.90897617968923));
#46890=CARTESIAN_POINT('Ctrl Pts',(-2.66969458792631,-1.,-2.91273193382882));
#46891=CARTESIAN_POINT('Ctrl Pts',(-2.66969458792631,1.,-2.91273193382882));
#46892=CARTESIAN_POINT('Ctrl Pts',(-2.67628728855312,-1.,-2.91644290704285));
#46893=CARTESIAN_POINT('Ctrl Pts',(-2.67628728855312,1.,-2.91644290704285));
#46894=CARTESIAN_POINT('Ctrl Pts',(-2.68290409279688,-1.,-2.92011090722152));
#46895=CARTESIAN_POINT('Ctrl Pts',(-2.68290409279688,1.,-2.92011090722152));
#46896=CARTESIAN_POINT('Ctrl Pts',(-2.68954721165339,-1.,-2.92373955325875));
#46897=CARTESIAN_POINT('Ctrl Pts',(-2.68954721165339,1.,-2.92373955325875));
#46898=CARTESIAN_POINT('Ctrl Pts',(-2.69621932864301,-1.,-2.92733294395267));
#46899=CARTESIAN_POINT('Ctrl Pts',(-2.69621932864301,1.,-2.92733294395267));
#46900=CARTESIAN_POINT('Ctrl Pts',(-2.70292247416885,-1.,-2.93089438233749));
#46901=CARTESIAN_POINT('Ctrl Pts',(-2.70292247416885,1.,-2.93089438233749));
#46902=CARTESIAN_POINT('Ctrl Pts',(-2.70965695523787,-1.,-2.93442516311179));
#46903=CARTESIAN_POINT('Ctrl Pts',(-2.70965695523787,1.,-2.93442516311179));
#46904=CARTESIAN_POINT('Ctrl Pts',(-2.71642190053592,-1.,-2.93792519474972));
#46905=CARTESIAN_POINT('Ctrl Pts',(-2.71642190053592,1.,-2.93792519474972));
#46906=CARTESIAN_POINT('Ctrl Pts',(-2.72321571511337,-1.,-2.94139351933897));
#46907=CARTESIAN_POINT('Ctrl Pts',(-2.72321571511337,1.,-2.94139351933897));
#46908=CARTESIAN_POINT('Ctrl Pts',(-2.73003657371617,-1.,-2.94482887675143));
#46909=CARTESIAN_POINT('Ctrl Pts',(-2.73003657371617,1.,-2.94482887675143));
#46910=CARTESIAN_POINT('Ctrl Pts',(-2.73688288329808,-1.,-2.94823023414364));
#46911=CARTESIAN_POINT('Ctrl Pts',(-2.73688288329808,1.,-2.94823023414364));
#46912=CARTESIAN_POINT('Ctrl Pts',(-2.74375379492172,-1.,-2.95159737214266));
#46913=CARTESIAN_POINT('Ctrl Pts',(-2.74375379492172,1.,-2.95159737214266));
#46914=CARTESIAN_POINT('Ctrl Pts',(-2.75064903318947,-1.,-2.95493069316161));
#46915=CARTESIAN_POINT('Ctrl Pts',(-2.75064903318947,1.,-2.95493069316161));
#46916=CARTESIAN_POINT('Ctrl Pts',(-2.7575686788835,-1.,-2.95823097665896));
#46917=CARTESIAN_POINT('Ctrl Pts',(-2.7575686788835,1.,-2.95823097665896));
#46918=CARTESIAN_POINT('Ctrl Pts',(-2.76451296269557,-1.,-2.96149914764818));
#46919=CARTESIAN_POINT('Ctrl Pts',(-2.76451296269557,1.,-2.96149914764818));
#46920=CARTESIAN_POINT('Ctrl Pts',(-2.77148206836498,-1.,-2.96473605585583));
#46921=CARTESIAN_POINT('Ctrl Pts',(-2.77148206836498,1.,-2.96473605585583));
#46922=CARTESIAN_POINT('Ctrl Pts',(-2.7784758954285,-1.,-2.96794221043036));
#46923=CARTESIAN_POINT('Ctrl Pts',(-2.7784758954285,1.,-2.96794221043036));
#46924=CARTESIAN_POINT('Ctrl Pts',(-2.78549409123769,-1.,-2.97111781461465));
#46925=CARTESIAN_POINT('Ctrl Pts',(-2.78549409123769,1.,-2.97111781461465));
#46926=CARTESIAN_POINT('Ctrl Pts',(-2.79253615718248,-1.,-2.9742628834758));
#46927=CARTESIAN_POINT('Ctrl Pts',(-2.79253615718248,1.,-2.9742628834758));
#46928=CARTESIAN_POINT('Ctrl Pts',(-2.7996015327823,-1.,-2.97737733718287));
#46929=CARTESIAN_POINT('Ctrl Pts',(-2.7996015327823,1.,-2.97737733718287));
#46930=CARTESIAN_POINT('Ctrl Pts',(-2.80668968101106,-1.,-2.98046109647241));
#46931=CARTESIAN_POINT('Ctrl Pts',(-2.80668968101106,1.,-2.98046109647241));
#46932=CARTESIAN_POINT('Ctrl Pts',(-2.81380019196286,-1.,-2.98351419779767));
#46933=CARTESIAN_POINT('Ctrl Pts',(-2.81380019196286,1.,-2.98351419779767));
#46934=CARTESIAN_POINT('Ctrl Pts',(-2.82093279065457,-1.,-2.9865368066918));
#46935=CARTESIAN_POINT('Ctrl Pts',(-2.82093279065457,1.,-2.9865368066918));
#46936=CARTESIAN_POINT('Ctrl Pts',(-2.82808728190157,-1.,-2.98952916401446));
#46937=CARTESIAN_POINT('Ctrl Pts',(-2.82808728190157,1.,-2.98952916401446));
#46938=CARTESIAN_POINT('Ctrl Pts',(-2.83526351254248,-1.,-2.99249155170339));
#46939=CARTESIAN_POINT('Ctrl Pts',(-2.83526351254248,1.,-2.99249155170339));
#46940=CARTESIAN_POINT('Ctrl Pts',(-2.84246132984415,-1.,-2.99542425341685));
#46941=CARTESIAN_POINT('Ctrl Pts',(-2.84246132984415,1.,-2.99542425341685));
#46942=CARTESIAN_POINT('Ctrl Pts',(-2.84968053289451,-1.,-2.99832751144925));
#46943=CARTESIAN_POINT('Ctrl Pts',(-2.84968053289451,1.,-2.99832751144925));
#46944=CARTESIAN_POINT('Ctrl Pts',(-2.85692085715686,-1.,-3.00120150796095));
#46945=CARTESIAN_POINT('Ctrl Pts',(-2.85692085715686,1.,-3.00120150796095));
#46946=CARTESIAN_POINT('Ctrl Pts',(-2.86418200833667,-1.,-3.00404638316867));
#46947=CARTESIAN_POINT('Ctrl Pts',(-2.86418200833667,1.,-3.00404638316867));
#46948=CARTESIAN_POINT('Ctrl Pts',(-2.87146368430502,-1.,-3.00686224485784));
#46949=CARTESIAN_POINT('Ctrl Pts',(-2.87146368430502,1.,-3.00686224485784));
#46950=CARTESIAN_POINT('Ctrl Pts',(-2.87876560072727,-1.,-3.00964918108476));
#46951=CARTESIAN_POINT('Ctrl Pts',(-2.87876560072727,1.,-3.00964918108476));
#46952=CARTESIAN_POINT('Ctrl Pts',(-2.8860875170608,-1.,-3.01240727308829));
#46953=CARTESIAN_POINT('Ctrl Pts',(-2.8860875170608,1.,-3.01240727308829));
#46954=CARTESIAN_POINT('Ctrl Pts',(-2.89342925566321,-1.,-3.01513660431928));
#46955=CARTESIAN_POINT('Ctrl Pts',(-2.89342925566321,1.,-3.01513660431928));
#46956=CARTESIAN_POINT('Ctrl Pts',(-2.9007906910105,-1.,-3.01783725121981));
#46957=CARTESIAN_POINT('Ctrl Pts',(-2.9007906910105,1.,-3.01783725121981));
#46958=CARTESIAN_POINT('Ctrl Pts',(-2.90669553302526,-1.,-3.01997487193503));
#46959=CARTESIAN_POINT('Ctrl Pts',(-2.90669553302526,1.,-3.01997487193503));
#46960=CARTESIAN_POINT('Ctrl Pts',(-2.91113297348212,-1.,-3.02156522742431));
#46961=CARTESIAN_POINT('Ctrl Pts',(-2.91113297348212,1.,-3.02156522742431));
#46962=CARTESIAN_POINT('Ctrl Pts',(-2.91409518070399,-1.,-3.02261975104593));
#46963=CARTESIAN_POINT('Ctrl Pts',(-2.91409518070399,1.,-3.02261975104593));
#46964=CARTESIAN_POINT('Ctrl Pts',(-2.91557726271063,-1.,-3.02314558451372));
#46965=CARTESIAN_POINT('Ctrl Pts',(-2.91557726271063,1.,-3.02314558451372));
#46966=CARTESIAN_POINT('',(-2.50410331873176,1.,-2.79140942341258));
#46967=CARTESIAN_POINT('Ctrl Pts',(-2.50410331873176,-1.,-2.79140942341258));
#46968=CARTESIAN_POINT('Ctrl Pts',(-2.50410331873176,-0.666666666666667,
-2.79140942341258));
#46969=CARTESIAN_POINT('Ctrl Pts',(-2.50410331873176,-0.333333333333333,
-2.79140942341258));
#46970=CARTESIAN_POINT('Ctrl Pts',(-2.50410331873176,0.333333333333333,
-2.79140942341258));
#46971=CARTESIAN_POINT('Ctrl Pts',(-2.50410331873176,0.666666666666667,
-2.79140942341258));
#46972=CARTESIAN_POINT('Ctrl Pts',(-2.50410331873176,1.,-2.79140942341258));
#46973=CARTESIAN_POINT('',(-2.91557726271063,1.,-3.02314558451372));
#46974=CARTESIAN_POINT('',(-2.91557726271063,0.,-3.02314558451372));
#46975=CARTESIAN_POINT('Ctrl Pts',(-2.50410331873176,1.,-2.79140942341258));
#46976=CARTESIAN_POINT('Ctrl Pts',(-2.50410700351493,1.,-2.79145823440781));
#46977=CARTESIAN_POINT('Ctrl Pts',(-2.50417932839313,1.,-2.79164172518905));
#46978=CARTESIAN_POINT('Ctrl Pts',(-2.50455968395146,1.,-2.79217568804755));
#46979=CARTESIAN_POINT('Ctrl Pts',(-2.50567182569081,1.,-2.79344192164147));
#46980=CARTESIAN_POINT('Ctrl Pts',(-2.50810555977671,1.,-2.79596878057287));
#46981=CARTESIAN_POINT('Ctrl Pts',(-2.51186983687818,1.,-2.79970585014168));
#46982=CARTESIAN_POINT('Ctrl Pts',(-2.51660190465805,1.,-2.80427363984653));
#46983=CARTESIAN_POINT('Ctrl Pts',(-2.52205778589653,1.,-2.80941521966941));
#46984=CARTESIAN_POINT('Ctrl Pts',(-2.52796388055278,1.,-2.81484379048475));
#46985=CARTESIAN_POINT('Ctrl Pts',(-2.53405679667412,1.,-2.82028550483689));
#46986=CARTESIAN_POINT('Ctrl Pts',(-2.54012272520199,1.,-2.8255216764922));
#46987=CARTESIAN_POINT('Ctrl Pts',(-2.54604736792655,1.,-2.83044254225917));
#46988=CARTESIAN_POINT('Ctrl Pts',(-2.55182152807077,1.,-2.83505269592536));
#46989=CARTESIAN_POINT('Ctrl Pts',(-2.55749952145241,1.,-2.83942515220782));
#46990=CARTESIAN_POINT('Ctrl Pts',(-2.56316920798513,1.,-2.84366802680237));
#46991=CARTESIAN_POINT('Ctrl Pts',(-2.56891984251721,1.,-2.84788893329067));
#46992=CARTESIAN_POINT('Ctrl Pts',(-2.57480482727081,1.,-2.85215360144431));
#46993=CARTESIAN_POINT('Ctrl Pts',(-2.58082875254357,1.,-2.85647171715092));
#46994=CARTESIAN_POINT('Ctrl Pts',(-2.58696770643524,1.,-2.86081999003629));
#46995=CARTESIAN_POINT('Ctrl Pts',(-2.59318160184908,1.,-2.86515629953513));
#46996=CARTESIAN_POINT('Ctrl Pts',(-2.5994287522321,1.,-2.86943633170722));
#46997=CARTESIAN_POINT('Ctrl Pts',(-2.60568177881303,1.,-2.87363176656501));
#46998=CARTESIAN_POINT('Ctrl Pts',(-2.61193507170955,1.,-2.87773881947915));
#46999=CARTESIAN_POINT('Ctrl Pts',(-2.61819596473108,1.,-2.88176821427525));
#47000=CARTESIAN_POINT('Ctrl Pts',(-2.62447947640262,1.,-2.88573922195059));
#47001=CARTESIAN_POINT('Ctrl Pts',(-2.63080195420767,1.,-2.88967244854239));
#47002=CARTESIAN_POINT('Ctrl Pts',(-2.63717442263932,1.,-2.89358228854544));
#47003=CARTESIAN_POINT('Ctrl Pts',(-2.64359851684131,1.,-2.89747231723345));
#47004=CARTESIAN_POINT('Ctrl Pts',(-2.65007017365564,1.,-2.90133950224867));
#47005=CARTESIAN_POINT('Ctrl Pts',(-2.65658188464282,1.,-2.90517678087461));
#47006=CARTESIAN_POINT('Ctrl Pts',(-2.6631254261681,1.,-2.90897617968923));
#47007=CARTESIAN_POINT('Ctrl Pts',(-2.66969458792631,1.,-2.91273193382882));
#47008=CARTESIAN_POINT('Ctrl Pts',(-2.67628728855312,1.,-2.91644290704285));
#47009=CARTESIAN_POINT('Ctrl Pts',(-2.68290409279688,1.,-2.92011090722152));
#47010=CARTESIAN_POINT('Ctrl Pts',(-2.68954721165339,1.,-2.92373955325875));
#47011=CARTESIAN_POINT('Ctrl Pts',(-2.69621932864301,1.,-2.92733294395267));
#47012=CARTESIAN_POINT('Ctrl Pts',(-2.70292247416885,1.,-2.93089438233749));
#47013=CARTESIAN_POINT('Ctrl Pts',(-2.70965695523787,1.,-2.93442516311179));
#47014=CARTESIAN_POINT('Ctrl Pts',(-2.71642190053592,1.,-2.93792519474972));
#47015=CARTESIAN_POINT('Ctrl Pts',(-2.72321571511337,1.,-2.94139351933897));
#47016=CARTESIAN_POINT('Ctrl Pts',(-2.73003657371617,1.,-2.94482887675143));
#47017=CARTESIAN_POINT('Ctrl Pts',(-2.73688288329808,1.,-2.94823023414364));
#47018=CARTESIAN_POINT('Ctrl Pts',(-2.74375379492172,1.,-2.95159737214266));
#47019=CARTESIAN_POINT('Ctrl Pts',(-2.75064903318947,1.,-2.95493069316161));
#47020=CARTESIAN_POINT('Ctrl Pts',(-2.7575686788835,1.,-2.95823097665896));
#47021=CARTESIAN_POINT('Ctrl Pts',(-2.76451296269557,1.,-2.96149914764818));
#47022=CARTESIAN_POINT('Ctrl Pts',(-2.77148206836498,1.,-2.96473605585583));
#47023=CARTESIAN_POINT('Ctrl Pts',(-2.7784758954285,1.,-2.96794221043036));
#47024=CARTESIAN_POINT('Ctrl Pts',(-2.78549409123769,1.,-2.97111781461465));
#47025=CARTESIAN_POINT('Ctrl Pts',(-2.79253615718248,1.,-2.9742628834758));
#47026=CARTESIAN_POINT('Ctrl Pts',(-2.7996015327823,1.,-2.97737733718287));
#47027=CARTESIAN_POINT('Ctrl Pts',(-2.80668968101106,1.,-2.98046109647241));
#47028=CARTESIAN_POINT('Ctrl Pts',(-2.81380019196286,1.,-2.98351419779767));
#47029=CARTESIAN_POINT('Ctrl Pts',(-2.82093279065457,1.,-2.9865368066918));
#47030=CARTESIAN_POINT('Ctrl Pts',(-2.82808728190157,1.,-2.98952916401446));
#47031=CARTESIAN_POINT('Ctrl Pts',(-2.83526351254248,1.,-2.99249155170339));
#47032=CARTESIAN_POINT('Ctrl Pts',(-2.84246132984415,1.,-2.99542425341685));
#47033=CARTESIAN_POINT('Ctrl Pts',(-2.84968053289451,1.,-2.99832751144925));
#47034=CARTESIAN_POINT('Ctrl Pts',(-2.85692085715686,1.,-3.00120150796095));
#47035=CARTESIAN_POINT('Ctrl Pts',(-2.86418200833667,1.,-3.00404638316867));
#47036=CARTESIAN_POINT('Ctrl Pts',(-2.87146368430502,1.,-3.00686224485784));
#47037=CARTESIAN_POINT('Ctrl Pts',(-2.87876560072727,1.,-3.00964918108476));
#47038=CARTESIAN_POINT('Ctrl Pts',(-2.8860875170608,1.,-3.01240727308829));
#47039=CARTESIAN_POINT('Ctrl Pts',(-2.89342925566321,1.,-3.01513660431928));
#47040=CARTESIAN_POINT('Ctrl Pts',(-2.9007906910105,1.,-3.01783725121981));
#47041=CARTESIAN_POINT('Ctrl Pts',(-2.90669553302526,1.,-3.01997487193503));
#47042=CARTESIAN_POINT('Ctrl Pts',(-2.91113297348212,1.,-3.02156522742431));
#47043=CARTESIAN_POINT('Ctrl Pts',(-2.91409518070399,1.,-3.02261975104593));
#47044=CARTESIAN_POINT('Ctrl Pts',(-2.91557726271063,1.,-3.02314558451372));
#47045=CARTESIAN_POINT('Origin',(-2.91557726271063,0.,-3.02314558451372));
#47046=CARTESIAN_POINT('',(-3.02314558451372,1.,-2.91557726271063));
#47047=CARTESIAN_POINT('Origin',(0.,0.,0.));
#47048=CARTESIAN_POINT('',(-2.36531447826213,1.,-2.90994629141562));
#47049=CARTESIAN_POINT('Origin',(0.,1.,0.));
#47050=CARTESIAN_POINT('Ctrl Pts',(-2.36531447826213,1.,-2.90994629141562));
#47051=CARTESIAN_POINT('Ctrl Pts',(-2.36531447826213,0.666666666666667,
-2.90994629141562));
#47052=CARTESIAN_POINT('Ctrl Pts',(-2.36531447826213,0.333333333333333,
-2.90994629141562));
#47053=CARTESIAN_POINT('Ctrl Pts',(-2.36531447826213,-0.333333333333333,
-2.90994629141562));
#47054=CARTESIAN_POINT('Ctrl Pts',(-2.36531447826213,-0.666666666666667,
-2.90994629141562));
#47055=CARTESIAN_POINT('Ctrl Pts',(-2.36531447826213,-1.,-2.90994629141562));
#47056=CARTESIAN_POINT('Ctrl Pts',(-2.52982887637028,-1.,-3.35260583073571));
#47057=CARTESIAN_POINT('Ctrl Pts',(-2.52982887637028,1.,-3.35260583073571));
#47058=CARTESIAN_POINT('Ctrl Pts',(-2.52954136549357,-1.,-3.35105973714426));
#47059=CARTESIAN_POINT('Ctrl Pts',(-2.52954136549357,1.,-3.35105973714426));
#47060=CARTESIAN_POINT('Ctrl Pts',(-2.5289632161143,-1.,-3.34796903577628));
#47061=CARTESIAN_POINT('Ctrl Pts',(-2.5289632161143,1.,-3.34796903577628));
#47062=CARTESIAN_POINT('Ctrl Pts',(-2.52808660916879,-1.,-3.34333744117093));
#47063=CARTESIAN_POINT('Ctrl Pts',(-2.52808660916879,1.,-3.34333744117093));
#47064=CARTESIAN_POINT('Ctrl Pts',(-2.52689902691551,-1.,-3.33717090000955));
#47065=CARTESIAN_POINT('Ctrl Pts',(-2.52689902691551,1.,-3.33717090000955));
#47066=CARTESIAN_POINT('Ctrl Pts',(-2.52538321165774,-1.,-3.32947762189049));
#47067=CARTESIAN_POINT('Ctrl Pts',(-2.52538321165774,1.,-3.32947762189049));
#47068=CARTESIAN_POINT('Ctrl Pts',(-2.52383598396878,-1.,-3.32179931079521));
#47069=CARTESIAN_POINT('Ctrl Pts',(-2.52383598396878,1.,-3.32179931079521));
#47070=CARTESIAN_POINT('Ctrl Pts',(-2.52225724871375,-1.,-3.31413607874727));
#47071=CARTESIAN_POINT('Ctrl Pts',(-2.52225724871375,1.,-3.31413607874727));
#47072=CARTESIAN_POINT('Ctrl Pts',(-2.52064689568167,-1.,-3.30648808814986));
#47073=CARTESIAN_POINT('Ctrl Pts',(-2.52064689568167,1.,-3.30648808814986));
#47074=CARTESIAN_POINT('Ctrl Pts',(-2.51900480700548,-1.,-3.29885556387661));
#47075=CARTESIAN_POINT('Ctrl Pts',(-2.51900480700548,1.,-3.29885556387661));
#47076=CARTESIAN_POINT('Ctrl Pts',(-2.51733085123316,-1.,-3.2912387729863));
#47077=CARTESIAN_POINT('Ctrl Pts',(-2.51733085123316,1.,-3.2912387729863));
#47078=CARTESIAN_POINT('Ctrl Pts',(-2.51562487464215,-1.,-3.28363799702583));
#47079=CARTESIAN_POINT('Ctrl Pts',(-2.51562487464215,1.,-3.28363799702583));
#47080=CARTESIAN_POINT('Ctrl Pts',(-2.51388669270329,-1.,-3.27605350473048));
#47081=CARTESIAN_POINT('Ctrl Pts',(-2.51388669270329,1.,-3.27605350473048));
#47082=CARTESIAN_POINT('Ctrl Pts',(-2.51211608411539,-1.,-3.26848552888271));
#47083=CARTESIAN_POINT('Ctrl Pts',(-2.51211608411539,1.,-3.26848552888271));
#47084=CARTESIAN_POINT('Ctrl Pts',(-2.51031277813697,-1.,-3.26093423001716));
#47085=CARTESIAN_POINT('Ctrl Pts',(-2.51031277813697,1.,-3.26093423001716));
#47086=CARTESIAN_POINT('Ctrl Pts',(-2.50847647070936,-1.,-3.25339971461265));
#47087=CARTESIAN_POINT('Ctrl Pts',(-2.50847647070936,1.,-3.25339971461265));
#47088=CARTESIAN_POINT('Ctrl Pts',(-2.50660685940645,-1.,-3.24588208984042));
#47089=CARTESIAN_POINT('Ctrl Pts',(-2.50660685940645,1.,-3.24588208984042));
#47090=CARTESIAN_POINT('Ctrl Pts',(-2.50470367580078,-1.,-3.23838151080383));
#47091=CARTESIAN_POINT('Ctrl Pts',(-2.50470367580078,1.,-3.23838151080383));
#47092=CARTESIAN_POINT('Ctrl Pts',(-2.50276671338074,-1.,-3.23089822320596));
#47093=CARTESIAN_POINT('Ctrl Pts',(-2.50276671338074,1.,-3.23089822320596));
#47094=CARTESIAN_POINT('Ctrl Pts',(-2.5007958720187,-1.,-3.22343262620387));
#47095=CARTESIAN_POINT('Ctrl Pts',(-2.5007958720187,1.,-3.22343262620387));
#47096=CARTESIAN_POINT('Ctrl Pts',(-2.49879114599293,-1.,-3.21598526261157));
#47097=CARTESIAN_POINT('Ctrl Pts',(-2.49879114599293,1.,-3.21598526261157));
#47098=CARTESIAN_POINT('Ctrl Pts',(-2.49675252647298,-1.,-3.2085566984974));
#47099=CARTESIAN_POINT('Ctrl Pts',(-2.49675252647298,1.,-3.2085566984974));
#47100=CARTESIAN_POINT('Ctrl Pts',(-2.49467992057726,-1.,-3.20114742397549));
#47101=CARTESIAN_POINT('Ctrl Pts',(-2.49467992057726,1.,-3.20114742397549));
#47102=CARTESIAN_POINT('Ctrl Pts',(-2.4925730723986,-1.,-3.19375775555814));
#47103=CARTESIAN_POINT('Ctrl Pts',(-2.4925730723986,1.,-3.19375775555814));
#47104=CARTESIAN_POINT('Ctrl Pts',(-2.49043146334095,-1.,-3.18638771282315));
#47105=CARTESIAN_POINT('Ctrl Pts',(-2.49043146334095,1.,-3.18638771282315));
#47106=CARTESIAN_POINT('Ctrl Pts',(-2.48825428288243,-1.,-3.17903698136679));
#47107=CARTESIAN_POINT('Ctrl Pts',(-2.48825428288243,1.,-3.17903698136679));
#47108=CARTESIAN_POINT('Ctrl Pts',(-2.48604065348619,-1.,-3.17170518863357));
#47109=CARTESIAN_POINT('Ctrl Pts',(-2.48604065348619,1.,-3.17170518863357));
#47110=CARTESIAN_POINT('Ctrl Pts',(-2.48378981792739,-1.,-3.16439213290181));
#47111=CARTESIAN_POINT('Ctrl Pts',(-2.48378981792739,1.,-3.16439213290181));
#47112=CARTESIAN_POINT('Ctrl Pts',(-2.48150133566568,-1.,-3.15709802322735));
#47113=CARTESIAN_POINT('Ctrl Pts',(-2.48150133566568,1.,-3.15709802322735));
#47114=CARTESIAN_POINT('Ctrl Pts',(-2.47917529057016,-1.,-3.14982373241335));
#47115=CARTESIAN_POINT('Ctrl Pts',(-2.47917529057016,1.,-3.14982373241335));
#47116=CARTESIAN_POINT('Ctrl Pts',(-2.47681245356095,-1.,-3.14257099546531));
#47117=CARTESIAN_POINT('Ctrl Pts',(-2.47681245356095,1.,-3.14257099546531));
#47118=CARTESIAN_POINT('Ctrl Pts',(-2.47441378371923,-1.,-3.13534181229282));
#47119=CARTESIAN_POINT('Ctrl Pts',(-2.47441378371923,1.,-3.13534181229282));
#47120=CARTESIAN_POINT('Ctrl Pts',(-2.47197997765868,-1.,-3.12813790805948));
#47121=CARTESIAN_POINT('Ctrl Pts',(-2.47197997765868,1.,-3.12813790805948));
#47122=CARTESIAN_POINT('Ctrl Pts',(-2.4695109894747,-1.,-3.12096015766984));
#47123=CARTESIAN_POINT('Ctrl Pts',(-2.4695109894747,1.,-3.12096015766984));
#47124=CARTESIAN_POINT('Ctrl Pts',(-2.46700558843507,-1.,-3.11380805536124));
#47125=CARTESIAN_POINT('Ctrl Pts',(-2.46700558843507,1.,-3.11380805536124));
#47126=CARTESIAN_POINT('Ctrl Pts',(-2.46446082979645,-1.,-3.10667907901981));
#47127=CARTESIAN_POINT('Ctrl Pts',(-2.46446082979645,1.,-3.10667907901981));
#47128=CARTESIAN_POINT('Ctrl Pts',(-2.4618730850188,-1.,-3.09956993697048));
#47129=CARTESIAN_POINT('Ctrl Pts',(-2.4618730850188,1.,-3.09956993697048));
#47130=CARTESIAN_POINT('Ctrl Pts',(-2.45923912563875,-1.,-3.09247787931881));
#47131=CARTESIAN_POINT('Ctrl Pts',(-2.45923912563875,1.,-3.09247787931881));
#47132=CARTESIAN_POINT('Ctrl Pts',(-2.45655725437037,-1.,-3.08540206545313));
#47133=CARTESIAN_POINT('Ctrl Pts',(-2.45655725437037,1.,-3.08540206545313));
#47134=CARTESIAN_POINT('Ctrl Pts',(-2.45382826787795,-1.,-3.07834472886145));
#47135=CARTESIAN_POINT('Ctrl Pts',(-2.45382826787795,1.,-3.07834472886145));
#47136=CARTESIAN_POINT('Ctrl Pts',(-2.45105688854432,-1.,-3.0713129052131));
#47137=CARTESIAN_POINT('Ctrl Pts',(-2.45105688854432,1.,-3.0713129052131));
#47138=CARTESIAN_POINT('Ctrl Pts',(-2.44824970516558,-1.,-3.06431596421422));
#47139=CARTESIAN_POINT('Ctrl Pts',(-2.44824970516558,1.,-3.06431596421422));
#47140=CARTESIAN_POINT('Ctrl Pts',(-2.44541251892568,-1.,-3.05736242671521));
#47141=CARTESIAN_POINT('Ctrl Pts',(-2.44541251892568,1.,-3.05736242671521));
#47142=CARTESIAN_POINT('Ctrl Pts',(-2.44254768923109,-1.,-3.05045678021509));
#47143=CARTESIAN_POINT('Ctrl Pts',(-2.44254768923109,1.,-3.05045678021509));
#47144=CARTESIAN_POINT('Ctrl Pts',(-2.43965194061849,-1.,-3.04359685040545));
#47145=CARTESIAN_POINT('Ctrl Pts',(-2.43965194061849,1.,-3.04359685040545));
#47146=CARTESIAN_POINT('Ctrl Pts',(-2.43671278042394,-1.,-3.03676949672797));
#47147=CARTESIAN_POINT('Ctrl Pts',(-2.43671278042394,1.,-3.03676949672797));
#47148=CARTESIAN_POINT('Ctrl Pts',(-2.43371241361462,-1.,-3.02995534946946));
#47149=CARTESIAN_POINT('Ctrl Pts',(-2.43371241361462,1.,-3.02995534946946));
#47150=CARTESIAN_POINT('Ctrl Pts',(-2.43063415586615,-1.,-3.02313656035977));
#47151=CARTESIAN_POINT('Ctrl Pts',(-2.43063415586615,1.,-3.02313656035977));
#47152=CARTESIAN_POINT('Ctrl Pts',(-2.4274685626416,-1.,-3.01630420830494));
#47153=CARTESIAN_POINT('Ctrl Pts',(-2.4274685626416,1.,-3.01630420830494));
#47154=CARTESIAN_POINT('Ctrl Pts',(-2.42421849439625,-1.,-3.00946442616674));
#47155=CARTESIAN_POINT('Ctrl Pts',(-2.42421849439625,1.,-3.00946442616674));
#47156=CARTESIAN_POINT('Ctrl Pts',(-2.42090763946812,-1.,-3.00264868586038));
#47157=CARTESIAN_POINT('Ctrl Pts',(-2.42090763946812,1.,-3.00264868586038));
#47158=CARTESIAN_POINT('Ctrl Pts',(-2.4175732450056,-1.,-2.99590509293561));
#47159=CARTESIAN_POINT('Ctrl Pts',(-2.4175732450056,1.,-2.99590509293561));
#47160=CARTESIAN_POINT('Ctrl Pts',(-2.4142506419963,-1.,-2.98927983005851));
#47161=CARTESIAN_POINT('Ctrl Pts',(-2.4142506419963,1.,-2.98927983005851));
#47162=CARTESIAN_POINT('Ctrl Pts',(-2.41095909342591,-1.,-2.98280015815132));
#47163=CARTESIAN_POINT('Ctrl Pts',(-2.41095909342591,1.,-2.98280015815132));
#47164=CARTESIAN_POINT('Ctrl Pts',(-2.40768975073691,-1.,-2.97646002822395));
#47165=CARTESIAN_POINT('Ctrl Pts',(-2.40768975073691,1.,-2.97646002822395));
#47166=CARTESIAN_POINT('Ctrl Pts',(-2.40438604734848,-1.,-2.97019641312272));
#47167=CARTESIAN_POINT('Ctrl Pts',(-2.40438604734848,1.,-2.97019641312272));
#47168=CARTESIAN_POINT('Ctrl Pts',(-2.40095565711535,-1.,-2.96390432240181));
#47169=CARTESIAN_POINT('Ctrl Pts',(-2.40095565711535,1.,-2.96390432240181));
#47170=CARTESIAN_POINT('Ctrl Pts',(-2.39730553974412,-1.,-2.95748006482811));
#47171=CARTESIAN_POINT('Ctrl Pts',(-2.39730553974412,1.,-2.95748006482811));
#47172=CARTESIAN_POINT('Ctrl Pts',(-2.39337207631613,-1.,-2.95085857128372));
#47173=CARTESIAN_POINT('Ctrl Pts',(-2.39337207631613,1.,-2.95085857128372));
#47174=CARTESIAN_POINT('Ctrl Pts',(-2.38914929090806,-1.,-2.94404820669135));
#47175=CARTESIAN_POINT('Ctrl Pts',(-2.38914929090806,1.,-2.94404820669135));
#47176=CARTESIAN_POINT('Ctrl Pts',(-2.38472771516476,-1.,-2.93717903280599));
#47177=CARTESIAN_POINT('Ctrl Pts',(-2.38472771516476,1.,-2.93717903280599));
#47178=CARTESIAN_POINT('Ctrl Pts',(-2.3802898958232,-1.,-2.93049643640517));
#47179=CARTESIAN_POINT('Ctrl Pts',(-2.3802898958232,1.,-2.93049643640517));
#47180=CARTESIAN_POINT('Ctrl Pts',(-2.37606510524271,-1.,-2.92430340582912));
#47181=CARTESIAN_POINT('Ctrl Pts',(-2.37606510524271,1.,-2.92430340582912));
#47182=CARTESIAN_POINT('Ctrl Pts',(-2.37229381109939,-1.,-2.9189150379156));
#47183=CARTESIAN_POINT('Ctrl Pts',(-2.37229381109939,1.,-2.9189150379156));
#47184=CARTESIAN_POINT('Ctrl Pts',(-2.36919161373074,-1.,-2.91461249883016));
#47185=CARTESIAN_POINT('Ctrl Pts',(-2.36919161373074,1.,-2.91461249883016));
#47186=CARTESIAN_POINT('Ctrl Pts',(-2.36690501170317,-1.,-2.9115863784165));
#47187=CARTESIAN_POINT('Ctrl Pts',(-2.36690501170317,1.,-2.9115863784165));
#47188=CARTESIAN_POINT('Ctrl Pts',(-2.36578327194396,-1.,-2.91025813829606));
#47189=CARTESIAN_POINT('Ctrl Pts',(-2.36578327194396,1.,-2.91025813829606));
#47190=CARTESIAN_POINT('Ctrl Pts',(-2.36535052956704,-1.,-2.90989022547738));
#47191=CARTESIAN_POINT('Ctrl Pts',(-2.36535052956704,1.,-2.90989022547738));
#47192=CARTESIAN_POINT('Ctrl Pts',(-2.36524348105023,-1.,-2.90992398626098));
#47193=CARTESIAN_POINT('Ctrl Pts',(-2.36524348105023,1.,-2.90992398626098));
#47194=CARTESIAN_POINT('Ctrl Pts',(-2.36523532225181,-1.,-2.91001063062876));
#47195=CARTESIAN_POINT('Ctrl Pts',(-2.36523532225181,1.,-2.91001063062876));
#47196=CARTESIAN_POINT('',(-2.52982887637028,1.,-3.35260583073571));
#47197=CARTESIAN_POINT('Ctrl Pts',(-2.52982887637028,1.,-3.35260583073571));
#47198=CARTESIAN_POINT('Ctrl Pts',(-2.52954136549357,1.,-3.35105973714426));
#47199=CARTESIAN_POINT('Ctrl Pts',(-2.5289632161143,1.,-3.34796903577628));
#47200=CARTESIAN_POINT('Ctrl Pts',(-2.52808660916879,1.,-3.34333744117093));
#47201=CARTESIAN_POINT('Ctrl Pts',(-2.52689902691551,1.,-3.33717090000955));
#47202=CARTESIAN_POINT('Ctrl Pts',(-2.52538321165774,1.,-3.32947762189049));
#47203=CARTESIAN_POINT('Ctrl Pts',(-2.52383598396878,1.,-3.32179931079521));
#47204=CARTESIAN_POINT('Ctrl Pts',(-2.52225724871375,1.,-3.31413607874727));
#47205=CARTESIAN_POINT('Ctrl Pts',(-2.52064689568167,1.,-3.30648808814986));
#47206=CARTESIAN_POINT('Ctrl Pts',(-2.51900480700548,1.,-3.29885556387661));
#47207=CARTESIAN_POINT('Ctrl Pts',(-2.51733085123316,1.,-3.2912387729863));
#47208=CARTESIAN_POINT('Ctrl Pts',(-2.51562487464215,1.,-3.28363799702583));
#47209=CARTESIAN_POINT('Ctrl Pts',(-2.51388669270329,1.,-3.27605350473048));
#47210=CARTESIAN_POINT('Ctrl Pts',(-2.51211608411539,1.,-3.26848552888271));
#47211=CARTESIAN_POINT('Ctrl Pts',(-2.51031277813697,1.,-3.26093423001716));
#47212=CARTESIAN_POINT('Ctrl Pts',(-2.50847647070936,1.,-3.25339971461265));
#47213=CARTESIAN_POINT('Ctrl Pts',(-2.50660685940645,1.,-3.24588208984042));
#47214=CARTESIAN_POINT('Ctrl Pts',(-2.50470367580078,1.,-3.23838151080383));
#47215=CARTESIAN_POINT('Ctrl Pts',(-2.50276671338074,1.,-3.23089822320596));
#47216=CARTESIAN_POINT('Ctrl Pts',(-2.5007958720187,1.,-3.22343262620387));
#47217=CARTESIAN_POINT('Ctrl Pts',(-2.49879114599293,1.,-3.21598526261157));
#47218=CARTESIAN_POINT('Ctrl Pts',(-2.49675252647298,1.,-3.2085566984974));
#47219=CARTESIAN_POINT('Ctrl Pts',(-2.49467992057726,1.,-3.20114742397549));
#47220=CARTESIAN_POINT('Ctrl Pts',(-2.4925730723986,1.,-3.19375775555814));
#47221=CARTESIAN_POINT('Ctrl Pts',(-2.49043146334095,1.,-3.18638771282315));
#47222=CARTESIAN_POINT('Ctrl Pts',(-2.48825428288243,1.,-3.17903698136679));
#47223=CARTESIAN_POINT('Ctrl Pts',(-2.48604065348619,1.,-3.17170518863357));
#47224=CARTESIAN_POINT('Ctrl Pts',(-2.48378981792739,1.,-3.16439213290181));
#47225=CARTESIAN_POINT('Ctrl Pts',(-2.48150133566568,1.,-3.15709802322735));
#47226=CARTESIAN_POINT('Ctrl Pts',(-2.47917529057016,1.,-3.14982373241335));
#47227=CARTESIAN_POINT('Ctrl Pts',(-2.47681245356095,1.,-3.14257099546531));
#47228=CARTESIAN_POINT('Ctrl Pts',(-2.47441378371923,1.,-3.13534181229282));
#47229=CARTESIAN_POINT('Ctrl Pts',(-2.47197997765868,1.,-3.12813790805948));
#47230=CARTESIAN_POINT('Ctrl Pts',(-2.4695109894747,1.,-3.12096015766984));
#47231=CARTESIAN_POINT('Ctrl Pts',(-2.46700558843507,1.,-3.11380805536124));
#47232=CARTESIAN_POINT('Ctrl Pts',(-2.46446082979645,1.,-3.10667907901981));
#47233=CARTESIAN_POINT('Ctrl Pts',(-2.4618730850188,1.,-3.09956993697048));
#47234=CARTESIAN_POINT('Ctrl Pts',(-2.45923912563875,1.,-3.09247787931881));
#47235=CARTESIAN_POINT('Ctrl Pts',(-2.45655725437037,1.,-3.08540206545313));
#47236=CARTESIAN_POINT('Ctrl Pts',(-2.45382826787795,1.,-3.07834472886145));
#47237=CARTESIAN_POINT('Ctrl Pts',(-2.45105688854432,1.,-3.0713129052131));
#47238=CARTESIAN_POINT('Ctrl Pts',(-2.44824970516558,1.,-3.06431596421422));
#47239=CARTESIAN_POINT('Ctrl Pts',(-2.44541251892568,1.,-3.05736242671521));
#47240=CARTESIAN_POINT('Ctrl Pts',(-2.44254768923109,1.,-3.05045678021509));
#47241=CARTESIAN_POINT('Ctrl Pts',(-2.43965194061849,1.,-3.04359685040545));
#47242=CARTESIAN_POINT('Ctrl Pts',(-2.43671278042394,1.,-3.03676949672797));
#47243=CARTESIAN_POINT('Ctrl Pts',(-2.43371241361462,1.,-3.02995534946946));
#47244=CARTESIAN_POINT('Ctrl Pts',(-2.43063415586615,1.,-3.02313656035977));
#47245=CARTESIAN_POINT('Ctrl Pts',(-2.4274685626416,1.,-3.01630420830494));
#47246=CARTESIAN_POINT('Ctrl Pts',(-2.42421849439625,1.,-3.00946442616674));
#47247=CARTESIAN_POINT('Ctrl Pts',(-2.42090763946812,1.,-3.00264868586038));
#47248=CARTESIAN_POINT('Ctrl Pts',(-2.4175732450056,1.,-2.99590509293561));
#47249=CARTESIAN_POINT('Ctrl Pts',(-2.4142506419963,1.,-2.98927983005851));
#47250=CARTESIAN_POINT('Ctrl Pts',(-2.41095909342591,1.,-2.98280015815132));
#47251=CARTESIAN_POINT('Ctrl Pts',(-2.40768975073691,1.,-2.97646002822395));
#47252=CARTESIAN_POINT('Ctrl Pts',(-2.40438604734848,1.,-2.97019641312272));
#47253=CARTESIAN_POINT('Ctrl Pts',(-2.40095565711535,1.,-2.96390432240181));
#47254=CARTESIAN_POINT('Ctrl Pts',(-2.39730553974412,1.,-2.95748006482811));
#47255=CARTESIAN_POINT('Ctrl Pts',(-2.39337207631613,1.,-2.95085857128372));
#47256=CARTESIAN_POINT('Ctrl Pts',(-2.38914929090806,1.,-2.94404820669135));
#47257=CARTESIAN_POINT('Ctrl Pts',(-2.38472771516476,1.,-2.93717903280599));
#47258=CARTESIAN_POINT('Ctrl Pts',(-2.3802898958232,1.,-2.93049643640517));
#47259=CARTESIAN_POINT('Ctrl Pts',(-2.37606510524271,1.,-2.92430340582912));
#47260=CARTESIAN_POINT('Ctrl Pts',(-2.37229381109939,1.,-2.9189150379156));
#47261=CARTESIAN_POINT('Ctrl Pts',(-2.36919161373074,1.,-2.91461249883016));
#47262=CARTESIAN_POINT('Ctrl Pts',(-2.36707658451709,1.,-2.91181344022628));
#47263=CARTESIAN_POINT('Ctrl Pts',(-2.36599991765853,1.,-2.91051690822262));
#47264=CARTESIAN_POINT('Ctrl Pts',(-2.36553202948741,1.,-2.9100577052777));
#47265=CARTESIAN_POINT('Ctrl Pts',(-2.3653621118858,1.,-2.90995756655559));
#47266=CARTESIAN_POINT('Ctrl Pts',(-2.36531447826213,1.,-2.90994629141563));
#47267=CARTESIAN_POINT('',(-2.52982887637028,0.,-3.35260583073571));
#47268=CARTESIAN_POINT('Ctrl Pts',(-2.03668666247593,-1.,-3.1487152044751));
#47269=CARTESIAN_POINT('Ctrl Pts',(-2.03668666247593,1.,-3.1487152044751));
#47270=CARTESIAN_POINT('Ctrl Pts',(-2.03660173757879,-1.,-3.14869618937258));
#47271=CARTESIAN_POINT('Ctrl Pts',(-2.03660173757879,1.,-3.14869618937258));
#47272=CARTESIAN_POINT('Ctrl Pts',(-2.03653654935592,-1.,-3.14878756590812));
#47273=CARTESIAN_POINT('Ctrl Pts',(-2.03653654935592,1.,-3.14878756590812));
#47274=CARTESIAN_POINT('Ctrl Pts',(-2.03675273049189,-1.,-3.14931281968048));
#47275=CARTESIAN_POINT('Ctrl Pts',(-2.03675273049189,1.,-3.14931281968048));
#47276=CARTESIAN_POINT('Ctrl Pts',(-2.03766932526445,-1.,-3.15079010635742));
#47277=CARTESIAN_POINT('Ctrl Pts',(-2.03766932526445,1.,-3.15079010635742));
#47278=CARTESIAN_POINT('Ctrl Pts',(-2.03984073791519,-1.,-3.15389991674792));
#47279=CARTESIAN_POINT('Ctrl Pts',(-2.03984073791519,1.,-3.15389991674792));
#47280=CARTESIAN_POINT('Ctrl Pts',(-2.04297406404027,-1.,-3.15817983946367));
#47281=CARTESIAN_POINT('Ctrl Pts',(-2.04297406404027,1.,-3.15817983946367));
#47282=CARTESIAN_POINT('Ctrl Pts',(-2.04693331247446,-1.,-3.16343165058912));
#47283=CARTESIAN_POINT('Ctrl Pts',(-2.04693331247446,1.,-3.16343165058912));
#47284=CARTESIAN_POINT('Ctrl Pts',(-2.05151770247233,-1.,-3.16936341689527));
#47285=CARTESIAN_POINT('Ctrl Pts',(-2.05151770247233,1.,-3.16936341689527));
#47286=CARTESIAN_POINT('Ctrl Pts',(-2.05650186773132,-1.,-3.17564906975371));
#47287=CARTESIAN_POINT('Ctrl Pts',(-2.05650186773132,1.,-3.17564906975371));
#47288=CARTESIAN_POINT('Ctrl Pts',(-2.06166849827101,-1.,-3.18197692964614));
#47289=CARTESIAN_POINT('Ctrl Pts',(-2.06166849827101,1.,-3.18197692964614));
#47290=CARTESIAN_POINT('Ctrl Pts',(-2.06684062744112,-1.,-3.18809755562368));
#47291=CARTESIAN_POINT('Ctrl Pts',(-2.06684062744112,1.,-3.18809755562368));
#47292=CARTESIAN_POINT('Ctrl Pts',(-2.07192253497857,-1.,-3.19388465568252));
#47293=CARTESIAN_POINT('Ctrl Pts',(-2.07192253497857,1.,-3.19388465568252));
#47294=CARTESIAN_POINT('Ctrl Pts',(-2.07690441870722,-1.,-3.19934132836019));
#47295=CARTESIAN_POINT('Ctrl Pts',(-2.07690441870722,1.,-3.19934132836019));
#47296=CARTESIAN_POINT('Ctrl Pts',(-2.08182850370878,-1.,-3.2045481863073));
#47297=CARTESIAN_POINT('Ctrl Pts',(-2.08182850370878,1.,-3.2045481863073));
#47298=CARTESIAN_POINT('Ctrl Pts',(-2.08676465517455,-1.,-3.20962575845463));
#47299=CARTESIAN_POINT('Ctrl Pts',(-2.08676465517455,1.,-3.20962575845463));
#47300=CARTESIAN_POINT('Ctrl Pts',(-2.09178419460443,-1.,-3.21469429601654));
#47301=CARTESIAN_POINT('Ctrl Pts',(-2.09178419460443,1.,-3.21469429601654));
#47302=CARTESIAN_POINT('Ctrl Pts',(-2.09692958434895,-1.,-3.21982707347009));
#47303=CARTESIAN_POINT('Ctrl Pts',(-2.09692958434895,1.,-3.21982707347009));
#47304=CARTESIAN_POINT('Ctrl Pts',(-2.10220384298492,-1.,-3.22503437553434));
#47305=CARTESIAN_POINT('Ctrl Pts',(-2.10220384298492,1.,-3.22503437553434));
#47306=CARTESIAN_POINT('Ctrl Pts',(-2.10758699642451,-1.,-3.23028945793289));
#47307=CARTESIAN_POINT('Ctrl Pts',(-2.10758699642451,1.,-3.23028945793289));
#47308=CARTESIAN_POINT('Ctrl Pts',(-2.11304604021773,-1.,-3.23554444767099));
#47309=CARTESIAN_POINT('Ctrl Pts',(-2.11304604021773,1.,-3.23554444767099));
#47310=CARTESIAN_POINT('Ctrl Pts',(-2.11854673326979,-1.,-3.24074905517293));
#47311=CARTESIAN_POINT('Ctrl Pts',(-2.11854673326979,1.,-3.24074905517293));
#47312=CARTESIAN_POINT('Ctrl Pts',(-2.12406646410962,-1.,-3.24587102613376));
#47313=CARTESIAN_POINT('Ctrl Pts',(-2.12406646410962,1.,-3.24587102613376));
#47314=CARTESIAN_POINT('Ctrl Pts',(-2.12960028396832,-1.,-3.25090574494028));
#47315=CARTESIAN_POINT('Ctrl Pts',(-2.12960028396832,1.,-3.25090574494028));
#47316=CARTESIAN_POINT('Ctrl Pts',(-2.13515375878803,-1.,-3.25586495065054));
#47317=CARTESIAN_POINT('Ctrl Pts',(-2.13515375878803,1.,-3.25586495065054));
#47318=CARTESIAN_POINT('Ctrl Pts',(-2.14073870754264,-1.,-3.26077002641879));
#47319=CARTESIAN_POINT('Ctrl Pts',(-2.14073870754264,1.,-3.26077002641879));
#47320=CARTESIAN_POINT('Ctrl Pts',(-2.1463680529566,-1.,-3.26564388189759));
#47321=CARTESIAN_POINT('Ctrl Pts',(-2.1463680529566,1.,-3.26564388189759));
#47322=CARTESIAN_POINT('Ctrl Pts',(-2.15205043199808,-1.,-3.27050245897228));
#47323=CARTESIAN_POINT('Ctrl Pts',(-2.15205043199808,1.,-3.27050245897228));
#47324=CARTESIAN_POINT('Ctrl Pts',(-2.15778690038347,-1.,-3.27534954469187));
#47325=CARTESIAN_POINT('Ctrl Pts',(-2.15778690038347,1.,-3.27534954469187));
#47326=CARTESIAN_POINT('Ctrl Pts',(-2.16357391934425,-1.,-3.280181508414));
#47327=CARTESIAN_POINT('Ctrl Pts',(-2.16357391934425,1.,-3.280181508414));
#47328=CARTESIAN_POINT('Ctrl Pts',(-2.16940517773455,-1.,-3.28499019979724));
#47329=CARTESIAN_POINT('Ctrl Pts',(-2.16940517773455,1.,-3.28499019979724));
#47330=CARTESIAN_POINT('Ctrl Pts',(-2.17527380048423,-1.,-3.28976645712568));
#47331=CARTESIAN_POINT('Ctrl Pts',(-2.17527380048423,1.,-3.28976645712568));
#47332=CARTESIAN_POINT('Ctrl Pts',(-2.18117455557065,-1.,-3.2945036150049));
#47333=CARTESIAN_POINT('Ctrl Pts',(-2.18117455557065,1.,-3.2945036150049));
#47334=CARTESIAN_POINT('Ctrl Pts',(-2.18710556500327,-1.,-3.29920022557639));
#47335=CARTESIAN_POINT('Ctrl Pts',(-2.18710556500327,1.,-3.29920022557639));
#47336=CARTESIAN_POINT('Ctrl Pts',(-2.19306710376111,-1.,-3.30385816281831));
#47337=CARTESIAN_POINT('Ctrl Pts',(-2.19306710376111,1.,-3.30385816281831));
#47338=CARTESIAN_POINT('Ctrl Pts',(-2.19906078949923,-1.,-3.30848134694595));
#47339=CARTESIAN_POINT('Ctrl Pts',(-2.19906078949923,1.,-3.30848134694595));
#47340=CARTESIAN_POINT('Ctrl Pts',(-2.20508863150607,-1.,-3.31307424608949));
#47341=CARTESIAN_POINT('Ctrl Pts',(-2.20508863150607,1.,-3.31307424608949));
#47342=CARTESIAN_POINT('Ctrl Pts',(-2.21115211847875,-1.,-3.31764044024235));
#47343=CARTESIAN_POINT('Ctrl Pts',(-2.21115211847875,1.,-3.31764044024235));
#47344=CARTESIAN_POINT('Ctrl Pts',(-2.21725135110898,-1.,-3.32218125618968));
#47345=CARTESIAN_POINT('Ctrl Pts',(-2.21725135110898,1.,-3.32218125618968));
#47346=CARTESIAN_POINT('Ctrl Pts',(-2.22338548312772,-1.,-3.3266964672289));
#47347=CARTESIAN_POINT('Ctrl Pts',(-2.22338548312772,1.,-3.3266964672289));
#47348=CARTESIAN_POINT('Ctrl Pts',(-2.22955308907233,-1.,-3.33118487773611));
#47349=CARTESIAN_POINT('Ctrl Pts',(-2.22955308907233,1.,-3.33118487773611));
#47350=CARTESIAN_POINT('Ctrl Pts',(-2.23575256328812,-1.,-3.33564495756482));
#47351=CARTESIAN_POINT('Ctrl Pts',(-2.23575256328812,1.,-3.33564495756482));
#47352=CARTESIAN_POINT('Ctrl Pts',(-2.24198249391422,-1.,-3.34007543738025));
#47353=CARTESIAN_POINT('Ctrl Pts',(-2.24198249391422,1.,-3.34007543738025));
#47354=CARTESIAN_POINT('Ctrl Pts',(-2.24824207678256,-1.,-3.34447596770723));
#47355=CARTESIAN_POINT('Ctrl Pts',(-2.24824207678256,1.,-3.34447596770723));
#47356=CARTESIAN_POINT('Ctrl Pts',(-2.25453097693483,-1.,-3.34884690292285));
#47357=CARTESIAN_POINT('Ctrl Pts',(-2.25453097693483,1.,-3.34884690292285));
#47358=CARTESIAN_POINT('Ctrl Pts',(-2.26084915222449,-1.,-3.35318902552626));
#47359=CARTESIAN_POINT('Ctrl Pts',(-2.26084915222449,1.,-3.35318902552626));
#47360=CARTESIAN_POINT('Ctrl Pts',(-2.2671966857991,-1.,-3.35750328523061));
#47361=CARTESIAN_POINT('Ctrl Pts',(-2.2671966857991,1.,-3.35750328523061));
#47362=CARTESIAN_POINT('Ctrl Pts',(-2.2735736262093,-1.,-3.36179055004409));
#47363=CARTESIAN_POINT('Ctrl Pts',(-2.2735736262093,1.,-3.36179055004409));
#47364=CARTESIAN_POINT('Ctrl Pts',(-2.27997979458037,-1.,-3.36605130713076));
#47365=CARTESIAN_POINT('Ctrl Pts',(-2.27997979458037,1.,-3.36605130713076));
#47366=CARTESIAN_POINT('Ctrl Pts',(-2.28641481081137,-1.,-3.37028570206488));
#47367=CARTESIAN_POINT('Ctrl Pts',(-2.28641481081137,1.,-3.37028570206488));
#47368=CARTESIAN_POINT('Ctrl Pts',(-2.29287818007393,-1.,-3.37449367172826));
#47369=CARTESIAN_POINT('Ctrl Pts',(-2.29287818007393,1.,-3.37449367172826));
#47370=CARTESIAN_POINT('Ctrl Pts',(-2.29936936127624,-1.,-3.37867504959433));
#47371=CARTESIAN_POINT('Ctrl Pts',(-2.29936936127624,1.,-3.37867504959433));
#47372=CARTESIAN_POINT('Ctrl Pts',(-2.30588783640343,-1.,-3.3828296733661));
#47373=CARTESIAN_POINT('Ctrl Pts',(-2.30588783640343,1.,-3.3828296733661));
#47374=CARTESIAN_POINT('Ctrl Pts',(-2.31243319489367,-1.,-3.38695751492462));
#47375=CARTESIAN_POINT('Ctrl Pts',(-2.31243319489367,1.,-3.38695751492462));
#47376=CARTESIAN_POINT('Ctrl Pts',(-2.31900513925424,-1.,-3.39105869474822));
#47377=CARTESIAN_POINT('Ctrl Pts',(-2.31900513925424,1.,-3.39105869474822));
#47378=CARTESIAN_POINT('Ctrl Pts',(-2.3256034390248,-1.,-3.39513342019756));
#47379=CARTESIAN_POINT('Ctrl Pts',(-2.3256034390248,1.,-3.39513342019756));
#47380=CARTESIAN_POINT('Ctrl Pts',(-2.33222789882489,-1.,-3.39918194577956));
#47381=CARTESIAN_POINT('Ctrl Pts',(-2.33222789882489,1.,-3.39918194577956));
#47382=CARTESIAN_POINT('Ctrl Pts',(-2.33887832342782,-1.,-3.40320452776743));
#47383=CARTESIAN_POINT('Ctrl Pts',(-2.33887832342782,1.,-3.40320452776743));
#47384=CARTESIAN_POINT('Ctrl Pts',(-2.34555447649188,-1.,-3.40720137404297));
#47385=CARTESIAN_POINT('Ctrl Pts',(-2.34555447649188,1.,-3.40720137404297));
#47386=CARTESIAN_POINT('Ctrl Pts',(-2.35225606824109,-1.,-3.41117262314119));
#47387=CARTESIAN_POINT('Ctrl Pts',(-2.35225606824109,1.,-3.41117262314119));
#47388=CARTESIAN_POINT('Ctrl Pts',(-2.35898278606946,-1.,-3.41511836751469));
#47389=CARTESIAN_POINT('Ctrl Pts',(-2.35898278606946,1.,-3.41511836751469));
#47390=CARTESIAN_POINT('Ctrl Pts',(-2.36573431470642,-1.,-3.41903866635852));
#47391=CARTESIAN_POINT('Ctrl Pts',(-2.36573431470642,1.,-3.41903866635852));
#47392=CARTESIAN_POINT('Ctrl Pts',(-2.37251035954292,-1.,-3.42293356216511));
#47393=CARTESIAN_POINT('Ctrl Pts',(-2.37251035954292,1.,-3.42293356216511));
#47394=CARTESIAN_POINT('Ctrl Pts',(-2.37931067028926,-1.,-3.42680309754399));
#47395=CARTESIAN_POINT('Ctrl Pts',(-2.37931067028926,1.,-3.42680309754399));
#47396=CARTESIAN_POINT('Ctrl Pts',(-2.38613505843552,-1.,-3.4306473271292));
#47397=CARTESIAN_POINT('Ctrl Pts',(-2.38613505843552,1.,-3.4306473271292));
#47398=CARTESIAN_POINT('Ctrl Pts',(-2.39298338804493,-1.,-3.4344663067854));
#47399=CARTESIAN_POINT('Ctrl Pts',(-2.39298338804493,1.,-3.4344663067854));
#47400=CARTESIAN_POINT('Ctrl Pts',(-2.39848113410292,-1.,-3.43750133064416));
#47401=CARTESIAN_POINT('Ctrl Pts',(-2.39848113410292,1.,-3.43750133064416));
#47402=CARTESIAN_POINT('Ctrl Pts',(-2.40261515589405,-1.,-3.43976627484234));
#47403=CARTESIAN_POINT('Ctrl Pts',(-2.40261515589405,1.,-3.43976627484234));
#47404=CARTESIAN_POINT('Ctrl Pts',(-2.4053759295909,-1.,-3.44127120683039));
#47405=CARTESIAN_POINT('Ctrl Pts',(-2.4053759295909,1.,-3.44127120683039));
#47406=CARTESIAN_POINT('Ctrl Pts',(-2.40675750623143,-1.,-3.44202241512147));
#47407=CARTESIAN_POINT('Ctrl Pts',(-2.40675750623143,1.,-3.44202241512147));
#47408=CARTESIAN_POINT('',(-2.03660101169714,1.,-3.14877060440328));
#47409=CARTESIAN_POINT('Ctrl Pts',(-2.03660101169715,-1.,-3.14877060440327));
#47410=CARTESIAN_POINT('Ctrl Pts',(-2.03660101169715,-0.666666666666667,
-3.14877060440327));
#47411=CARTESIAN_POINT('Ctrl Pts',(-2.03660101169715,-0.333333333333333,
-3.14877060440327));
#47412=CARTESIAN_POINT('Ctrl Pts',(-2.03660101169715,0.333333333333333,
-3.14877060440327));
#47413=CARTESIAN_POINT('Ctrl Pts',(-2.03660101169715,0.666666666666667,
-3.14877060440327));
#47414=CARTESIAN_POINT('Ctrl Pts',(-2.03660101169715,1.,-3.14877060440327));
#47415=CARTESIAN_POINT('',(-2.40675750623143,1.,-3.44202241512147));
#47416=CARTESIAN_POINT('',(-2.40675750623143,0.,-3.44202241512147));
#47417=CARTESIAN_POINT('Ctrl Pts',(-2.03660101169715,1.,-3.14877060440328));
#47418=CARTESIAN_POINT('Ctrl Pts',(-2.03659701539259,1.,-3.14881939088124));
#47419=CARTESIAN_POINT('Ctrl Pts',(-2.03663974554932,1.,-3.1490119366901));
#47420=CARTESIAN_POINT('Ctrl Pts',(-2.03693188810545,1.,-3.14959882629805));
#47421=CARTESIAN_POINT('Ctrl Pts',(-2.03783225495961,1.,-3.15102344775328));
#47422=CARTESIAN_POINT('Ctrl Pts',(-2.03984073791519,1.,-3.15389991674792));
#47423=CARTESIAN_POINT('Ctrl Pts',(-2.04297406404027,1.,-3.15817983946367));
#47424=CARTESIAN_POINT('Ctrl Pts',(-2.04693331247446,1.,-3.16343165058912));
#47425=CARTESIAN_POINT('Ctrl Pts',(-2.05151770247233,1.,-3.16936341689527));
#47426=CARTESIAN_POINT('Ctrl Pts',(-2.05650186773132,1.,-3.17564906975371));
#47427=CARTESIAN_POINT('Ctrl Pts',(-2.06166849827101,1.,-3.18197692964614));
#47428=CARTESIAN_POINT('Ctrl Pts',(-2.06684062744112,1.,-3.18809755562368));
#47429=CARTESIAN_POINT('Ctrl Pts',(-2.07192253497857,1.,-3.19388465568252));
#47430=CARTESIAN_POINT('Ctrl Pts',(-2.07690441870722,1.,-3.19934132836019));
#47431=CARTESIAN_POINT('Ctrl Pts',(-2.08182850370878,1.,-3.2045481863073));
#47432=CARTESIAN_POINT('Ctrl Pts',(-2.08676465517455,1.,-3.20962575845463));
#47433=CARTESIAN_POINT('Ctrl Pts',(-2.09178419460443,1.,-3.21469429601654));
#47434=CARTESIAN_POINT('Ctrl Pts',(-2.09692958434895,1.,-3.21982707347009));
#47435=CARTESIAN_POINT('Ctrl Pts',(-2.10220384298492,1.,-3.22503437553434));
#47436=CARTESIAN_POINT('Ctrl Pts',(-2.10758699642451,1.,-3.23028945793289));
#47437=CARTESIAN_POINT('Ctrl Pts',(-2.11304604021773,1.,-3.23554444767099));
#47438=CARTESIAN_POINT('Ctrl Pts',(-2.11854673326979,1.,-3.24074905517293));
#47439=CARTESIAN_POINT('Ctrl Pts',(-2.12406646410962,1.,-3.24587102613376));
#47440=CARTESIAN_POINT('Ctrl Pts',(-2.12960028396832,1.,-3.25090574494028));
#47441=CARTESIAN_POINT('Ctrl Pts',(-2.13515375878803,1.,-3.25586495065054));
#47442=CARTESIAN_POINT('Ctrl Pts',(-2.14073870754264,1.,-3.26077002641879));
#47443=CARTESIAN_POINT('Ctrl Pts',(-2.1463680529566,1.,-3.26564388189759));
#47444=CARTESIAN_POINT('Ctrl Pts',(-2.15205043199808,1.,-3.27050245897228));
#47445=CARTESIAN_POINT('Ctrl Pts',(-2.15778690038347,1.,-3.27534954469187));
#47446=CARTESIAN_POINT('Ctrl Pts',(-2.16357391934425,1.,-3.280181508414));
#47447=CARTESIAN_POINT('Ctrl Pts',(-2.16940517773455,1.,-3.28499019979724));
#47448=CARTESIAN_POINT('Ctrl Pts',(-2.17527380048423,1.,-3.28976645712568));
#47449=CARTESIAN_POINT('Ctrl Pts',(-2.18117455557065,1.,-3.2945036150049));
#47450=CARTESIAN_POINT('Ctrl Pts',(-2.18710556500327,1.,-3.29920022557639));
#47451=CARTESIAN_POINT('Ctrl Pts',(-2.19306710376111,1.,-3.30385816281831));
#47452=CARTESIAN_POINT('Ctrl Pts',(-2.19906078949923,1.,-3.30848134694595));
#47453=CARTESIAN_POINT('Ctrl Pts',(-2.20508863150607,1.,-3.31307424608949));
#47454=CARTESIAN_POINT('Ctrl Pts',(-2.21115211847875,1.,-3.31764044024235));
#47455=CARTESIAN_POINT('Ctrl Pts',(-2.21725135110898,1.,-3.32218125618968));
#47456=CARTESIAN_POINT('Ctrl Pts',(-2.22338548312772,1.,-3.3266964672289));
#47457=CARTESIAN_POINT('Ctrl Pts',(-2.22955308907233,1.,-3.33118487773611));
#47458=CARTESIAN_POINT('Ctrl Pts',(-2.23575256328812,1.,-3.33564495756482));
#47459=CARTESIAN_POINT('Ctrl Pts',(-2.24198249391422,1.,-3.34007543738025));
#47460=CARTESIAN_POINT('Ctrl Pts',(-2.24824207678256,1.,-3.34447596770723));
#47461=CARTESIAN_POINT('Ctrl Pts',(-2.25453097693483,1.,-3.34884690292285));
#47462=CARTESIAN_POINT('Ctrl Pts',(-2.26084915222449,1.,-3.35318902552626));
#47463=CARTESIAN_POINT('Ctrl Pts',(-2.2671966857991,1.,-3.35750328523061));
#47464=CARTESIAN_POINT('Ctrl Pts',(-2.2735736262093,1.,-3.36179055004409));
#47465=CARTESIAN_POINT('Ctrl Pts',(-2.27997979458037,1.,-3.36605130713076));
#47466=CARTESIAN_POINT('Ctrl Pts',(-2.28641481081137,1.,-3.37028570206488));
#47467=CARTESIAN_POINT('Ctrl Pts',(-2.29287818007393,1.,-3.37449367172826));
#47468=CARTESIAN_POINT('Ctrl Pts',(-2.29936936127624,1.,-3.37867504959433));
#47469=CARTESIAN_POINT('Ctrl Pts',(-2.30588783640343,1.,-3.3828296733661));
#47470=CARTESIAN_POINT('Ctrl Pts',(-2.31243319489367,1.,-3.38695751492462));
#47471=CARTESIAN_POINT('Ctrl Pts',(-2.31900513925424,1.,-3.39105869474822));
#47472=CARTESIAN_POINT('Ctrl Pts',(-2.3256034390248,1.,-3.39513342019756));
#47473=CARTESIAN_POINT('Ctrl Pts',(-2.33222789882489,1.,-3.39918194577956));
#47474=CARTESIAN_POINT('Ctrl Pts',(-2.33887832342782,1.,-3.40320452776743));
#47475=CARTESIAN_POINT('Ctrl Pts',(-2.34555447649188,1.,-3.40720137404297));
#47476=CARTESIAN_POINT('Ctrl Pts',(-2.35225606824109,1.,-3.41117262314119));
#47477=CARTESIAN_POINT('Ctrl Pts',(-2.35898278606946,1.,-3.41511836751469));
#47478=CARTESIAN_POINT('Ctrl Pts',(-2.36573431470642,1.,-3.41903866635852));
#47479=CARTESIAN_POINT('Ctrl Pts',(-2.37251035954292,1.,-3.42293356216511));
#47480=CARTESIAN_POINT('Ctrl Pts',(-2.37931067028926,1.,-3.42680309754399));
#47481=CARTESIAN_POINT('Ctrl Pts',(-2.38613505843552,1.,-3.4306473271292));
#47482=CARTESIAN_POINT('Ctrl Pts',(-2.39298338804493,1.,-3.4344663067854));
#47483=CARTESIAN_POINT('Ctrl Pts',(-2.39848113410292,1.,-3.43750133064416));
#47484=CARTESIAN_POINT('Ctrl Pts',(-2.40261515589405,1.,-3.43976627484234));
#47485=CARTESIAN_POINT('Ctrl Pts',(-2.4053759295909,1.,-3.44127120683039));
#47486=CARTESIAN_POINT('Ctrl Pts',(-2.40675750623143,1.,-3.44202241512147));
#47487=CARTESIAN_POINT('Origin',(-2.40675750623143,0.,-3.44202241512147));
#47488=CARTESIAN_POINT('',(-2.52982887637028,1.,-3.35260583073571));
#47489=CARTESIAN_POINT('Origin',(0.,0.,0.));
#47490=CARTESIAN_POINT('',(-1.88097764062697,1.,-3.24413672884812));
#47491=CARTESIAN_POINT('Origin',(0.,1.,0.));
#47492=CARTESIAN_POINT('Ctrl Pts',(-1.88097764062697,1.,-3.24413672884812));
#47493=CARTESIAN_POINT('Ctrl Pts',(-1.88097764062697,0.666666666666667,
-3.24413672884812));
#47494=CARTESIAN_POINT('Ctrl Pts',(-1.88097764062697,0.333333333333333,
-3.24413672884812));
#47495=CARTESIAN_POINT('Ctrl Pts',(-1.88097764062697,-0.333333333333333,
-3.24413672884812));
#47496=CARTESIAN_POINT('Ctrl Pts',(-1.88097764062697,-0.666666666666667,
-3.24413672884812));
#47497=CARTESIAN_POINT('Ctrl Pts',(-1.88097764062697,-1.,-3.24413672884812));
#47498=CARTESIAN_POINT('Ctrl Pts',(-1.97421938526992,-1.,-3.70708211654725));
#47499=CARTESIAN_POINT('Ctrl Pts',(-1.97421938526992,1.,-3.70708211654725));
#47500=CARTESIAN_POINT('Ctrl Pts',(-1.97417727645308,-1.,-3.70551008132332));
#47501=CARTESIAN_POINT('Ctrl Pts',(-1.97417727645308,1.,-3.70551008132332));
#47502=CARTESIAN_POINT('Ctrl Pts',(-1.97408973726715,-1.,-3.70236698912904));
#47503=CARTESIAN_POINT('Ctrl Pts',(-1.97408973726715,1.,-3.70236698912904));
#47504=CARTESIAN_POINT('Ctrl Pts',(-1.97394846383216,-1.,-3.6976552856004));
#47505=CARTESIAN_POINT('Ctrl Pts',(-1.97394846383216,1.,-3.6976552856004));
#47506=CARTESIAN_POINT('Ctrl Pts',(-1.97374016225483,-1.,-3.69137888599902));
#47507=CARTESIAN_POINT('Ctrl Pts',(-1.97374016225483,1.,-3.69137888599902));
#47508=CARTESIAN_POINT('Ctrl Pts',(-1.97344650304519,-1.,-3.68354319915092));
#47509=CARTESIAN_POINT('Ctrl Pts',(-1.97344650304519,1.,-3.68354319915092));
#47510=CARTESIAN_POINT('Ctrl Pts',(-1.97311947678517,-1.,-3.67571738107084));
#47511=CARTESIAN_POINT('Ctrl Pts',(-1.97311947678517,1.,-3.67571738107084));
#47512=CARTESIAN_POINT('Ctrl Pts',(-1.97275897198678,-1.,-3.66790152752075));
#47513=CARTESIAN_POINT('Ctrl Pts',(-1.97275897198678,1.,-3.66790152752075));
#47514=CARTESIAN_POINT('Ctrl Pts',(-1.9723648543905,-1.,-3.6600957816636));
#47515=CARTESIAN_POINT('Ctrl Pts',(-1.9723648543905,1.,-3.6600957816636));
#47516=CARTESIAN_POINT('Ctrl Pts',(-1.9719369724024,-1.,-3.652300347166));
#47517=CARTESIAN_POINT('Ctrl Pts',(-1.9719369724024,1.,-3.652300347166));
#47518=CARTESIAN_POINT('Ctrl Pts',(-1.97147515441164,-1.,-3.64451546723514));
#47519=CARTESIAN_POINT('Ctrl Pts',(-1.97147515441164,1.,-3.64451546723514));
#47520=CARTESIAN_POINT('Ctrl Pts',(-1.97097920454464,-1.,-3.63674139590412));
#47521=CARTESIAN_POINT('Ctrl Pts',(-1.97097920454464,1.,-3.63674139590412));
#47522=CARTESIAN_POINT('Ctrl Pts',(-1.97044889850463,-1.,-3.62897836973293));
#47523=CARTESIAN_POINT('Ctrl Pts',(-1.97044889850463,1.,-3.62897836973293));
#47524=CARTESIAN_POINT('Ctrl Pts',(-1.96988398129978,-1.,-3.62122658401893));
#47525=CARTESIAN_POINT('Ctrl Pts',(-1.96988398129978,1.,-3.62122658401893));
#47526=CARTESIAN_POINT('Ctrl Pts',(-1.96928416040877,-1.,-3.61348615496704));
#47527=CARTESIAN_POINT('Ctrl Pts',(-1.96928416040877,1.,-3.61348615496704));
#47528=CARTESIAN_POINT('Ctrl Pts',(-1.9686491188594,-1.,-3.60575714017989));
#47529=CARTESIAN_POINT('Ctrl Pts',(-1.9686491188594,1.,-3.60575714017989));
#47530=CARTESIAN_POINT('Ctrl Pts',(-1.96797854118369,-1.,-3.59803959819938));
#47531=CARTESIAN_POINT('Ctrl Pts',(-1.96797854118369,1.,-3.59803959819938));
#47532=CARTESIAN_POINT('Ctrl Pts',(-1.96727213799544,-1.,-3.59033364022801));
#47533=CARTESIAN_POINT('Ctrl Pts',(-1.96727213799544,1.,-3.59033364022801));
#47534=CARTESIAN_POINT('Ctrl Pts',(-1.96652966688911,-1.,-3.58263947663829));
#47535=CARTESIAN_POINT('Ctrl Pts',(-1.96652966688911,1.,-3.58263947663829));
#47536=CARTESIAN_POINT('Ctrl Pts',(-1.96575096652789,-1.,-3.57495748600959));
#47537=CARTESIAN_POINT('Ctrl Pts',(-1.96575096652789,1.,-3.57495748600959));
#47538=CARTESIAN_POINT('Ctrl Pts',(-1.96493594634567,-1.,-3.56728820357791));
#47539=CARTESIAN_POINT('Ctrl Pts',(-1.96493594634567,1.,-3.56728820357791));
#47540=CARTESIAN_POINT('Ctrl Pts',(-1.96408450906812,-1.,-3.55963218706096));
#47541=CARTESIAN_POINT('Ctrl Pts',(-1.96408450906812,1.,-3.55963218706096));
#47542=CARTESIAN_POINT('Ctrl Pts',(-1.96319648628644,-1.,-3.55198990600886));
#47543=CARTESIAN_POINT('Ctrl Pts',(-1.96319648628644,1.,-3.55198990600886));
#47544=CARTESIAN_POINT('Ctrl Pts',(-1.96227157573067,-1.,-3.54436163300443));
#47545=CARTESIAN_POINT('Ctrl Pts',(-1.96227157573067,1.,-3.54436163300443));
#47546=CARTESIAN_POINT('Ctrl Pts',(-1.96130926212689,-1.,-3.53674730625813));
#47547=CARTESIAN_POINT('Ctrl Pts',(-1.96130926212689,1.,-3.53674730625813));
#47548=CARTESIAN_POINT('Ctrl Pts',(-1.96030879411566,-1.,-3.52914648844351));
#47549=CARTESIAN_POINT('Ctrl Pts',(-1.96030879411566,1.,-3.52914648844351));
#47550=CARTESIAN_POINT('Ctrl Pts',(-1.95926936324461,-1.,-3.52155867431486));
#47551=CARTESIAN_POINT('Ctrl Pts',(-1.95926936324461,1.,-3.52155867431486));
#47552=CARTESIAN_POINT('Ctrl Pts',(-1.95819025316779,-1.,-3.51398354617794));
#47553=CARTESIAN_POINT('Ctrl Pts',(-1.95819025316779,1.,-3.51398354617794));
#47554=CARTESIAN_POINT('Ctrl Pts',(-1.95707099606511,-1.,-3.50642124159909));
#47555=CARTESIAN_POINT('Ctrl Pts',(-1.95707099606511,1.,-3.50642124159909));
#47556=CARTESIAN_POINT('Ctrl Pts',(-1.95591153823661,-1.,-3.49887263575583));
#47557=CARTESIAN_POINT('Ctrl Pts',(-1.95591153823661,1.,-3.49887263575583));
#47558=CARTESIAN_POINT('Ctrl Pts',(-1.95471236969643,-1.,-3.49133956289133));
#47559=CARTESIAN_POINT('Ctrl Pts',(-1.95471236969643,1.,-3.49133956289133));
#47560=CARTESIAN_POINT('Ctrl Pts',(-1.95347412486309,-1.,-3.48382414832634));
#47561=CARTESIAN_POINT('Ctrl Pts',(-1.95347412486309,1.,-3.48382414832634));
#47562=CARTESIAN_POINT('Ctrl Pts',(-1.95219722189876,-1.,-3.47632820495921));
#47563=CARTESIAN_POINT('Ctrl Pts',(-1.95219722189876,1.,-3.47632820495921));
#47564=CARTESIAN_POINT('Ctrl Pts',(-1.95088147859877,-1.,-3.46885258974191));
#47565=CARTESIAN_POINT('Ctrl Pts',(-1.95088147859877,1.,-3.46885258974191));
#47566=CARTESIAN_POINT('Ctrl Pts',(-1.94952575850197,-1.,-3.46139661060962));
#47567=CARTESIAN_POINT('Ctrl Pts',(-1.94952575850197,1.,-3.46139661060962));
#47568=CARTESIAN_POINT('Ctrl Pts',(-1.94812754766524,-1.,-3.45395731584051));
#47569=CARTESIAN_POINT('Ctrl Pts',(-1.94812754766524,1.,-3.45395731584051));
#47570=CARTESIAN_POINT('Ctrl Pts',(-1.94668377715329,-1.,-3.44653088665681));
#47571=CARTESIAN_POINT('Ctrl Pts',(-1.94668377715329,1.,-3.44653088665681));
#47572=CARTESIAN_POINT('Ctrl Pts',(-1.94519168842879,-1.,-3.43911410197687));
#47573=CARTESIAN_POINT('Ctrl Pts',(-1.94519168842879,1.,-3.43911410197687));
#47574=CARTESIAN_POINT('Ctrl Pts',(-1.94364973660284,-1.,-3.43170586602434));
#47575=CARTESIAN_POINT('Ctrl Pts',(-1.94364973660284,1.,-3.43170586602434));
#47576=CARTESIAN_POINT('Ctrl Pts',(-1.94205835913696,-1.,-3.42430850941503));
#47577=CARTESIAN_POINT('Ctrl Pts',(-1.94205835913696,1.,-3.42430850941503));
#47578=CARTESIAN_POINT('Ctrl Pts',(-1.94042111965246,-1.,-3.41692971994096));
#47579=CARTESIAN_POINT('Ctrl Pts',(-1.94042111965246,1.,-3.41692971994096));
#47580=CARTESIAN_POINT('Ctrl Pts',(-1.93874306008143,-1.,-3.40957978266642));
#47581=CARTESIAN_POINT('Ctrl Pts',(-1.93874306008143,1.,-3.40957978266642));
#47582=CARTESIAN_POINT('Ctrl Pts',(-1.93702857723098,-1.,-3.40226802104109));
#47583=CARTESIAN_POINT('Ctrl Pts',(-1.93702857723098,1.,-3.40226802104109));
#47584=CARTESIAN_POINT('Ctrl Pts',(-1.93527929945985,-1.,-3.39499923640795));
#47585=CARTESIAN_POINT('Ctrl Pts',(-1.93527929945985,1.,-3.39499923640795));
#47586=CARTESIAN_POINT('Ctrl Pts',(-1.93349233176788,-1.,-3.38777076883256));
#47587=CARTESIAN_POINT('Ctrl Pts',(-1.93349233176788,1.,-3.38777076883256));
#47588=CARTESIAN_POINT('Ctrl Pts',(-1.93165739093276,-1.,-3.3805676852555));
#47589=CARTESIAN_POINT('Ctrl Pts',(-1.93165739093276,1.,-3.3805676852555));
#47590=CARTESIAN_POINT('Ctrl Pts',(-1.92975993109877,-1.,-3.37336807068043));
#47591=CARTESIAN_POINT('Ctrl Pts',(-1.92975993109877,1.,-3.37336807068043));
#47592=CARTESIAN_POINT('Ctrl Pts',(-1.92778626543786,-1.,-3.36615168657567));
#47593=CARTESIAN_POINT('Ctrl Pts',(-1.92778626543786,1.,-3.36615168657567));
#47594=CARTESIAN_POINT('Ctrl Pts',(-1.92572846125756,-1.,-3.35890824422965));
#47595=CARTESIAN_POINT('Ctrl Pts',(-1.92572846125756,1.,-3.35890824422965));
#47596=CARTESIAN_POINT('Ctrl Pts',(-1.92358838440528,-1.,-3.35164424847223));
#47597=CARTESIAN_POINT('Ctrl Pts',(-1.92358838440528,1.,-3.35164424847223));
#47598=CARTESIAN_POINT('Ctrl Pts',(-1.92138450828404,-1.,-3.34439448941961));
#47599=CARTESIAN_POINT('Ctrl Pts',(-1.92138450828404,1.,-3.34439448941961));
#47600=CARTESIAN_POINT('Ctrl Pts',(-1.9191460961021,-1.,-3.33721230710012));
#47601=CARTESIAN_POINT('Ctrl Pts',(-1.9191460961021,1.,-3.33721230710012));
#47602=CARTESIAN_POINT('Ctrl Pts',(-1.91690081930331,-1.,-3.33014884257873));
#47603=CARTESIAN_POINT('Ctrl Pts',(-1.91690081930331,1.,-3.33014884257873));
#47604=CARTESIAN_POINT('Ctrl Pts',(-1.91466343916628,-1.,-3.32323403454535));
#47605=CARTESIAN_POINT('Ctrl Pts',(-1.91466343916628,1.,-3.32323403454535));
#47606=CARTESIAN_POINT('Ctrl Pts',(-1.91242616234442,-1.,-3.31646052426364));
#47607=CARTESIAN_POINT('Ctrl Pts',(-1.91242616234442,1.,-3.31646052426364));
#47608=CARTESIAN_POINT('Ctrl Pts',(-1.91014297830446,-1.,-3.30975721158596));
#47609=CARTESIAN_POINT('Ctrl Pts',(-1.91014297830446,1.,-3.30975721158596));
#47610=CARTESIAN_POINT('Ctrl Pts',(-1.90773912171341,-1.,-3.30300595568195));
#47611=CARTESIAN_POINT('Ctrl Pts',(-1.90773912171341,1.,-3.30300595568195));
#47612=CARTESIAN_POINT('Ctrl Pts',(-1.90513891864087,-1.,-3.29608978722113));
#47613=CARTESIAN_POINT('Ctrl Pts',(-1.90513891864087,1.,-3.29608978722113));
#47614=CARTESIAN_POINT('Ctrl Pts',(-1.90228971247527,-1.,-3.2889344860029));
#47615=CARTESIAN_POINT('Ctrl Pts',(-1.90228971247527,1.,-3.2889344860029));
#47616=CARTESIAN_POINT('Ctrl Pts',(-1.89918429230462,-1.,-3.28154737912352));
#47617=CARTESIAN_POINT('Ctrl Pts',(-1.89918429230462,1.,-3.28154737912352));
#47618=CARTESIAN_POINT('Ctrl Pts',(-1.89589172903793,-1.,-3.27407108933139));
#47619=CARTESIAN_POINT('Ctrl Pts',(-1.89589172903793,1.,-3.27407108933139));
#47620=CARTESIAN_POINT('Ctrl Pts',(-1.89255393500965,-1.,-3.26677653888676));
#47621=CARTESIAN_POINT('Ctrl Pts',(-1.89255393500965,1.,-3.26677653888676));
#47622=CARTESIAN_POINT('Ctrl Pts',(-1.88934996203698,-1.,-3.25999885193947));
#47623=CARTESIAN_POINT('Ctrl Pts',(-1.88934996203698,1.,-3.25999885193947));
#47624=CARTESIAN_POINT('Ctrl Pts',(-1.88646802523466,-1.,-3.25408686339463));
#47625=CARTESIAN_POINT('Ctrl Pts',(-1.88646802523466,1.,-3.25408686339463));
#47626=CARTESIAN_POINT('Ctrl Pts',(-1.88407708646357,-1.,-3.24935200511918));
#47627=CARTESIAN_POINT('Ctrl Pts',(-1.88407708646357,1.,-3.24935200511918));
#47628=CARTESIAN_POINT('Ctrl Pts',(-1.88229202582941,-1.,-3.24600543790443));
#47629=CARTESIAN_POINT('Ctrl Pts',(-1.88229202582941,1.,-3.24600543790443));
#47630=CARTESIAN_POINT('Ctrl Pts',(-1.88139187908074,-1.,-3.24451807186481));
#47631=CARTESIAN_POINT('Ctrl Pts',(-1.88139187908074,1.,-3.24451807186481));
#47632=CARTESIAN_POINT('Ctrl Pts',(-1.88102201872555,-1.,-3.24408699284121));
#47633=CARTESIAN_POINT('Ctrl Pts',(-1.88102201872555,1.,-3.24408699284121));
#47634=CARTESIAN_POINT('Ctrl Pts',(-1.88091100680349,-1.,-3.24410359189609));
#47635=CARTESIAN_POINT('Ctrl Pts',(-1.88091100680349,1.,-3.24410359189609));
#47636=CARTESIAN_POINT('Ctrl Pts',(-1.8808893942881,-1.,-3.24418789321065));
#47637=CARTESIAN_POINT('Ctrl Pts',(-1.8808893942881,1.,-3.24418789321065));
#47638=CARTESIAN_POINT('',(-1.97421938526992,1.,-3.70708211654725));
#47639=CARTESIAN_POINT('Ctrl Pts',(-1.97421938526992,1.,-3.70708211654725));
#47640=CARTESIAN_POINT('Ctrl Pts',(-1.97417727645308,1.,-3.70551008132332));
#47641=CARTESIAN_POINT('Ctrl Pts',(-1.97408973726715,1.,-3.70236698912904));
#47642=CARTESIAN_POINT('Ctrl Pts',(-1.97394846383216,1.,-3.6976552856004));
#47643=CARTESIAN_POINT('Ctrl Pts',(-1.97374016225483,1.,-3.69137888599902));
#47644=CARTESIAN_POINT('Ctrl Pts',(-1.97344650304519,1.,-3.68354319915092));
#47645=CARTESIAN_POINT('Ctrl Pts',(-1.97311947678517,1.,-3.67571738107084));
#47646=CARTESIAN_POINT('Ctrl Pts',(-1.97275897198678,1.,-3.66790152752075));
#47647=CARTESIAN_POINT('Ctrl Pts',(-1.9723648543905,1.,-3.6600957816636));
#47648=CARTESIAN_POINT('Ctrl Pts',(-1.9719369724024,1.,-3.652300347166));
#47649=CARTESIAN_POINT('Ctrl Pts',(-1.97147515441164,1.,-3.64451546723514));
#47650=CARTESIAN_POINT('Ctrl Pts',(-1.97097920454464,1.,-3.63674139590412));
#47651=CARTESIAN_POINT('Ctrl Pts',(-1.97044889850463,1.,-3.62897836973293));
#47652=CARTESIAN_POINT('Ctrl Pts',(-1.96988398129978,1.,-3.62122658401893));
#47653=CARTESIAN_POINT('Ctrl Pts',(-1.96928416040877,1.,-3.61348615496704));
#47654=CARTESIAN_POINT('Ctrl Pts',(-1.9686491188594,1.,-3.60575714017989));
#47655=CARTESIAN_POINT('Ctrl Pts',(-1.96797854118369,1.,-3.59803959819938));
#47656=CARTESIAN_POINT('Ctrl Pts',(-1.96727213799544,1.,-3.59033364022801));
#47657=CARTESIAN_POINT('Ctrl Pts',(-1.96652966688911,1.,-3.58263947663829));
#47658=CARTESIAN_POINT('Ctrl Pts',(-1.96575096652789,1.,-3.57495748600959));
#47659=CARTESIAN_POINT('Ctrl Pts',(-1.96493594634567,1.,-3.56728820357791));
#47660=CARTESIAN_POINT('Ctrl Pts',(-1.96408450906812,1.,-3.55963218706096));
#47661=CARTESIAN_POINT('Ctrl Pts',(-1.96319648628644,1.,-3.55198990600886));
#47662=CARTESIAN_POINT('Ctrl Pts',(-1.96227157573067,1.,-3.54436163300443));
#47663=CARTESIAN_POINT('Ctrl Pts',(-1.96130926212689,1.,-3.53674730625813));
#47664=CARTESIAN_POINT('Ctrl Pts',(-1.96030879411566,1.,-3.52914648844351));
#47665=CARTESIAN_POINT('Ctrl Pts',(-1.95926936324461,1.,-3.52155867431486));
#47666=CARTESIAN_POINT('Ctrl Pts',(-1.95819025316779,1.,-3.51398354617794));
#47667=CARTESIAN_POINT('Ctrl Pts',(-1.95707099606511,1.,-3.50642124159909));
#47668=CARTESIAN_POINT('Ctrl Pts',(-1.95591153823661,1.,-3.49887263575583));
#47669=CARTESIAN_POINT('Ctrl Pts',(-1.95471236969643,1.,-3.49133956289133));
#47670=CARTESIAN_POINT('Ctrl Pts',(-1.95347412486309,1.,-3.48382414832634));
#47671=CARTESIAN_POINT('Ctrl Pts',(-1.95219722189876,1.,-3.47632820495921));
#47672=CARTESIAN_POINT('Ctrl Pts',(-1.95088147859877,1.,-3.46885258974191));
#47673=CARTESIAN_POINT('Ctrl Pts',(-1.94952575850197,1.,-3.46139661060962));
#47674=CARTESIAN_POINT('Ctrl Pts',(-1.94812754766524,1.,-3.45395731584051));
#47675=CARTESIAN_POINT('Ctrl Pts',(-1.94668377715329,1.,-3.44653088665681));
#47676=CARTESIAN_POINT('Ctrl Pts',(-1.94519168842879,1.,-3.43911410197687));
#47677=CARTESIAN_POINT('Ctrl Pts',(-1.94364973660284,1.,-3.43170586602434));
#47678=CARTESIAN_POINT('Ctrl Pts',(-1.94205835913696,1.,-3.42430850941503));
#47679=CARTESIAN_POINT('Ctrl Pts',(-1.94042111965246,1.,-3.41692971994096));
#47680=CARTESIAN_POINT('Ctrl Pts',(-1.93874306008143,1.,-3.40957978266642));
#47681=CARTESIAN_POINT('Ctrl Pts',(-1.93702857723098,1.,-3.40226802104109));
#47682=CARTESIAN_POINT('Ctrl Pts',(-1.93527929945985,1.,-3.39499923640795));
#47683=CARTESIAN_POINT('Ctrl Pts',(-1.93349233176788,1.,-3.38777076883256));
#47684=CARTESIAN_POINT('Ctrl Pts',(-1.93165739093276,1.,-3.3805676852555));
#47685=CARTESIAN_POINT('Ctrl Pts',(-1.92975993109877,1.,-3.37336807068043));
#47686=CARTESIAN_POINT('Ctrl Pts',(-1.92778626543786,1.,-3.36615168657567));
#47687=CARTESIAN_POINT('Ctrl Pts',(-1.92572846125756,1.,-3.35890824422965));
#47688=CARTESIAN_POINT('Ctrl Pts',(-1.92358838440528,1.,-3.35164424847223));
#47689=CARTESIAN_POINT('Ctrl Pts',(-1.92138450828404,1.,-3.34439448941961));
#47690=CARTESIAN_POINT('Ctrl Pts',(-1.9191460961021,1.,-3.33721230710012));
#47691=CARTESIAN_POINT('Ctrl Pts',(-1.91690081930331,1.,-3.33014884257873));
#47692=CARTESIAN_POINT('Ctrl Pts',(-1.91466343916628,1.,-3.32323403454535));
#47693=CARTESIAN_POINT('Ctrl Pts',(-1.91242616234442,1.,-3.31646052426364));
#47694=CARTESIAN_POINT('Ctrl Pts',(-1.91014297830446,1.,-3.30975721158596));
#47695=CARTESIAN_POINT('Ctrl Pts',(-1.90773912171341,1.,-3.30300595568195));
#47696=CARTESIAN_POINT('Ctrl Pts',(-1.90513891864087,1.,-3.29608978722113));
#47697=CARTESIAN_POINT('Ctrl Pts',(-1.90228971247527,1.,-3.2889344860029));
#47698=CARTESIAN_POINT('Ctrl Pts',(-1.89918429230462,1.,-3.28154737912352));
#47699=CARTESIAN_POINT('Ctrl Pts',(-1.89589172903793,1.,-3.27407108933139));
#47700=CARTESIAN_POINT('Ctrl Pts',(-1.89255393500965,1.,-3.26677653888676));
#47701=CARTESIAN_POINT('Ctrl Pts',(-1.88934996203698,1.,-3.25999885193947));
#47702=CARTESIAN_POINT('Ctrl Pts',(-1.88646802523466,1.,-3.25408686339463));
#47703=CARTESIAN_POINT('Ctrl Pts',(-1.88407708646357,1.,-3.24935200511918));
#47704=CARTESIAN_POINT('Ctrl Pts',(-1.88242596600454,1.,-3.2462565441079));
#47705=CARTESIAN_POINT('Ctrl Pts',(-1.88156537699203,1.,-3.24480754676064));
#47706=CARTESIAN_POINT('Ctrl Pts',(-1.88117508446775,1.,-3.24428080353022));
#47707=CARTESIAN_POINT('Ctrl Pts',(-1.8810229239812,1.,-3.24415531671284));
#47708=CARTESIAN_POINT('Ctrl Pts',(-1.88097764062697,1.,-3.24413672884812));
#47709=CARTESIAN_POINT('',(-1.97421938526992,0.,-3.70708211654725));
#47710=CARTESIAN_POINT('Ctrl Pts',(-1.519044091397,-1.,-3.42855728381368));
#47711=CARTESIAN_POINT('Ctrl Pts',(-1.519044091397,1.,-3.42855728381368));
#47712=CARTESIAN_POINT('Ctrl Pts',(-1.51896318668366,-1.,-3.42852521763778));
#47713=CARTESIAN_POINT('Ctrl Pts',(-1.51896318668366,1.,-3.42852521763778));
#47714=CARTESIAN_POINT('Ctrl Pts',(-1.51888450659652,-1.,-3.42860527149177));
#47715=CARTESIAN_POINT('Ctrl Pts',(-1.51888450659652,1.,-3.42860527149177));
#47716=CARTESIAN_POINT('Ctrl Pts',(-1.51901585839109,-1.,-3.42915787669893));
#47717=CARTESIAN_POINT('Ctrl Pts',(-1.51901585839109,1.,-3.42915787669893));
#47718=CARTESIAN_POINT('Ctrl Pts',(-1.51969006980999,-1.,-3.43076036253837));
#47719=CARTESIAN_POINT('Ctrl Pts',(-1.51969006980999,1.,-3.43076036253837));
#47720=CARTESIAN_POINT('Ctrl Pts',(-1.52134826724293,-1.,-3.43417156977893));
#47721=CARTESIAN_POINT('Ctrl Pts',(-1.52134826724293,1.,-3.43417156977893));
#47722=CARTESIAN_POINT('Ctrl Pts',(-1.5237734895035,-1.,-3.4388889597401));
#47723=CARTESIAN_POINT('Ctrl Pts',(-1.5237734895035,1.,-3.4388889597401));
#47724=CARTESIAN_POINT('Ctrl Pts',(-1.52686242875556,-1.,-3.44469547526647));
#47725=CARTESIAN_POINT('Ctrl Pts',(-1.52686242875556,1.,-3.44469547526647));
#47726=CARTESIAN_POINT('Ctrl Pts',(-1.53046244461635,-1.,-3.45127136828305));
#47727=CARTESIAN_POINT('Ctrl Pts',(-1.53046244461635,1.,-3.45127136828305));
#47728=CARTESIAN_POINT('Ctrl Pts',(-1.53440195378792,-1.,-3.45825932955032));
#47729=CARTESIAN_POINT('Ctrl Pts',(-1.53440195378792,1.,-3.45825932955032));
#47730=CARTESIAN_POINT('Ctrl Pts',(-1.53851507915502,-1.,-3.46531752207153));
#47731=CARTESIAN_POINT('Ctrl Pts',(-1.53851507915502,1.,-3.46531752207153));
#47732=CARTESIAN_POINT('Ctrl Pts',(-1.54266605398187,-1.,-3.47217189224653));
#47733=CARTESIAN_POINT('Ctrl Pts',(-1.54266605398187,1.,-3.47217189224653));
#47734=CARTESIAN_POINT('Ctrl Pts',(-1.54678009290276,-1.,-3.47868272898751));
#47735=CARTESIAN_POINT('Ctrl Pts',(-1.54678009290276,1.,-3.47868272898751));
#47736=CARTESIAN_POINT('Ctrl Pts',(-1.55084702970452,-1.,-3.48485155928567));
#47737=CARTESIAN_POINT('Ctrl Pts',(-1.55084702970452,1.,-3.48485155928567));
#47738=CARTESIAN_POINT('Ctrl Pts',(-1.55489595901116,-1.,-3.4907646087742));
#47739=CARTESIAN_POINT('Ctrl Pts',(-1.55489595901116,1.,-3.4907646087742));
#47740=CARTESIAN_POINT('Ctrl Pts',(-1.55897703097874,-1.,-3.49655185179655));
#47741=CARTESIAN_POINT('Ctrl Pts',(-1.55897703097874,1.,-3.49655185179655));
#47742=CARTESIAN_POINT('Ctrl Pts',(-1.56314187758675,-1.,-3.50234321621578));
#47743=CARTESIAN_POINT('Ctrl Pts',(-1.56314187758675,1.,-3.50234321621578));
#47744=CARTESIAN_POINT('Ctrl Pts',(-1.56742097575012,-1.,-3.50821771695363));
#47745=CARTESIAN_POINT('Ctrl Pts',(-1.56742097575012,1.,-3.50821771695363));
#47746=CARTESIAN_POINT('Ctrl Pts',(-1.57181569799743,-1.,-3.51418598431665));
#47747=CARTESIAN_POINT('Ctrl Pts',(-1.57181569799743,1.,-3.51418598431665));
#47748=CARTESIAN_POINT('Ctrl Pts',(-1.57631049988158,-1.,-3.52021847865912));
#47749=CARTESIAN_POINT('Ctrl Pts',(-1.57631049988158,1.,-3.52021847865912));
#47750=CARTESIAN_POINT('Ctrl Pts',(-1.58088027227848,-1.,-3.52626275334881));
#47751=CARTESIAN_POINT('Ctrl Pts',(-1.58088027227848,1.,-3.52626275334881));
#47752=CARTESIAN_POINT('Ctrl Pts',(-1.58549906268088,-1.,-3.5322637814708));
#47753=CARTESIAN_POINT('Ctrl Pts',(-1.58549906268088,1.,-3.5322637814708));
#47754=CARTESIAN_POINT('Ctrl Pts',(-1.59014958368739,-1.,-3.53818616861077));
#47755=CARTESIAN_POINT('Ctrl Pts',(-1.59014958368739,1.,-3.53818616861077));
#47756=CARTESIAN_POINT('Ctrl Pts',(-1.59482766949766,-1.,-3.54402458182337));
#47757=CARTESIAN_POINT('Ctrl Pts',(-1.59482766949766,1.,-3.54402458182337));
#47758=CARTESIAN_POINT('Ctrl Pts',(-1.59953698113457,-1.,-3.54979148634454));
#47759=CARTESIAN_POINT('Ctrl Pts',(-1.59953698113457,1.,-3.54979148634454));
#47760=CARTESIAN_POINT('Ctrl Pts',(-1.60428584699853,-1.,-3.55550985096129));
#47761=CARTESIAN_POINT('Ctrl Pts',(-1.60428584699853,1.,-3.55550985096129));
#47762=CARTESIAN_POINT('Ctrl Pts',(-1.60908344685457,-1.,-3.5612043248298));
#47763=CARTESIAN_POINT('Ctrl Pts',(-1.60908344685457,1.,-3.5612043248298));
#47764=CARTESIAN_POINT('Ctrl Pts',(-1.61393581747514,-1.,-3.56689200468387));
#47765=CARTESIAN_POINT('Ctrl Pts',(-1.61393581747514,1.,-3.56689200468387));
#47766=CARTESIAN_POINT('Ctrl Pts',(-1.61884340915404,-1.,-3.57257679609806));
#47767=CARTESIAN_POINT('Ctrl Pts',(-1.61884340915404,1.,-3.57257679609806));
#47768=CARTESIAN_POINT('Ctrl Pts',(-1.62380329464844,-1.,-3.5782545595439));
#47769=CARTESIAN_POINT('Ctrl Pts',(-1.62380329464844,1.,-3.5782545595439));
#47770=CARTESIAN_POINT('Ctrl Pts',(-1.62881051550745,-1.,-3.58391625774343));
#47771=CARTESIAN_POINT('Ctrl Pts',(-1.62881051550745,1.,-3.58391625774343));
#47772=CARTESIAN_POINT('Ctrl Pts',(-1.6338597145126,-1.,-3.58955176627879));
#47773=CARTESIAN_POINT('Ctrl Pts',(-1.6338597145126,1.,-3.58955176627879));
#47774=CARTESIAN_POINT('Ctrl Pts',(-1.63894676675352,-1.,-3.59515368334893));
#47775=CARTESIAN_POINT('Ctrl Pts',(-1.63894676675352,1.,-3.59515368334893));
#47776=CARTESIAN_POINT('Ctrl Pts',(-1.64407004385582,-1.,-3.60072028513845));
#47777=CARTESIAN_POINT('Ctrl Pts',(-1.64407004385582,1.,-3.60072028513845));
#47778=CARTESIAN_POINT('Ctrl Pts',(-1.64922952425832,-1.,-3.60625346556992));
#47779=CARTESIAN_POINT('Ctrl Pts',(-1.64922952425832,1.,-3.60625346556992));
#47780=CARTESIAN_POINT('Ctrl Pts',(-1.65442619244325,-1.,-3.61175734965127));
#47781=CARTESIAN_POINT('Ctrl Pts',(-1.65442619244325,1.,-3.61175734965127));
#47782=CARTESIAN_POINT('Ctrl Pts',(-1.65966133399186,-1.,-3.61723666482456));
#47783=CARTESIAN_POINT('Ctrl Pts',(-1.65966133399186,1.,-3.61723666482456));
#47784=CARTESIAN_POINT('Ctrl Pts',(-1.66493585923855,-1.,-3.62269517989109));
#47785=CARTESIAN_POINT('Ctrl Pts',(-1.66493585923855,1.,-3.62269517989109));
#47786=CARTESIAN_POINT('Ctrl Pts',(-1.67024966008045,-1.,-3.62813422105271));
#47787=CARTESIAN_POINT('Ctrl Pts',(-1.67024966008045,1.,-3.62813422105271));
#47788=CARTESIAN_POINT('Ctrl Pts',(-1.67560193613156,-1.,-3.63355343201232));
#47789=CARTESIAN_POINT('Ctrl Pts',(-1.67560193613156,1.,-3.63355343201232));
#47790=CARTESIAN_POINT('Ctrl Pts',(-1.68099146651586,-1.,-3.63895140887462));
#47791=CARTESIAN_POINT('Ctrl Pts',(-1.68099146651586,1.,-3.63895140887462));
#47792=CARTESIAN_POINT('Ctrl Pts',(-1.68641690471457,-1.,-3.64432638915203));
#47793=CARTESIAN_POINT('Ctrl Pts',(-1.68641690471457,1.,-3.64432638915203));
#47794=CARTESIAN_POINT('Ctrl Pts',(-1.69187705481689,-1.,-3.64967689827371));
#47795=CARTESIAN_POINT('Ctrl Pts',(-1.69187705481689,1.,-3.64967689827371));
#47796=CARTESIAN_POINT('Ctrl Pts',(-1.69737117722534,-1.,-3.65500246526749));
#47797=CARTESIAN_POINT('Ctrl Pts',(-1.69737117722534,1.,-3.65500246526749));
#47798=CARTESIAN_POINT('Ctrl Pts',(-1.70289888566873,-1.,-3.66030338774847));
#47799=CARTESIAN_POINT('Ctrl Pts',(-1.70289888566873,1.,-3.66030338774847));
#47800=CARTESIAN_POINT('Ctrl Pts',(-1.70846001610956,-1.,-3.66558043198876));
#47801=CARTESIAN_POINT('Ctrl Pts',(-1.70846001610956,1.,-3.66558043198876));
#47802=CARTESIAN_POINT('Ctrl Pts',(-1.71405450210384,-1.,-3.67083454901611));
#47803=CARTESIAN_POINT('Ctrl Pts',(-1.71405450210384,1.,-3.67083454901611));
#47804=CARTESIAN_POINT('Ctrl Pts',(-1.71968225581808,-1.,-3.67606660374709));
#47805=CARTESIAN_POINT('Ctrl Pts',(-1.71968225581808,1.,-3.67606660374709));
#47806=CARTESIAN_POINT('Ctrl Pts',(-1.72534302437056,-1.,-3.68127704936579));
#47807=CARTESIAN_POINT('Ctrl Pts',(-1.72534302437056,1.,-3.68127704936579));
#47808=CARTESIAN_POINT('Ctrl Pts',(-1.73103640956717,-1.,-3.68646597019332));
#47809=CARTESIAN_POINT('Ctrl Pts',(-1.73103640956717,1.,-3.68646597019332));
#47810=CARTESIAN_POINT('Ctrl Pts',(-1.73676193254557,-1.,-3.69163322648036));
#47811=CARTESIAN_POINT('Ctrl Pts',(-1.73676193254557,1.,-3.69163322648036));
#47812=CARTESIAN_POINT('Ctrl Pts',(-1.74251908492617,-1.,-3.69677856910517));
#47813=CARTESIAN_POINT('Ctrl Pts',(-1.74251908492617,1.,-3.69677856910517));
#47814=CARTESIAN_POINT('Ctrl Pts',(-1.74830738046057,-1.,-3.7019017567335));
#47815=CARTESIAN_POINT('Ctrl Pts',(-1.74830738046057,1.,-3.7019017567335));
#47816=CARTESIAN_POINT('Ctrl Pts',(-1.75412641804042,-1.,-3.70700269736659));
#47817=CARTESIAN_POINT('Ctrl Pts',(-1.75412641804042,1.,-3.70700269736659));
#47818=CARTESIAN_POINT('Ctrl Pts',(-1.75997588498865,-1.,-3.71208146346136));
#47819=CARTESIAN_POINT('Ctrl Pts',(-1.75997588498865,1.,-3.71208146346136));
#47820=CARTESIAN_POINT('Ctrl Pts',(-1.76585552124394,-1.,-3.71713822377359));
#47821=CARTESIAN_POINT('Ctrl Pts',(-1.76585552124394,1.,-3.71713822377359));
#47822=CARTESIAN_POINT('Ctrl Pts',(-1.77176509401761,-1.,-3.72217319911254));
#47823=CARTESIAN_POINT('Ctrl Pts',(-1.77176509401761,1.,-3.72217319911254));
#47824=CARTESIAN_POINT('Ctrl Pts',(-1.77770437039658,-1.,-3.72718661205609));
#47825=CARTESIAN_POINT('Ctrl Pts',(-1.77770437039658,1.,-3.72718661205609));
#47826=CARTESIAN_POINT('Ctrl Pts',(-1.78367308442901,-1.,-3.7321786309547));
#47827=CARTESIAN_POINT('Ctrl Pts',(-1.78367308442901,1.,-3.7321786309547));
#47828=CARTESIAN_POINT('Ctrl Pts',(-1.78967092823491,-1.,-3.73714934730681));
#47829=CARTESIAN_POINT('Ctrl Pts',(-1.78967092823491,1.,-3.73714934730681));
#47830=CARTESIAN_POINT('Ctrl Pts',(-1.79569757859422,-1.,-3.74209880352445));
#47831=CARTESIAN_POINT('Ctrl Pts',(-1.79569757859422,1.,-3.74209880352445));
#47832=CARTESIAN_POINT('Ctrl Pts',(-1.8017527148577,-1.,-3.74702700875467));
#47833=CARTESIAN_POINT('Ctrl Pts',(-1.8017527148577,1.,-3.74702700875467));
#47834=CARTESIAN_POINT('Ctrl Pts',(-1.80783603939617,-1.,-3.75193395887977));
#47835=CARTESIAN_POINT('Ctrl Pts',(-1.80783603939617,1.,-3.75193395887977));
#47836=CARTESIAN_POINT('Ctrl Pts',(-1.8139472983358,-1.,-3.75681965683071));
#47837=CARTESIAN_POINT('Ctrl Pts',(-1.8139472983358,1.,-3.75681965683071));
#47838=CARTESIAN_POINT('Ctrl Pts',(-1.82008629694091,-1.,-3.76168412707948));
#47839=CARTESIAN_POINT('Ctrl Pts',(-1.82008629694091,1.,-3.76168412707948));
#47840=CARTESIAN_POINT('Ctrl Pts',(-1.82625289220915,-1.,-3.76652740353775));
#47841=CARTESIAN_POINT('Ctrl Pts',(-1.82625289220915,1.,-3.76652740353775));
#47842=CARTESIAN_POINT('Ctrl Pts',(-1.83120816955645,-1.,-3.77038509817999));
#47843=CARTESIAN_POINT('Ctrl Pts',(-1.83120816955645,1.,-3.77038509817999));
#47844=CARTESIAN_POINT('Ctrl Pts',(-1.83493697934534,-1.,-3.77326886064398));
#47845=CARTESIAN_POINT('Ctrl Pts',(-1.83493697934534,1.,-3.77326886064398));
#47846=CARTESIAN_POINT('Ctrl Pts',(-1.83742834010626,-1.,-3.77518714457833));
#47847=CARTESIAN_POINT('Ctrl Pts',(-1.83742834010626,1.,-3.77518714457833));
#47848=CARTESIAN_POINT('Ctrl Pts',(-1.83867539237861,-1.,-3.77614523045147));
#47849=CARTESIAN_POINT('Ctrl Pts',(-1.83867539237861,1.,-3.77614523045147));
#47850=CARTESIAN_POINT('',(-1.5189508286633,1.,-3.42859860294306));
#47851=CARTESIAN_POINT('Ctrl Pts',(-1.5189508286633,-1.,-3.42859860294306));
#47852=CARTESIAN_POINT('Ctrl Pts',(-1.5189508286633,-0.666666666666667,
-3.42859860294306));
#47853=CARTESIAN_POINT('Ctrl Pts',(-1.5189508286633,-0.333333333333333,
-3.42859860294306));
#47854=CARTESIAN_POINT('Ctrl Pts',(-1.5189508286633,0.333333333333333,-3.42859860294306));
#47855=CARTESIAN_POINT('Ctrl Pts',(-1.5189508286633,0.666666666666667,-3.42859860294305));
#47856=CARTESIAN_POINT('Ctrl Pts',(-1.5189508286633,1.,-3.42859860294305));
#47857=CARTESIAN_POINT('',(-1.83867539237861,1.,-3.77614523045147));
#47858=CARTESIAN_POINT('',(-1.83867539237861,0.,-3.77614523045147));
#47859=CARTESIAN_POINT('Ctrl Pts',(-1.5189508286633,1.,-3.42859860294306));
#47860=CARTESIAN_POINT('Ctrl Pts',(-1.51893924967331,1.,-3.42864616361875));
#47861=CARTESIAN_POINT('Ctrl Pts',(-1.5189513329503,1.,-3.42884302333841));
#47862=CARTESIAN_POINT('Ctrl Pts',(-1.51914806898491,1.,-3.42946838852588));
#47863=CARTESIAN_POINT('Ctrl Pts',(-1.5198144909338,1.,-3.43101631893414));
#47864=CARTESIAN_POINT('Ctrl Pts',(-1.52134826724293,1.,-3.43417156977893));
#47865=CARTESIAN_POINT('Ctrl Pts',(-1.5237734895035,1.,-3.4388889597401));
#47866=CARTESIAN_POINT('Ctrl Pts',(-1.52686242875556,1.,-3.44469547526647));
#47867=CARTESIAN_POINT('Ctrl Pts',(-1.53046244461635,1.,-3.45127136828305));
#47868=CARTESIAN_POINT('Ctrl Pts',(-1.53440195378792,1.,-3.45825932955032));
#47869=CARTESIAN_POINT('Ctrl Pts',(-1.53851507915502,1.,-3.46531752207153));
#47870=CARTESIAN_POINT('Ctrl Pts',(-1.54266605398187,1.,-3.47217189224653));
#47871=CARTESIAN_POINT('Ctrl Pts',(-1.54678009290276,1.,-3.47868272898751));
#47872=CARTESIAN_POINT('Ctrl Pts',(-1.55084702970452,1.,-3.48485155928567));
#47873=CARTESIAN_POINT('Ctrl Pts',(-1.55489595901116,1.,-3.4907646087742));
#47874=CARTESIAN_POINT('Ctrl Pts',(-1.55897703097874,1.,-3.49655185179655));
#47875=CARTESIAN_POINT('Ctrl Pts',(-1.56314187758675,1.,-3.50234321621578));
#47876=CARTESIAN_POINT('Ctrl Pts',(-1.56742097575012,1.,-3.50821771695363));
#47877=CARTESIAN_POINT('Ctrl Pts',(-1.57181569799743,1.,-3.51418598431665));
#47878=CARTESIAN_POINT('Ctrl Pts',(-1.57631049988158,1.,-3.52021847865912));
#47879=CARTESIAN_POINT('Ctrl Pts',(-1.58088027227848,1.,-3.52626275334881));
#47880=CARTESIAN_POINT('Ctrl Pts',(-1.58549906268088,1.,-3.5322637814708));
#47881=CARTESIAN_POINT('Ctrl Pts',(-1.59014958368739,1.,-3.53818616861077));
#47882=CARTESIAN_POINT('Ctrl Pts',(-1.59482766949766,1.,-3.54402458182337));
#47883=CARTESIAN_POINT('Ctrl Pts',(-1.59953698113457,1.,-3.54979148634454));
#47884=CARTESIAN_POINT('Ctrl Pts',(-1.60428584699853,1.,-3.55550985096129));
#47885=CARTESIAN_POINT('Ctrl Pts',(-1.60908344685457,1.,-3.5612043248298));
#47886=CARTESIAN_POINT('Ctrl Pts',(-1.61393581747514,1.,-3.56689200468387));
#47887=CARTESIAN_POINT('Ctrl Pts',(-1.61884340915404,1.,-3.57257679609806));
#47888=CARTESIAN_POINT('Ctrl Pts',(-1.62380329464844,1.,-3.5782545595439));
#47889=CARTESIAN_POINT('Ctrl Pts',(-1.62881051550745,1.,-3.58391625774343));
#47890=CARTESIAN_POINT('Ctrl Pts',(-1.6338597145126,1.,-3.58955176627879));
#47891=CARTESIAN_POINT('Ctrl Pts',(-1.63894676675352,1.,-3.59515368334893));
#47892=CARTESIAN_POINT('Ctrl Pts',(-1.64407004385582,1.,-3.60072028513845));
#47893=CARTESIAN_POINT('Ctrl Pts',(-1.64922952425832,1.,-3.60625346556992));
#47894=CARTESIAN_POINT('Ctrl Pts',(-1.65442619244325,1.,-3.61175734965127));
#47895=CARTESIAN_POINT('Ctrl Pts',(-1.65966133399186,1.,-3.61723666482456));
#47896=CARTESIAN_POINT('Ctrl Pts',(-1.66493585923855,1.,-3.62269517989109));
#47897=CARTESIAN_POINT('Ctrl Pts',(-1.67024966008045,1.,-3.62813422105271));
#47898=CARTESIAN_POINT('Ctrl Pts',(-1.67560193613156,1.,-3.63355343201232));
#47899=CARTESIAN_POINT('Ctrl Pts',(-1.68099146651586,1.,-3.63895140887462));
#47900=CARTESIAN_POINT('Ctrl Pts',(-1.68641690471457,1.,-3.64432638915203));
#47901=CARTESIAN_POINT('Ctrl Pts',(-1.69187705481689,1.,-3.64967689827371));
#47902=CARTESIAN_POINT('Ctrl Pts',(-1.69737117722534,1.,-3.65500246526749));
#47903=CARTESIAN_POINT('Ctrl Pts',(-1.70289888566873,1.,-3.66030338774847));
#47904=CARTESIAN_POINT('Ctrl Pts',(-1.70846001610956,1.,-3.66558043198876));
#47905=CARTESIAN_POINT('Ctrl Pts',(-1.71405450210384,1.,-3.67083454901611));
#47906=CARTESIAN_POINT('Ctrl Pts',(-1.71968225581808,1.,-3.67606660374709));
#47907=CARTESIAN_POINT('Ctrl Pts',(-1.72534302437056,1.,-3.68127704936579));
#47908=CARTESIAN_POINT('Ctrl Pts',(-1.73103640956717,1.,-3.68646597019332));
#47909=CARTESIAN_POINT('Ctrl Pts',(-1.73676193254557,1.,-3.69163322648036));
#47910=CARTESIAN_POINT('Ctrl Pts',(-1.74251908492617,1.,-3.69677856910517));
#47911=CARTESIAN_POINT('Ctrl Pts',(-1.74830738046057,1.,-3.7019017567335));
#47912=CARTESIAN_POINT('Ctrl Pts',(-1.75412641804042,1.,-3.70700269736659));
#47913=CARTESIAN_POINT('Ctrl Pts',(-1.75997588498865,1.,-3.71208146346136));
#47914=CARTESIAN_POINT('Ctrl Pts',(-1.76585552124394,1.,-3.71713822377359));
#47915=CARTESIAN_POINT('Ctrl Pts',(-1.77176509401761,1.,-3.72217319911254));
#47916=CARTESIAN_POINT('Ctrl Pts',(-1.77770437039658,1.,-3.72718661205609));
#47917=CARTESIAN_POINT('Ctrl Pts',(-1.78367308442901,1.,-3.7321786309547));
#47918=CARTESIAN_POINT('Ctrl Pts',(-1.78967092823491,1.,-3.73714934730681));
#47919=CARTESIAN_POINT('Ctrl Pts',(-1.79569757859422,1.,-3.74209880352445));
#47920=CARTESIAN_POINT('Ctrl Pts',(-1.8017527148577,1.,-3.74702700875467));
#47921=CARTESIAN_POINT('Ctrl Pts',(-1.80783603939617,1.,-3.75193395887977));
#47922=CARTESIAN_POINT('Ctrl Pts',(-1.8139472983358,1.,-3.75681965683071));
#47923=CARTESIAN_POINT('Ctrl Pts',(-1.82008629694091,1.,-3.76168412707948));
#47924=CARTESIAN_POINT('Ctrl Pts',(-1.82625289220915,1.,-3.76652740353775));
#47925=CARTESIAN_POINT('Ctrl Pts',(-1.83120816955645,1.,-3.77038509817999));
#47926=CARTESIAN_POINT('Ctrl Pts',(-1.83493697934534,1.,-3.77326886064398));
#47927=CARTESIAN_POINT('Ctrl Pts',(-1.83742834010626,1.,-3.77518714457833));
#47928=CARTESIAN_POINT('Ctrl Pts',(-1.83867539237861,1.,-3.77614523045147));
#47929=CARTESIAN_POINT('Origin',(-1.83867539237861,0.,-3.77614523045147));
#47930=CARTESIAN_POINT('',(-1.97421938526992,1.,-3.70708211654725));
#47931=CARTESIAN_POINT('Origin',(0.,0.,0.));
#47932=CARTESIAN_POINT('',(-1.35032489087269,1.,-3.49844575334386));
#47933=CARTESIAN_POINT('Origin',(0.,1.,0.));
#47934=CARTESIAN_POINT('Ctrl Pts',(-1.35032489087269,1.,-3.49844575334386));
#47935=CARTESIAN_POINT('Ctrl Pts',(-1.35032489087269,0.666666666666667,
-3.49844575334386));
#47936=CARTESIAN_POINT('Ctrl Pts',(-1.35032489087269,0.333333333333333,
-3.49844575334386));
#47937=CARTESIAN_POINT('Ctrl Pts',(-1.35032489087269,-0.333333333333333,
-3.49844575334386));
#47938=CARTESIAN_POINT('Ctrl Pts',(-1.35032489087269,-0.666666666666667,
-3.49844575334386));
#47939=CARTESIAN_POINT('Ctrl Pts',(-1.35032489087269,-1.,-3.49844575334386));
#47940=CARTESIAN_POINT('Ctrl Pts',(-1.36999806084572,-1.,-3.97027773754922));
#47941=CARTESIAN_POINT('Ctrl Pts',(-1.36999806084572,1.,-3.97027773754922));
#47942=CARTESIAN_POINT('Ctrl Pts',(-1.37020239094758,-1.,-3.9687184694173));
#47943=CARTESIAN_POINT('Ctrl Pts',(-1.37020239094758,1.,-3.9687184694173));
#47944=CARTESIAN_POINT('Ctrl Pts',(-1.37060761746027,-1.,-3.96560037975788));
#47945=CARTESIAN_POINT('Ctrl Pts',(-1.37060761746027,1.,-3.96560037975788));
#47946=CARTESIAN_POINT('Ctrl Pts',(-1.37120515615663,-1.,-3.96092458508407));
#47947=CARTESIAN_POINT('Ctrl Pts',(-1.37120515615663,1.,-3.96092458508407));
#47948=CARTESIAN_POINT('Ctrl Pts',(-1.37198126433139,-1.,-3.95469287283105));
#47949=CARTESIAN_POINT('Ctrl Pts',(-1.37198126433139,1.,-3.95469287283105));
#47950=CARTESIAN_POINT('Ctrl Pts',(-1.37291699203423,-1.,-3.94690771786926));
#47951=CARTESIAN_POINT('Ctrl Pts',(-1.37291699203423,1.,-3.94690771786926));
#47952=CARTESIAN_POINT('Ctrl Pts',(-1.37381821967499,-1.,-3.93912709041791));
#47953=CARTESIAN_POINT('Ctrl Pts',(-1.37381821967499,1.,-3.93912709041791));
#47954=CARTESIAN_POINT('Ctrl Pts',(-1.37468482215784,-1.,-3.93135106761941));
#47955=CARTESIAN_POINT('Ctrl Pts',(-1.37468482215784,1.,-3.93135106761941));
#47956=CARTESIAN_POINT('Ctrl Pts',(-1.37551664448057,-1.,-3.92357976987132));
#47957=CARTESIAN_POINT('Ctrl Pts',(-1.37551664448057,1.,-3.92357976987132));
#47958=CARTESIAN_POINT('Ctrl Pts',(-1.37631350505516,-1.,-3.91581337461825));
#47959=CARTESIAN_POINT('Ctrl Pts',(-1.37631350505516,1.,-3.91581337461825));
#47960=CARTESIAN_POINT('Ctrl Pts',(-1.3770751963376,-1.,-3.90805209522729));
#47961=CARTESIAN_POINT('Ctrl Pts',(-1.3770751963376,1.,-3.90805209522729));
#47962=CARTESIAN_POINT('Ctrl Pts',(-1.3778014851263,-1.,-3.90029615196255));
#47963=CARTESIAN_POINT('Ctrl Pts',(-1.3778014851263,1.,-3.90029615196255));
#47964=CARTESIAN_POINT('Ctrl Pts',(-1.37849211287981,-1.,-3.89254574338385));
#47965=CARTESIAN_POINT('Ctrl Pts',(-1.37849211287981,1.,-3.89254574338385));
#47966=CARTESIAN_POINT('Ctrl Pts',(-1.37914679719446,-1.,-3.88480102249461));
#47967=CARTESIAN_POINT('Ctrl Pts',(-1.37914679719446,1.,-3.88480102249461));
#47968=CARTESIAN_POINT('Ctrl Pts',(-1.37976523097187,-1.,-3.87706205830865));
#47969=CARTESIAN_POINT('Ctrl Pts',(-1.37976523097187,1.,-3.87706205830865));
#47970=CARTESIAN_POINT('Ctrl Pts',(-1.38034709213129,-1.,-3.86932885813403));
#47971=CARTESIAN_POINT('Ctrl Pts',(-1.38034709213129,1.,-3.86932885813403));
#47972=CARTESIAN_POINT('Ctrl Pts',(-1.38089205993067,-1.,-3.86160143044187));
#47973=CARTESIAN_POINT('Ctrl Pts',(-1.38089205993067,1.,-3.86160143044187));
#47974=CARTESIAN_POINT('Ctrl Pts',(-1.38139983115075,-1.,-3.85387983979557));
#47975=CARTESIAN_POINT('Ctrl Pts',(-1.38139983115075,1.,-3.85387983979557));
#47976=CARTESIAN_POINT('Ctrl Pts',(-1.38187013346089,-1.,-3.84616425605705));
#47977=CARTESIAN_POINT('Ctrl Pts',(-1.38187013346089,1.,-3.84616425605705));
#47978=CARTESIAN_POINT('Ctrl Pts',(-1.38230274828774,-1.,-3.83845502790609));
#47979=CARTESIAN_POINT('Ctrl Pts',(-1.38230274828774,1.,-3.83845502790609));
#47980=CARTESIAN_POINT('Ctrl Pts',(-1.38269750245086,-1.,-3.83075266982138));
#47981=CARTESIAN_POINT('Ctrl Pts',(-1.38269750245086,1.,-3.83075266982138));
#47982=CARTESIAN_POINT('Ctrl Pts',(-1.38305421262724,-1.,-3.82305771743715));
#47983=CARTESIAN_POINT('Ctrl Pts',(-1.38305421262724,1.,-3.82305771743715));
#47984=CARTESIAN_POINT('Ctrl Pts',(-1.38337263902766,-1.,-3.81537060817765));
#47985=CARTESIAN_POINT('Ctrl Pts',(-1.38337263902766,1.,-3.81537060817765));
#47986=CARTESIAN_POINT('Ctrl Pts',(-1.38365244046226,-1.,-3.80769156398429));
#47987=CARTESIAN_POINT('Ctrl Pts',(-1.38365244046226,1.,-3.80769156398429));
#47988=CARTESIAN_POINT('Ctrl Pts',(-1.38389311766701,-1.,-3.80002044322169));
#47989=CARTESIAN_POINT('Ctrl Pts',(-1.38389311766701,1.,-3.80002044322169));
#47990=CARTESIAN_POINT('Ctrl Pts',(-1.38409399694589,-1.,-3.79235669640907));
#47991=CARTESIAN_POINT('Ctrl Pts',(-1.38409399694589,1.,-3.79235669640907));
#47992=CARTESIAN_POINT('Ctrl Pts',(-1.38425435883773,-1.,-3.78469969805134));
#47993=CARTESIAN_POINT('Ctrl Pts',(-1.38425435883773,1.,-3.78469969805134));
#47994=CARTESIAN_POINT('Ctrl Pts',(-1.38437354551435,-1.,-3.77704902230441));
#47995=CARTESIAN_POINT('Ctrl Pts',(-1.38437354551435,1.,-3.77704902230441));
#47996=CARTESIAN_POINT('Ctrl Pts',(-1.38445107339517,-1.,-3.76940473185775));
#47997=CARTESIAN_POINT('Ctrl Pts',(-1.38445107339517,1.,-3.76940473185775));
#47998=CARTESIAN_POINT('Ctrl Pts',(-1.38448675253343,-1.,-3.76176768271347));
#47999=CARTESIAN_POINT('Ctrl Pts',(-1.38448675253343,1.,-3.76176768271347));
#48000=CARTESIAN_POINT('Ctrl Pts',(-1.38448077997155,-1.,-3.75413976318727));
#48001=CARTESIAN_POINT('Ctrl Pts',(-1.38448077997155,1.,-3.75413976318727));
#48002=CARTESIAN_POINT('Ctrl Pts',(-1.38443344984389,-1.,-3.7465231716786));
#48003=CARTESIAN_POINT('Ctrl Pts',(-1.38443344984389,1.,-3.7465231716786));
#48004=CARTESIAN_POINT('Ctrl Pts',(-1.38434489156456,-1.,-3.73891976418099));
#48005=CARTESIAN_POINT('Ctrl Pts',(-1.38434489156456,1.,-3.73891976418099));
#48006=CARTESIAN_POINT('Ctrl Pts',(-1.38421479111531,-1.,-3.73133035859283));
#48007=CARTESIAN_POINT('Ctrl Pts',(-1.38421479111531,1.,-3.73133035859283));
#48008=CARTESIAN_POINT('Ctrl Pts',(-1.3840421342895,-1.,-3.72375409358805));
#48009=CARTESIAN_POINT('Ctrl Pts',(-1.3840421342895,1.,-3.72375409358805));
#48010=CARTESIAN_POINT('Ctrl Pts',(-1.38382489984585,-1.,-3.7161876605181));
#48011=CARTESIAN_POINT('Ctrl Pts',(-1.38382489984585,1.,-3.7161876605181));
#48012=CARTESIAN_POINT('Ctrl Pts',(-1.38356065402122,-1.,-3.70862680753343));
#48013=CARTESIAN_POINT('Ctrl Pts',(-1.38356065402122,1.,-3.70862680753343));
#48014=CARTESIAN_POINT('Ctrl Pts',(-1.38324717612862,-1.,-3.70106792167894));
#48015=CARTESIAN_POINT('Ctrl Pts',(-1.38324717612862,1.,-3.70106792167894));
#48016=CARTESIAN_POINT('Ctrl Pts',(-1.38288311171649,-1.,-3.69350967899523));
#48017=CARTESIAN_POINT('Ctrl Pts',(-1.38288311171649,1.,-3.69350967899523));
#48018=CARTESIAN_POINT('Ctrl Pts',(-1.38246852827185,-1.,-3.68595444983844));
#48019=CARTESIAN_POINT('Ctrl Pts',(-1.38246852827185,1.,-3.68595444983844));
#48020=CARTESIAN_POINT('Ctrl Pts',(-1.38200574290626,-1.,-3.6784103848243));
#48021=CARTESIAN_POINT('Ctrl Pts',(-1.38200574290626,1.,-3.6784103848243));
#48022=CARTESIAN_POINT('Ctrl Pts',(-1.38149812653876,-1.,-3.67088843112282));
#48023=CARTESIAN_POINT('Ctrl Pts',(-1.38149812653876,1.,-3.67088843112282));
#48024=CARTESIAN_POINT('Ctrl Pts',(-1.38094856333558,-1.,-3.66339848520874));
#48025=CARTESIAN_POINT('Ctrl Pts',(-1.38094856333558,1.,-3.66339848520874));
#48026=CARTESIAN_POINT('Ctrl Pts',(-1.38035791051215,-1.,-3.65594554404396));
#48027=CARTESIAN_POINT('Ctrl Pts',(-1.38035791051215,1.,-3.65594554404396));
#48028=CARTESIAN_POINT('Ctrl Pts',(-1.37972372481598,-1.,-3.64852652756444));
#48029=CARTESIAN_POINT('Ctrl Pts',(-1.37972372481598,1.,-3.64852652756444));
#48030=CARTESIAN_POINT('Ctrl Pts',(-1.37903818567347,-1.,-3.64112507791112));
#48031=CARTESIAN_POINT('Ctrl Pts',(-1.37903818567347,1.,-3.64112507791112));
#48032=CARTESIAN_POINT('Ctrl Pts',(-1.37829035457324,-1.,-3.63371727442448));
#48033=CARTESIAN_POINT('Ctrl Pts',(-1.37829035457324,1.,-3.63371727442448));
#48034=CARTESIAN_POINT('Ctrl Pts',(-1.37746987919868,-1.,-3.62628098665112));
#48035=CARTESIAN_POINT('Ctrl Pts',(-1.37746987919868,1.,-3.62628098665112));
#48036=CARTESIAN_POINT('Ctrl Pts',(-1.37657053403102,-1.,-3.61880481160408));
#48037=CARTESIAN_POINT('Ctrl Pts',(-1.37657053403102,1.,-3.61880481160408));
#48038=CARTESIAN_POINT('Ctrl Pts',(-1.37559314436641,-1.,-3.61129546591082));
#48039=CARTESIAN_POINT('Ctrl Pts',(-1.37559314436641,1.,-3.61129546591082));
#48040=CARTESIAN_POINT('Ctrl Pts',(-1.37455051379642,-1.,-3.60379020124038));
#48041=CARTESIAN_POINT('Ctrl Pts',(-1.37455051379642,1.,-3.60379020124038));
#48042=CARTESIAN_POINT('Ctrl Pts',(-1.37346320103184,-1.,-3.59634627869117));
#48043=CARTESIAN_POINT('Ctrl Pts',(-1.37346320103184,1.,-3.59634627869117));
#48044=CARTESIAN_POINT('Ctrl Pts',(-1.37235053661,-1.,-3.5890185384643));
#48045=CARTESIAN_POINT('Ctrl Pts',(-1.37235053661,1.,-3.5890185384643));
#48046=CARTESIAN_POINT('Ctrl Pts',(-1.37122241663073,-1.,-3.58183885982745));
#48047=CARTESIAN_POINT('Ctrl Pts',(-1.37122241663073,1.,-3.58183885982745));
#48048=CARTESIAN_POINT('Ctrl Pts',(-1.37007229485646,-1.,-3.57479875549453));
#48049=CARTESIAN_POINT('Ctrl Pts',(-1.37007229485646,1.,-3.57479875549453));
#48050=CARTESIAN_POINT('Ctrl Pts',(-1.36886584973349,-1.,-3.56782080304554));
#48051=CARTESIAN_POINT('Ctrl Pts',(-1.36886584973349,1.,-3.56782080304554));
#48052=CARTESIAN_POINT('Ctrl Pts',(-1.36754771771174,-1.,-3.56077662028492));
#48053=CARTESIAN_POINT('Ctrl Pts',(-1.36754771771174,1.,-3.56077662028492));
#48054=CARTESIAN_POINT('Ctrl Pts',(-1.36606145456711,-1.,-3.55353883995793));
#48055=CARTESIAN_POINT('Ctrl Pts',(-1.36606145456711,1.,-3.55353883995793));
#48056=CARTESIAN_POINT('Ctrl Pts',(-1.36436666257567,-1.,-3.54602591832893));
#48057=CARTESIAN_POINT('Ctrl Pts',(-1.36436666257567,1.,-3.54602591832893));
#48058=CARTESIAN_POINT('Ctrl Pts',(-1.36245507339334,-1.,-3.53824396425032));
#48059=CARTESIAN_POINT('Ctrl Pts',(-1.36245507339334,1.,-3.53824396425032));
#48060=CARTESIAN_POINT('Ctrl Pts',(-1.36037259643827,-1.,-3.53034464961849));
#48061=CARTESIAN_POINT('Ctrl Pts',(-1.36037259643827,1.,-3.53034464961849));
#48062=CARTESIAN_POINT('Ctrl Pts',(-1.35821701528975,-1.,-3.52261776117121));
#48063=CARTESIAN_POINT('Ctrl Pts',(-1.35821701528975,1.,-3.52261776117121));
#48064=CARTESIAN_POINT('Ctrl Pts',(-1.35611275237288,-1.,-3.51542230699919));
#48065=CARTESIAN_POINT('Ctrl Pts',(-1.35611275237288,1.,-3.51542230699919));
#48066=CARTESIAN_POINT('Ctrl Pts',(-1.35419113576022,-1.,-3.50913227060177));
#48067=CARTESIAN_POINT('Ctrl Pts',(-1.35419113576022,1.,-3.50913227060177));
#48068=CARTESIAN_POINT('Ctrl Pts',(-1.3525703284343,-1.,-3.50408168106113));
#48069=CARTESIAN_POINT('Ctrl Pts',(-1.3525703284343,1.,-3.50408168106113));
#48070=CARTESIAN_POINT('Ctrl Pts',(-1.35133076331065,-1.,-3.50049707063673));
#48071=CARTESIAN_POINT('Ctrl Pts',(-1.35133076331065,1.,-3.50049707063673));
#48072=CARTESIAN_POINT('Ctrl Pts',(-1.35067437417289,-1.,-3.49888720256612));
#48073=CARTESIAN_POINT('Ctrl Pts',(-1.35067437417289,1.,-3.49888720256612));
#48074=CARTESIAN_POINT('Ctrl Pts',(-1.35037650302887,-1.,-3.49840357193384));
#48075=CARTESIAN_POINT('Ctrl Pts',(-1.35037650302887,1.,-3.49840357193384));
#48076=CARTESIAN_POINT('Ctrl Pts',(-1.35026426118351,-1.,-3.49840260053616));
#48077=CARTESIAN_POINT('Ctrl Pts',(-1.35026426118351,1.,-3.49840260053616));
#48078=CARTESIAN_POINT('Ctrl Pts',(-1.35022972712301,-1.,-3.49848248301936));
#48079=CARTESIAN_POINT('Ctrl Pts',(-1.35022972712301,1.,-3.49848248301936));
#48080=CARTESIAN_POINT('',(-1.36999806084572,1.,-3.97027773754922));
#48081=CARTESIAN_POINT('Ctrl Pts',(-1.36999806084572,1.,-3.97027773754922));
#48082=CARTESIAN_POINT('Ctrl Pts',(-1.37020239094758,1.,-3.9687184694173));
#48083=CARTESIAN_POINT('Ctrl Pts',(-1.37060761746027,1.,-3.96560037975788));
#48084=CARTESIAN_POINT('Ctrl Pts',(-1.37120515615663,1.,-3.96092458508407));
#48085=CARTESIAN_POINT('Ctrl Pts',(-1.37198126433139,1.,-3.95469287283105));
#48086=CARTESIAN_POINT('Ctrl Pts',(-1.37291699203423,1.,-3.94690771786926));
#48087=CARTESIAN_POINT('Ctrl Pts',(-1.37381821967499,1.,-3.93912709041791));
#48088=CARTESIAN_POINT('Ctrl Pts',(-1.37468482215784,1.,-3.93135106761941));
#48089=CARTESIAN_POINT('Ctrl Pts',(-1.37551664448057,1.,-3.92357976987132));
#48090=CARTESIAN_POINT('Ctrl Pts',(-1.37631350505516,1.,-3.91581337461825));
#48091=CARTESIAN_POINT('Ctrl Pts',(-1.3770751963376,1.,-3.90805209522729));
#48092=CARTESIAN_POINT('Ctrl Pts',(-1.3778014851263,1.,-3.90029615196255));
#48093=CARTESIAN_POINT('Ctrl Pts',(-1.37849211287981,1.,-3.89254574338385));
#48094=CARTESIAN_POINT('Ctrl Pts',(-1.37914679719446,1.,-3.88480102249461));
#48095=CARTESIAN_POINT('Ctrl Pts',(-1.37976523097187,1.,-3.87706205830865));
#48096=CARTESIAN_POINT('Ctrl Pts',(-1.38034709213129,1.,-3.86932885813403));
#48097=CARTESIAN_POINT('Ctrl Pts',(-1.38089205993067,1.,-3.86160143044187));
#48098=CARTESIAN_POINT('Ctrl Pts',(-1.38139983115075,1.,-3.85387983979557));
#48099=CARTESIAN_POINT('Ctrl Pts',(-1.38187013346089,1.,-3.84616425605705));
#48100=CARTESIAN_POINT('Ctrl Pts',(-1.38230274828774,1.,-3.83845502790609));
#48101=CARTESIAN_POINT('Ctrl Pts',(-1.38269750245086,1.,-3.83075266982138));
#48102=CARTESIAN_POINT('Ctrl Pts',(-1.38305421262724,1.,-3.82305771743715));
#48103=CARTESIAN_POINT('Ctrl Pts',(-1.38337263902766,1.,-3.81537060817765));
#48104=CARTESIAN_POINT('Ctrl Pts',(-1.38365244046226,1.,-3.80769156398429));
#48105=CARTESIAN_POINT('Ctrl Pts',(-1.38389311766701,1.,-3.80002044322169));
#48106=CARTESIAN_POINT('Ctrl Pts',(-1.38409399694589,1.,-3.79235669640907));
#48107=CARTESIAN_POINT('Ctrl Pts',(-1.38425435883773,1.,-3.78469969805134));
#48108=CARTESIAN_POINT('Ctrl Pts',(-1.38437354551435,1.,-3.77704902230441));
#48109=CARTESIAN_POINT('Ctrl Pts',(-1.38445107339517,1.,-3.76940473185775));
#48110=CARTESIAN_POINT('Ctrl Pts',(-1.38448675253343,1.,-3.76176768271347));
#48111=CARTESIAN_POINT('Ctrl Pts',(-1.38448077997155,1.,-3.75413976318727));
#48112=CARTESIAN_POINT('Ctrl Pts',(-1.38443344984389,1.,-3.7465231716786));
#48113=CARTESIAN_POINT('Ctrl Pts',(-1.38434489156456,1.,-3.73891976418099));
#48114=CARTESIAN_POINT('Ctrl Pts',(-1.38421479111531,1.,-3.73133035859283));
#48115=CARTESIAN_POINT('Ctrl Pts',(-1.3840421342895,1.,-3.72375409358805));
#48116=CARTESIAN_POINT('Ctrl Pts',(-1.38382489984585,1.,-3.7161876605181));
#48117=CARTESIAN_POINT('Ctrl Pts',(-1.38356065402122,1.,-3.70862680753343));
#48118=CARTESIAN_POINT('Ctrl Pts',(-1.38324717612862,1.,-3.70106792167894));
#48119=CARTESIAN_POINT('Ctrl Pts',(-1.38288311171649,1.,-3.69350967899523));
#48120=CARTESIAN_POINT('Ctrl Pts',(-1.38246852827185,1.,-3.68595444983844));
#48121=CARTESIAN_POINT('Ctrl Pts',(-1.38200574290626,1.,-3.6784103848243));
#48122=CARTESIAN_POINT('Ctrl Pts',(-1.38149812653876,1.,-3.67088843112282));
#48123=CARTESIAN_POINT('Ctrl Pts',(-1.38094856333558,1.,-3.66339848520874));
#48124=CARTESIAN_POINT('Ctrl Pts',(-1.38035791051215,1.,-3.65594554404396));
#48125=CARTESIAN_POINT('Ctrl Pts',(-1.37972372481598,1.,-3.64852652756444));
#48126=CARTESIAN_POINT('Ctrl Pts',(-1.37903818567347,1.,-3.64112507791112));
#48127=CARTESIAN_POINT('Ctrl Pts',(-1.37829035457324,1.,-3.63371727442448));
#48128=CARTESIAN_POINT('Ctrl Pts',(-1.37746987919868,1.,-3.62628098665112));
#48129=CARTESIAN_POINT('Ctrl Pts',(-1.37657053403102,1.,-3.61880481160408));
#48130=CARTESIAN_POINT('Ctrl Pts',(-1.37559314436641,1.,-3.61129546591082));
#48131=CARTESIAN_POINT('Ctrl Pts',(-1.37455051379642,1.,-3.60379020124038));
#48132=CARTESIAN_POINT('Ctrl Pts',(-1.37346320103184,1.,-3.59634627869117));
#48133=CARTESIAN_POINT('Ctrl Pts',(-1.37235053661,1.,-3.5890185384643));
#48134=CARTESIAN_POINT('Ctrl Pts',(-1.37122241663073,1.,-3.58183885982745));
#48135=CARTESIAN_POINT('Ctrl Pts',(-1.37007229485646,1.,-3.57479875549453));
#48136=CARTESIAN_POINT('Ctrl Pts',(-1.36886584973349,1.,-3.56782080304554));
#48137=CARTESIAN_POINT('Ctrl Pts',(-1.36754771771174,1.,-3.56077662028492));
#48138=CARTESIAN_POINT('Ctrl Pts',(-1.36606145456711,1.,-3.55353883995793));
#48139=CARTESIAN_POINT('Ctrl Pts',(-1.36436666257567,1.,-3.54602591832893));
#48140=CARTESIAN_POINT('Ctrl Pts',(-1.36245507339334,1.,-3.53824396425032));
#48141=CARTESIAN_POINT('Ctrl Pts',(-1.36037259643827,1.,-3.53034464961849));
#48142=CARTESIAN_POINT('Ctrl Pts',(-1.35821701528975,1.,-3.52261776117121));
#48143=CARTESIAN_POINT('Ctrl Pts',(-1.35611275237288,1.,-3.51542230699919));
#48144=CARTESIAN_POINT('Ctrl Pts',(-1.35419113576022,1.,-3.50913227060177));
#48145=CARTESIAN_POINT('Ctrl Pts',(-1.3525703284343,1.,-3.50408168106113));
#48146=CARTESIAN_POINT('Ctrl Pts',(-1.35142377279535,1.,-3.5007660381658));
#48147=CARTESIAN_POINT('Ctrl Pts',(-1.35080045218652,1.,-3.49920025459856));
#48148=CARTESIAN_POINT('Ctrl Pts',(-1.35049736560633,1.,-3.49861894124915));
#48149=CARTESIAN_POINT('Ctrl Pts',(-1.35036670893102,1.,-3.49847119623841));
#48150=CARTESIAN_POINT('Ctrl Pts',(-1.35032489087269,1.,-3.49844575334386));
#48151=CARTESIAN_POINT('',(-1.36999806084572,0.,-3.97027773754922));
#48152=CARTESIAN_POINT('Ctrl Pts',(-0.96399761336957,-1.,-3.62397690409552));
#48153=CARTESIAN_POINT('Ctrl Pts',(-0.96399761336957,1.,-3.62397690409552));
#48154=CARTESIAN_POINT('Ctrl Pts',(-0.963922720982576,-1.,-3.62393257642191));
#48155=CARTESIAN_POINT('Ctrl Pts',(-0.963922720982576,1.,-3.62393257642191));
#48156=CARTESIAN_POINT('Ctrl Pts',(-0.963832486396055,-1.,-3.62399933640277));
#48157=CARTESIAN_POINT('Ctrl Pts',(-0.963832486396055,1.,-3.62399933640277));
#48158=CARTESIAN_POINT('Ctrl Pts',(-0.963875774532103,-1.,-3.62456568607055));
#48159=CARTESIAN_POINT('Ctrl Pts',(-0.963875774532103,1.,-3.62456568607055));
#48160=CARTESIAN_POINT('Ctrl Pts',(-0.964291001274618,-1.,-3.62625391255277));
#48161=CARTESIAN_POINT('Ctrl Pts',(-0.964291001274618,1.,-3.62625391255277));
#48162=CARTESIAN_POINT('Ctrl Pts',(-0.965395153165716,-1.,-3.62988252139998));
#48163=CARTESIAN_POINT('Ctrl Pts',(-0.965395153165716,1.,-3.62988252139998));
#48164=CARTESIAN_POINT('Ctrl Pts',(-0.967052554540877,-1.,-3.6349212208096));
#48165=CARTESIAN_POINT('Ctrl Pts',(-0.967052554540877,1.,-3.6349212208096));
#48166=CARTESIAN_POINT('Ctrl Pts',(-0.969195124674829,-1.,-3.64113946505393));
#48167=CARTESIAN_POINT('Ctrl Pts',(-0.969195124674829,1.,-3.64113946505393));
#48168=CARTESIAN_POINT('Ctrl Pts',(-0.971722122060277,-1.,-3.64819756447072));
#48169=CARTESIAN_POINT('Ctrl Pts',(-0.971722122060277,1.,-3.64819756447072));
#48170=CARTESIAN_POINT('Ctrl Pts',(-0.974519971354139,-1.,-3.6557157673487));
#48171=CARTESIAN_POINT('Ctrl Pts',(-0.974519971354139,1.,-3.6557157673487));
#48172=CARTESIAN_POINT('Ctrl Pts',(-0.977478312751416,-1.,-3.66333049637403));
#48173=CARTESIAN_POINT('Ctrl Pts',(-0.977478312751416,1.,-3.66333049637403));
#48174=CARTESIAN_POINT('Ctrl Pts',(-0.980505922458494,-1.,-3.67074983340444));
#48175=CARTESIAN_POINT('Ctrl Pts',(-0.980505922458494,1.,-3.67074983340444));
#48176=CARTESIAN_POINT('Ctrl Pts',(-0.983550791470864,-1.,-3.67782408841876));
#48177=CARTESIAN_POINT('Ctrl Pts',(-0.983550791470864,1.,-3.67782408841876));
#48178=CARTESIAN_POINT('Ctrl Pts',(-0.986602639864286,-1.,-3.6845531792623));
#48179=CARTESIAN_POINT('Ctrl Pts',(-0.986602639864286,1.,-3.6845531792623));
#48180=CARTESIAN_POINT('Ctrl Pts',(-0.989676715398858,-1.,-3.69102682138955));
#48181=CARTESIAN_POINT('Ctrl Pts',(-0.989676715398858,1.,-3.69102682138955));
#48182=CARTESIAN_POINT('Ctrl Pts',(-0.992802218332104,-1.,-3.69738123415696));
#48183=CARTESIAN_POINT('Ctrl Pts',(-0.992802218332104,1.,-3.69738123415696));
#48184=CARTESIAN_POINT('Ctrl Pts',(-0.996009819772432,-1.,-3.70375282282107));
#48185=CARTESIAN_POINT('Ctrl Pts',(-0.996009819772432,1.,-3.70375282282107));
#48186=CARTESIAN_POINT('Ctrl Pts',(-0.999317260756344,-1.,-3.7102243971387));
#48187=CARTESIAN_POINT('Ctrl Pts',(-0.999317260756344,1.,-3.7102243971387));
#48188=CARTESIAN_POINT('Ctrl Pts',(-1.00272423396802,-1.,-3.71680667125047));
#48189=CARTESIAN_POINT('Ctrl Pts',(-1.00272423396802,1.,-3.71680667125047));
#48190=CARTESIAN_POINT('Ctrl Pts',(-1.00622000735696,-1.,-3.72346803750544));
#48191=CARTESIAN_POINT('Ctrl Pts',(-1.00622000735696,1.,-3.72346803750544));
#48192=CARTESIAN_POINT('Ctrl Pts',(-1.00978798539491,-1.,-3.73015276704407));
#48193=CARTESIAN_POINT('Ctrl Pts',(-1.00978798539491,1.,-3.73015276704407));
#48194=CARTESIAN_POINT('Ctrl Pts',(-1.01341114319906,-1.,-3.73680245055747));
#48195=CARTESIAN_POINT('Ctrl Pts',(-1.01341114319906,1.,-3.73680245055747));
#48196=CARTESIAN_POINT('Ctrl Pts',(-1.01707794311088,-1.,-3.74337942504993));
#48197=CARTESIAN_POINT('Ctrl Pts',(-1.01707794311088,1.,-3.74337942504993));
#48198=CARTESIAN_POINT('Ctrl Pts',(-1.02078510487439,-1.,-3.74987777155873));
#48199=CARTESIAN_POINT('Ctrl Pts',(-1.02078510487439,1.,-3.74987777155873));
#48200=CARTESIAN_POINT('Ctrl Pts',(-1.02453429444668,-1.,-3.75631037456224));
#48201=CARTESIAN_POINT('Ctrl Pts',(-1.02453429444668,1.,-3.75631037456224));
#48202=CARTESIAN_POINT('Ctrl Pts',(-1.02833014458184,-1.,-3.76270122291245));
#48203=CARTESIAN_POINT('Ctrl Pts',(-1.02833014458184,1.,-3.76270122291245));
#48204=CARTESIAN_POINT('Ctrl Pts',(-1.03217786604919,-1.,-3.76907609832516));
#48205=CARTESIAN_POINT('Ctrl Pts',(-1.03217786604919,1.,-3.76907609832516));
#48206=CARTESIAN_POINT('Ctrl Pts',(-1.03608074678008,-1.,-3.77545283140427));
#48207=CARTESIAN_POINT('Ctrl Pts',(-1.03608074678008,1.,-3.77545283140427));
#48208=CARTESIAN_POINT('Ctrl Pts',(-1.04003862055798,-1.,-3.7818353500817));
#48209=CARTESIAN_POINT('Ctrl Pts',(-1.04003862055798,1.,-3.7818353500817));
#48210=CARTESIAN_POINT('Ctrl Pts',(-1.04404924374422,-1.,-3.78821910787179));
#48211=CARTESIAN_POINT('Ctrl Pts',(-1.04404924374422,1.,-3.78821910787179));
#48212=CARTESIAN_POINT('Ctrl Pts',(-1.04810913267639,-1.,-3.79459440308786));
#48213=CARTESIAN_POINT('Ctrl Pts',(-1.04810913267639,1.,-3.79459440308786));
#48214=CARTESIAN_POINT('Ctrl Pts',(-1.05221457990016,-1.,-3.80095039790681));
#48215=CARTESIAN_POINT('Ctrl Pts',(-1.05221457990016,1.,-3.80095039790681));
#48216=CARTESIAN_POINT('Ctrl Pts',(-1.05636266918644,-1.,-3.80727913637791));
#48217=CARTESIAN_POINT('Ctrl Pts',(-1.05636266918644,1.,-3.80727913637791));
#48218=CARTESIAN_POINT('Ctrl Pts',(-1.06055206187299,-1.,-3.8135786611749));
#48219=CARTESIAN_POINT('Ctrl Pts',(-1.06055206187299,1.,-3.8135786611749));
#48220=CARTESIAN_POINT('Ctrl Pts',(-1.0647824403893,-1.,-3.81985083953012));
#48221=CARTESIAN_POINT('Ctrl Pts',(-1.0647824403893,1.,-3.81985083953012));
#48222=CARTESIAN_POINT('Ctrl Pts',(-1.06905413180359,-1.,-3.82609989967276));
#48223=CARTESIAN_POINT('Ctrl Pts',(-1.06905413180359,1.,-3.82609989967276));
#48224=CARTESIAN_POINT('Ctrl Pts',(-1.07336766633459,-1.,-3.83233071195144));
#48225=CARTESIAN_POINT('Ctrl Pts',(-1.07336766633459,1.,-3.83233071195144));
#48226=CARTESIAN_POINT('Ctrl Pts',(-1.07772335353858,-1.,-3.83854714117491));
#48227=CARTESIAN_POINT('Ctrl Pts',(-1.07772335353858,1.,-3.83854714117491));
#48228=CARTESIAN_POINT('Ctrl Pts',(-1.08212087917991,-1.,-3.8447504803063));
#48229=CARTESIAN_POINT('Ctrl Pts',(-1.08212087917991,1.,-3.8447504803063));
#48230=CARTESIAN_POINT('Ctrl Pts',(-1.08655950846384,-1.,-3.85094025222713));
#48231=CARTESIAN_POINT('Ctrl Pts',(-1.08655950846384,1.,-3.85094025222713));
#48232=CARTESIAN_POINT('Ctrl Pts',(-1.09103825516294,-1.,-3.85711487933931));
#48233=CARTESIAN_POINT('Ctrl Pts',(-1.09103825516294,1.,-3.85711487933931));
#48234=CARTESIAN_POINT('Ctrl Pts',(-1.09555606505013,-1.,-3.86327241021247));
#48235=CARTESIAN_POINT('Ctrl Pts',(-1.09555606505013,1.,-3.86327241021247));
#48236=CARTESIAN_POINT('Ctrl Pts',(-1.10011198761195,-1.,-3.86941120134849));
#48237=CARTESIAN_POINT('Ctrl Pts',(-1.10011198761195,1.,-3.86941120134849));
#48238=CARTESIAN_POINT('Ctrl Pts',(-1.10470536603287,-1.,-3.87553067187514));
#48239=CARTESIAN_POINT('Ctrl Pts',(-1.10470536603287,1.,-3.87553067187514));
#48240=CARTESIAN_POINT('Ctrl Pts',(-1.10933577224008,-1.,-3.88163105531724));
#48241=CARTESIAN_POINT('Ctrl Pts',(-1.10933577224008,1.,-3.88163105531724));
#48242=CARTESIAN_POINT('Ctrl Pts',(-1.11400292434429,-1.,-3.88771308285171));
#48243=CARTESIAN_POINT('Ctrl Pts',(-1.11400292434429,1.,-3.88771308285171));
#48244=CARTESIAN_POINT('Ctrl Pts',(-1.11870660794603,-1.,-3.89377768340344));
#48245=CARTESIAN_POINT('Ctrl Pts',(-1.11870660794603,1.,-3.89377768340344));
#48246=CARTESIAN_POINT('Ctrl Pts',(-1.12344660099043,-1.,-3.89982569750025));
#48247=CARTESIAN_POINT('Ctrl Pts',(-1.12344660099043,1.,-3.89982569750025));
#48248=CARTESIAN_POINT('Ctrl Pts',(-1.12822258281553,-1.,-3.90585753318737));
#48249=CARTESIAN_POINT('Ctrl Pts',(-1.12822258281553,1.,-3.90585753318737));
#48250=CARTESIAN_POINT('Ctrl Pts',(-1.13303414693896,-1.,-3.91187321145649));
#48251=CARTESIAN_POINT('Ctrl Pts',(-1.13303414693896,1.,-3.91187321145649));
#48252=CARTESIAN_POINT('Ctrl Pts',(-1.13788084225554,-1.,-3.91787251936827));
#48253=CARTESIAN_POINT('Ctrl Pts',(-1.13788084225554,1.,-3.91787251936827));
#48254=CARTESIAN_POINT('Ctrl Pts',(-1.14276220561593,-1.,-3.92385513133997));
#48255=CARTESIAN_POINT('Ctrl Pts',(-1.14276220561593,1.,-3.92385513133997));
#48256=CARTESIAN_POINT('Ctrl Pts',(-1.14767779451123,-1.,-3.92982073294257));
#48257=CARTESIAN_POINT('Ctrl Pts',(-1.14767779451123,1.,-3.92982073294257));
#48258=CARTESIAN_POINT('Ctrl Pts',(-1.1526272271632,-1.,-3.9357691705628));
#48259=CARTESIAN_POINT('Ctrl Pts',(-1.1526272271632,1.,-3.9357691705628));
#48260=CARTESIAN_POINT('Ctrl Pts',(-1.15761018340956,-1.,-3.94170046685203));
#48261=CARTESIAN_POINT('Ctrl Pts',(-1.15761018340956,1.,-3.94170046685203));
#48262=CARTESIAN_POINT('Ctrl Pts',(-1.16262637999157,-1.,-3.94761474780583));
#48263=CARTESIAN_POINT('Ctrl Pts',(-1.16262637999157,1.,-3.94761474780583));
#48264=CARTESIAN_POINT('Ctrl Pts',(-1.16767555244438,-1.,-3.95351219509876));
#48265=CARTESIAN_POINT('Ctrl Pts',(-1.16767555244438,1.,-3.95351219509876));
#48266=CARTESIAN_POINT('Ctrl Pts',(-1.17275743590361,-1.,-3.95939299213276));
#48267=CARTESIAN_POINT('Ctrl Pts',(-1.17275743590361,1.,-3.95939299213276));
#48268=CARTESIAN_POINT('Ctrl Pts',(-1.17787174135592,-1.,-3.96525726358159));
#48269=CARTESIAN_POINT('Ctrl Pts',(-1.17787174135592,1.,-3.96525726358159));
#48270=CARTESIAN_POINT('Ctrl Pts',(-1.18301815039831,-1.,-3.97110505165415));
#48271=CARTESIAN_POINT('Ctrl Pts',(-1.18301815039831,1.,-3.97110505165415));
#48272=CARTESIAN_POINT('Ctrl Pts',(-1.18819633715539,-1.,-3.97693634767754));
#48273=CARTESIAN_POINT('Ctrl Pts',(-1.18819633715539,1.,-3.97693634767754));
#48274=CARTESIAN_POINT('Ctrl Pts',(-1.19340598349475,-1.,-3.98275111052561));
#48275=CARTESIAN_POINT('Ctrl Pts',(-1.19340598349475,1.,-3.98275111052561));
#48276=CARTESIAN_POINT('Ctrl Pts',(-1.19864679609566,-1.,-3.98854928957189));
#48277=CARTESIAN_POINT('Ctrl Pts',(-1.19864679609566,1.,-3.98854928957189));
#48278=CARTESIAN_POINT('Ctrl Pts',(-1.20391852375139,-1.,-3.99433084799666));
#48279=CARTESIAN_POINT('Ctrl Pts',(-1.20391852375139,1.,-3.99433084799666));
#48280=CARTESIAN_POINT('Ctrl Pts',(-1.20922097029551,-1.,-4.00009577950721));
#48281=CARTESIAN_POINT('Ctrl Pts',(-1.20922097029551,1.,-4.00009577950721));
#48282=CARTESIAN_POINT('Ctrl Pts',(-1.21455398918133,-1.,-4.00584409522722));
#48283=CARTESIAN_POINT('Ctrl Pts',(-1.21455398918133,1.,-4.00584409522722));
#48284=CARTESIAN_POINT('Ctrl Pts',(-1.21884478244403,-1.,-4.01042947140789));
#48285=CARTESIAN_POINT('Ctrl Pts',(-1.21884478244403,1.,-4.01042947140789));
#48286=CARTESIAN_POINT('Ctrl Pts',(-1.22207656455845,-1.,-4.01386104433519));
#48287=CARTESIAN_POINT('Ctrl Pts',(-1.22207656455845,1.,-4.01386104433519));
#48288=CARTESIAN_POINT('Ctrl Pts',(-1.22423716681317,-1.,-4.01614544569895));
#48289=CARTESIAN_POINT('Ctrl Pts',(-1.22423716681317,1.,-4.01614544569895));
#48290=CARTESIAN_POINT('Ctrl Pts',(-1.22531898815164,-1.,-4.01728681790024));
#48291=CARTESIAN_POINT('Ctrl Pts',(-1.22531898815164,1.,-4.01728681790024));
#48292=CARTESIAN_POINT('',(-0.963899035118984,1.,-3.62400312501199));
#48293=CARTESIAN_POINT('Ctrl Pts',(-0.963899035118985,-1.,-3.62400312501199));
#48294=CARTESIAN_POINT('Ctrl Pts',(-0.963899035118985,-0.666666666666667,
-3.62400312501199));
#48295=CARTESIAN_POINT('Ctrl Pts',(-0.963899035118985,-0.333333333333333,
-3.62400312501199));
#48296=CARTESIAN_POINT('Ctrl Pts',(-0.963899035118985,0.333333333333333,
-3.62400312501199));
#48297=CARTESIAN_POINT('Ctrl Pts',(-0.963899035118986,0.666666666666667,
-3.62400312501199));
#48298=CARTESIAN_POINT('Ctrl Pts',(-0.963899035118986,1.,-3.62400312501199));
#48299=CARTESIAN_POINT('',(-1.22531898815164,1.,-4.01728681790024));
#48300=CARTESIAN_POINT('',(-1.22531898815164,0.,-4.01728681790024));
#48301=CARTESIAN_POINT('Ctrl Pts',(-0.963899035118985,1.,-3.62400312501199));
#48302=CARTESIAN_POINT('Ctrl Pts',(-0.963880158556713,1.,-3.62404828878375));
#48303=CARTESIAN_POINT('Ctrl Pts',(-0.963861297423579,1.,-3.62424461507455));
#48304=CARTESIAN_POINT('Ctrl Pts',(-0.963957782642589,1.,-3.62489305727516));
#48305=CARTESIAN_POINT('Ctrl Pts',(-0.964373850166081,1.,-3.62652618145252));
#48306=CARTESIAN_POINT('Ctrl Pts',(-0.965395153165716,1.,-3.62988252139998));
#48307=CARTESIAN_POINT('Ctrl Pts',(-0.967052554540877,1.,-3.6349212208096));
#48308=CARTESIAN_POINT('Ctrl Pts',(-0.969195124674829,1.,-3.64113946505393));
#48309=CARTESIAN_POINT('Ctrl Pts',(-0.971722122060277,1.,-3.64819756447072));
#48310=CARTESIAN_POINT('Ctrl Pts',(-0.974519971354139,1.,-3.6557157673487));
#48311=CARTESIAN_POINT('Ctrl Pts',(-0.977478312751416,1.,-3.66333049637403));
#48312=CARTESIAN_POINT('Ctrl Pts',(-0.980505922458494,1.,-3.67074983340444));
#48313=CARTESIAN_POINT('Ctrl Pts',(-0.983550791470864,1.,-3.67782408841876));
#48314=CARTESIAN_POINT('Ctrl Pts',(-0.986602639864286,1.,-3.6845531792623));
#48315=CARTESIAN_POINT('Ctrl Pts',(-0.989676715398858,1.,-3.69102682138955));
#48316=CARTESIAN_POINT('Ctrl Pts',(-0.992802218332104,1.,-3.69738123415696));
#48317=CARTESIAN_POINT('Ctrl Pts',(-0.996009819772432,1.,-3.70375282282107));
#48318=CARTESIAN_POINT('Ctrl Pts',(-0.999317260756344,1.,-3.7102243971387));
#48319=CARTESIAN_POINT('Ctrl Pts',(-1.00272423396802,1.,-3.71680667125047));
#48320=CARTESIAN_POINT('Ctrl Pts',(-1.00622000735696,1.,-3.72346803750544));
#48321=CARTESIAN_POINT('Ctrl Pts',(-1.00978798539491,1.,-3.73015276704407));
#48322=CARTESIAN_POINT('Ctrl Pts',(-1.01341114319906,1.,-3.73680245055747));
#48323=CARTESIAN_POINT('Ctrl Pts',(-1.01707794311088,1.,-3.74337942504993));
#48324=CARTESIAN_POINT('Ctrl Pts',(-1.02078510487439,1.,-3.74987777155873));
#48325=CARTESIAN_POINT('Ctrl Pts',(-1.02453429444668,1.,-3.75631037456224));
#48326=CARTESIAN_POINT('Ctrl Pts',(-1.02833014458184,1.,-3.76270122291245));
#48327=CARTESIAN_POINT('Ctrl Pts',(-1.03217786604919,1.,-3.76907609832516));
#48328=CARTESIAN_POINT('Ctrl Pts',(-1.03608074678008,1.,-3.77545283140427));
#48329=CARTESIAN_POINT('Ctrl Pts',(-1.04003862055798,1.,-3.7818353500817));
#48330=CARTESIAN_POINT('Ctrl Pts',(-1.04404924374422,1.,-3.78821910787179));
#48331=CARTESIAN_POINT('Ctrl Pts',(-1.04810913267639,1.,-3.79459440308786));
#48332=CARTESIAN_POINT('Ctrl Pts',(-1.05221457990016,1.,-3.80095039790681));
#48333=CARTESIAN_POINT('Ctrl Pts',(-1.05636266918644,1.,-3.80727913637791));
#48334=CARTESIAN_POINT('Ctrl Pts',(-1.06055206187299,1.,-3.8135786611749));
#48335=CARTESIAN_POINT('Ctrl Pts',(-1.0647824403893,1.,-3.81985083953012));
#48336=CARTESIAN_POINT('Ctrl Pts',(-1.06905413180359,1.,-3.82609989967276));
#48337=CARTESIAN_POINT('Ctrl Pts',(-1.07336766633459,1.,-3.83233071195144));
#48338=CARTESIAN_POINT('Ctrl Pts',(-1.07772335353858,1.,-3.83854714117491));
#48339=CARTESIAN_POINT('Ctrl Pts',(-1.08212087917991,1.,-3.8447504803063));
#48340=CARTESIAN_POINT('Ctrl Pts',(-1.08655950846384,1.,-3.85094025222713));
#48341=CARTESIAN_POINT('Ctrl Pts',(-1.09103825516294,1.,-3.85711487933931));
#48342=CARTESIAN_POINT('Ctrl Pts',(-1.09555606505013,1.,-3.86327241021247));
#48343=CARTESIAN_POINT('Ctrl Pts',(-1.10011198761195,1.,-3.86941120134849));
#48344=CARTESIAN_POINT('Ctrl Pts',(-1.10470536603287,1.,-3.87553067187514));
#48345=CARTESIAN_POINT('Ctrl Pts',(-1.10933577224008,1.,-3.88163105531724));
#48346=CARTESIAN_POINT('Ctrl Pts',(-1.11400292434429,1.,-3.88771308285171));
#48347=CARTESIAN_POINT('Ctrl Pts',(-1.11870660794603,1.,-3.89377768340344));
#48348=CARTESIAN_POINT('Ctrl Pts',(-1.12344660099043,1.,-3.89982569750025));
#48349=CARTESIAN_POINT('Ctrl Pts',(-1.12822258281553,1.,-3.90585753318737));
#48350=CARTESIAN_POINT('Ctrl Pts',(-1.13303414693896,1.,-3.91187321145649));
#48351=CARTESIAN_POINT('Ctrl Pts',(-1.13788084225554,1.,-3.91787251936827));
#48352=CARTESIAN_POINT('Ctrl Pts',(-1.14276220561593,1.,-3.92385513133997));
#48353=CARTESIAN_POINT('Ctrl Pts',(-1.14767779451123,1.,-3.92982073294257));
#48354=CARTESIAN_POINT('Ctrl Pts',(-1.1526272271632,1.,-3.9357691705628));
#48355=CARTESIAN_POINT('Ctrl Pts',(-1.15761018340956,1.,-3.94170046685203));
#48356=CARTESIAN_POINT('Ctrl Pts',(-1.16262637999157,1.,-3.94761474780583));
#48357=CARTESIAN_POINT('Ctrl Pts',(-1.16767555244438,1.,-3.95351219509876));
#48358=CARTESIAN_POINT('Ctrl Pts',(-1.17275743590361,1.,-3.95939299213276));
#48359=CARTESIAN_POINT('Ctrl Pts',(-1.17787174135592,1.,-3.96525726358159));
#48360=CARTESIAN_POINT('Ctrl Pts',(-1.18301815039831,1.,-3.97110505165415));
#48361=CARTESIAN_POINT('Ctrl Pts',(-1.18819633715539,1.,-3.97693634767754));
#48362=CARTESIAN_POINT('Ctrl Pts',(-1.19340598349475,1.,-3.98275111052561));
#48363=CARTESIAN_POINT('Ctrl Pts',(-1.19864679609566,1.,-3.98854928957189));
#48364=CARTESIAN_POINT('Ctrl Pts',(-1.20391852375139,1.,-3.99433084799666));
#48365=CARTESIAN_POINT('Ctrl Pts',(-1.20922097029551,1.,-4.00009577950721));
#48366=CARTESIAN_POINT('Ctrl Pts',(-1.21455398918133,1.,-4.00584409522722));
#48367=CARTESIAN_POINT('Ctrl Pts',(-1.21884478244403,1.,-4.01042947140789));
#48368=CARTESIAN_POINT('Ctrl Pts',(-1.22207656455845,1.,-4.01386104433519));
#48369=CARTESIAN_POINT('Ctrl Pts',(-1.22423716681317,1.,-4.01614544569895));
#48370=CARTESIAN_POINT('Ctrl Pts',(-1.22531898815164,1.,-4.01728681790024));
#48371=CARTESIAN_POINT('Origin',(-1.22531898815164,0.,-4.01728681790024));
#48372=CARTESIAN_POINT('',(-1.36999806084572,1.,-3.97027773754922));
#48373=CARTESIAN_POINT('Origin',(0.,0.,0.));
#48374=CARTESIAN_POINT('',(-0.786422660833743,1.,-3.66661143271648));
#48375=CARTESIAN_POINT('Origin',(0.,1.,0.));
#48376=CARTESIAN_POINT('Ctrl Pts',(-0.786422660833742,1.,-3.66661143271648));
#48377=CARTESIAN_POINT('Ctrl Pts',(-0.786422660833742,0.666666666666667,
-3.66661143271648));
#48378=CARTESIAN_POINT('Ctrl Pts',(-0.786422660833742,0.333333333333333,
-3.66661143271648));
#48379=CARTESIAN_POINT('Ctrl Pts',(-0.786422660833742,-0.333333333333333,
-3.66661143271648));
#48380=CARTESIAN_POINT('Ctrl Pts',(-0.786422660833742,-0.666666666666667,
-3.66661143271648));
#48381=CARTESIAN_POINT('Ctrl Pts',(-0.786422660833742,-1.,-3.66661143271648));
#48382=CARTESIAN_POINT('Ctrl Pts',(-0.732042837400619,-1.,-4.13571194405636));
#48383=CARTESIAN_POINT('Ctrl Pts',(-0.732042837400619,1.,-4.13571194405636));
#48384=CARTESIAN_POINT('Ctrl Pts',(-0.732488575135926,-1.,-4.13420383737278));
#48385=CARTESIAN_POINT('Ctrl Pts',(-0.732488575135926,1.,-4.13420383737278));
#48386=CARTESIAN_POINT('Ctrl Pts',(-0.733376589325634,-1.,-4.13118752796397));
#48387=CARTESIAN_POINT('Ctrl Pts',(-0.733376589325634,1.,-4.13118752796397));
#48388=CARTESIAN_POINT('Ctrl Pts',(-0.734698226767512,-1.,-4.12666277572794));
#48389=CARTESIAN_POINT('Ctrl Pts',(-0.734698226767512,1.,-4.12666277572794));
#48390=CARTESIAN_POINT('Ctrl Pts',(-0.736439634335347,-1.,-4.12062919626082));
#48391=CARTESIAN_POINT('Ctrl Pts',(-0.736439634335347,1.,-4.12062919626082));
#48392=CARTESIAN_POINT('Ctrl Pts',(-0.738581708229119,-1.,-4.11308626953795));
#48393=CARTESIAN_POINT('Ctrl Pts',(-0.738581708229119,1.,-4.11308626953795));
#48394=CARTESIAN_POINT('Ctrl Pts',(-0.740688998555152,-1.,-4.1055424175856));
#48395=CARTESIAN_POINT('Ctrl Pts',(-0.740688998555152,1.,-4.1055424175856));
#48396=CARTESIAN_POINT('Ctrl Pts',(-0.742761369690018,-1.,-4.09799769702712));
#48397=CARTESIAN_POINT('Ctrl Pts',(-0.742761369690018,1.,-4.09799769702712));
#48398=CARTESIAN_POINT('Ctrl Pts',(-0.744798649705514,-1.,-4.09045220253011));
#48399=CARTESIAN_POINT('Ctrl Pts',(-0.744798649705514,1.,-4.09045220253011));
#48400=CARTESIAN_POINT('Ctrl Pts',(-0.746800631490822,-1.,-4.08290608094789));
#48401=CARTESIAN_POINT('Ctrl Pts',(-0.746800631490822,1.,-4.08290608094789));
#48402=CARTESIAN_POINT('Ctrl Pts',(-0.748767076679177,-1.,-4.07535951055363));
#48403=CARTESIAN_POINT('Ctrl Pts',(-0.748767076679177,1.,-4.07535951055363));
#48404=CARTESIAN_POINT('Ctrl Pts',(-0.750697720483176,-1.,-4.06781267241886));
#48405=CARTESIAN_POINT('Ctrl Pts',(-0.750697720483176,1.,-4.06781267241886));
#48406=CARTESIAN_POINT('Ctrl Pts',(-0.752592276482869,-1.,-4.06026572221399));
#48407=CARTESIAN_POINT('Ctrl Pts',(-0.752592276482869,1.,-4.06026572221399));
#48408=CARTESIAN_POINT('Ctrl Pts',(-0.754450441816412,-1.,-4.05271876688106));
#48409=CARTESIAN_POINT('Ctrl Pts',(-0.754450441816412,1.,-4.05271876688106));
#48410=CARTESIAN_POINT('Ctrl Pts',(-0.756271902370187,-1.,-4.04517182654344));
#48411=CARTESIAN_POINT('Ctrl Pts',(-0.756271902370187,1.,-4.04517182654344));
#48412=CARTESIAN_POINT('Ctrl Pts',(-0.758056338885554,-1.,-4.03762485803468));
#48413=CARTESIAN_POINT('Ctrl Pts',(-0.758056338885554,1.,-4.03762485803468));
#48414=CARTESIAN_POINT('Ctrl Pts',(-0.759803433244166,-1.,-4.0300778195465));
#48415=CARTESIAN_POINT('Ctrl Pts',(-0.759803433244166,1.,-4.0300778195465));
#48416=CARTESIAN_POINT('Ctrl Pts',(-0.761512875859942,-1.,-4.02253072741347));
#48417=CARTESIAN_POINT('Ctrl Pts',(-0.761512875859942,1.,-4.02253072741347));
#48418=CARTESIAN_POINT('Ctrl Pts',(-0.763184371182827,-1.,-4.01498370680434));
#48419=CARTESIAN_POINT('Ctrl Pts',(-0.763184371182827,1.,-4.01498370680434));
#48420=CARTESIAN_POINT('Ctrl Pts',(-0.764817648784946,-1.,-4.00743706791366));
#48421=CARTESIAN_POINT('Ctrl Pts',(-0.764817648784946,1.,-4.00743706791366));
#48422=CARTESIAN_POINT('Ctrl Pts',(-0.766412457135786,-1.,-3.99989129179464));
#48423=CARTESIAN_POINT('Ctrl Pts',(-0.766412457135786,1.,-3.99989129179464));
#48424=CARTESIAN_POINT('Ctrl Pts',(-0.767968531377708,-1.,-3.99234687880892));
#48425=CARTESIAN_POINT('Ctrl Pts',(-0.767968531377708,1.,-3.99234687880892));
#48426=CARTESIAN_POINT('Ctrl Pts',(-0.769485566245459,-1.,-3.98480422348403));
#48427=CARTESIAN_POINT('Ctrl Pts',(-0.769485566245459,1.,-3.98480422348403));
#48428=CARTESIAN_POINT('Ctrl Pts',(-0.770963190030504,-1.,-3.97726349165507));
#48429=CARTESIAN_POINT('Ctrl Pts',(-0.770963190030504,1.,-3.97726349165507));
#48430=CARTESIAN_POINT('Ctrl Pts',(-0.772400931772239,-1.,-3.96972446532832));
#48431=CARTESIAN_POINT('Ctrl Pts',(-0.772400931772239,1.,-3.96972446532832));
#48432=CARTESIAN_POINT('Ctrl Pts',(-0.773798212026683,-1.,-3.96218649639876));
#48433=CARTESIAN_POINT('Ctrl Pts',(-0.773798212026683,1.,-3.96218649639876));
#48434=CARTESIAN_POINT('Ctrl Pts',(-0.775154418039441,-1.,-3.95464885452364));
#48435=CARTESIAN_POINT('Ctrl Pts',(-0.775154418039441,1.,-3.95464885452364));
#48436=CARTESIAN_POINT('Ctrl Pts',(-0.77646896669796,-1.,-3.94711101619471));
#48437=CARTESIAN_POINT('Ctrl Pts',(-0.77646896669796,1.,-3.94711101619471));
#48438=CARTESIAN_POINT('Ctrl Pts',(-0.77774137056855,-1.,-3.93957296768098));
#48439=CARTESIAN_POINT('Ctrl Pts',(-0.77774137056855,1.,-3.93957296768098));
#48440=CARTESIAN_POINT('Ctrl Pts',(-0.778971308134786,-1.,-3.93203552473153));
#48441=CARTESIAN_POINT('Ctrl Pts',(-0.778971308134786,1.,-3.93203552473153));
#48442=CARTESIAN_POINT('Ctrl Pts',(-0.780158678615507,-1.,-3.92450058323799));
#48443=CARTESIAN_POINT('Ctrl Pts',(-0.780158678615507,1.,-3.92450058323799));
#48444=CARTESIAN_POINT('Ctrl Pts',(-0.781303428618344,-1.,-3.9169703605466));
#48445=CARTESIAN_POINT('Ctrl Pts',(-0.781303428618344,1.,-3.9169703605466));
#48446=CARTESIAN_POINT('Ctrl Pts',(-0.782405395622759,-1.,-3.90944671004536));
#48447=CARTESIAN_POINT('Ctrl Pts',(-0.782405395622759,1.,-3.90944671004536));
#48448=CARTESIAN_POINT('Ctrl Pts',(-0.783464141529082,-1.,-3.90193039043971));
#48449=CARTESIAN_POINT('Ctrl Pts',(-0.783464141529082,1.,-3.90193039043971));
#48450=CARTESIAN_POINT('Ctrl Pts',(-0.784478799358336,-1.,-3.89442039235105));
#48451=CARTESIAN_POINT('Ctrl Pts',(-0.784478799358336,1.,-3.89442039235105));
#48452=CARTESIAN_POINT('Ctrl Pts',(-0.785447890340723,-1.,-3.88691313167399));
#48453=CARTESIAN_POINT('Ctrl Pts',(-0.785447890340723,1.,-3.88691313167399));
#48454=CARTESIAN_POINT('Ctrl Pts',(-0.786369675812592,-1.,-3.87940402818186));
#48455=CARTESIAN_POINT('Ctrl Pts',(-0.786369675812592,1.,-3.87940402818186));
#48456=CARTESIAN_POINT('Ctrl Pts',(-0.78724252761798,-1.,-3.87188916600905));
#48457=CARTESIAN_POINT('Ctrl Pts',(-0.78724252761798,1.,-3.87188916600905));
#48458=CARTESIAN_POINT('Ctrl Pts',(-0.788065315093771,-1.,-3.86436702561342));
#48459=CARTESIAN_POINT('Ctrl Pts',(-0.788065315093771,1.,-3.86436702561342));
#48460=CARTESIAN_POINT('Ctrl Pts',(-0.788837734090688,-1.,-3.85683995872536));
#48461=CARTESIAN_POINT('Ctrl Pts',(-0.788837734090688,1.,-3.85683995872536));
#48462=CARTESIAN_POINT('Ctrl Pts',(-0.789560798155619,-1.,-3.8493163780891));
#48463=CARTESIAN_POINT('Ctrl Pts',(-0.789560798155619,1.,-3.8493163780891));
#48464=CARTESIAN_POINT('Ctrl Pts',(-0.790236124191289,-1.,-3.84180762342476));
#48465=CARTESIAN_POINT('Ctrl Pts',(-0.790236124191289,1.,-3.84180762342476));
#48466=CARTESIAN_POINT('Ctrl Pts',(-0.79086501270534,-1.,-3.83432392054804));
#48467=CARTESIAN_POINT('Ctrl Pts',(-0.79086501270534,1.,-3.83432392054804));
#48468=CARTESIAN_POINT('Ctrl Pts',(-0.791447528662381,-1.,-3.82687033899799));
#48469=CARTESIAN_POINT('Ctrl Pts',(-0.791447528662381,1.,-3.82687033899799));
#48470=CARTESIAN_POINT('Ctrl Pts',(-0.791981740718606,-1.,-3.81944345442237));
#48471=CARTESIAN_POINT('Ctrl Pts',(-0.791981740718606,1.,-3.81944345442237));
#48472=CARTESIAN_POINT('Ctrl Pts',(-0.792462483517568,-1.,-3.81202588694726));
#48473=CARTESIAN_POINT('Ctrl Pts',(-0.792462483517568,1.,-3.81202588694726));
#48474=CARTESIAN_POINT('Ctrl Pts',(-0.792882695234693,-1.,-3.80459229925598));
#48475=CARTESIAN_POINT('Ctrl Pts',(-0.792882695234693,1.,-3.80459229925598));
#48476=CARTESIAN_POINT('Ctrl Pts',(-0.7932356129732,-1.,-3.79711921389862));
#48477=CARTESIAN_POINT('Ctrl Pts',(-0.7932356129732,1.,-3.79711921389862));
#48478=CARTESIAN_POINT('Ctrl Pts',(-0.793516871680966,-1.,-3.78959439439222));
#48479=CARTESIAN_POINT('Ctrl Pts',(-0.793516871680966,1.,-3.78959439439222));
#48480=CARTESIAN_POINT('Ctrl Pts',(-0.793726235781339,-1.,-3.78202460377617));
#48481=CARTESIAN_POINT('Ctrl Pts',(-0.793726235781339,1.,-3.78202460377617));
#48482=CARTESIAN_POINT('Ctrl Pts',(-0.793870523787515,-1.,-3.77444863801264));
#48483=CARTESIAN_POINT('Ctrl Pts',(-0.793870523787515,1.,-3.77444863801264));
#48484=CARTESIAN_POINT('Ctrl Pts',(-0.793961083689141,-1.,-3.76692626931184));
#48485=CARTESIAN_POINT('Ctrl Pts',(-0.793961083689141,1.,-3.76692626931184));
#48486=CARTESIAN_POINT('Ctrl Pts',(-0.794008429135047,-1.,-3.75951468666325));
#48487=CARTESIAN_POINT('Ctrl Pts',(-0.794008429135047,1.,-3.75951468666325));
#48488=CARTESIAN_POINT('Ctrl Pts',(-0.794017347371441,-1.,-3.75224692493895));
#48489=CARTESIAN_POINT('Ctrl Pts',(-0.794017347371441,1.,-3.75224692493895));
#48490=CARTESIAN_POINT('Ctrl Pts',(-0.79398270045988,-1.,-3.74511357728827));
#48491=CARTESIAN_POINT('Ctrl Pts',(-0.79398270045988,1.,-3.74511357728827));
#48492=CARTESIAN_POINT('Ctrl Pts',(-0.79388270093679,-1.,-3.73803280541576));
#48493=CARTESIAN_POINT('Ctrl Pts',(-0.79388270093679,1.,-3.73803280541576));
#48494=CARTESIAN_POINT('Ctrl Pts',(-0.793682750269347,-1.,-3.7308691469564));
#48495=CARTESIAN_POINT('Ctrl Pts',(-0.793682750269347,1.,-3.7308691469564));
#48496=CARTESIAN_POINT('Ctrl Pts',(-0.79334702378387,-1.,-3.7234879729357));
#48497=CARTESIAN_POINT('Ctrl Pts',(-0.79334702378387,1.,-3.7234879729357));
#48498=CARTESIAN_POINT('Ctrl Pts',(-0.792848377370115,-1.,-3.7158024239604));
#48499=CARTESIAN_POINT('Ctrl Pts',(-0.792848377370115,1.,-3.7158024239604));
#48500=CARTESIAN_POINT('Ctrl Pts',(-0.792177688845968,-1.,-3.70781724021879));
#48501=CARTESIAN_POINT('Ctrl Pts',(-0.792177688845968,1.,-3.70781724021879));
#48502=CARTESIAN_POINT('Ctrl Pts',(-0.791356575696509,-1.,-3.69968940808982));
#48503=CARTESIAN_POINT('Ctrl Pts',(-0.791356575696509,1.,-3.69968940808982));
#48504=CARTESIAN_POINT('Ctrl Pts',(-0.79043628498958,-1.,-3.69172044327754));
#48505=CARTESIAN_POINT('Ctrl Pts',(-0.79043628498958,1.,-3.69172044327754));
#48506=CARTESIAN_POINT('Ctrl Pts',(-0.789483546065158,-1.,-3.68428439784285));
#48507=CARTESIAN_POINT('Ctrl Pts',(-0.789483546065158,1.,-3.68428439784285));
#48508=CARTESIAN_POINT('Ctrl Pts',(-0.788569566220662,-1.,-3.67777119516438));
#48509=CARTESIAN_POINT('Ctrl Pts',(-0.788569566220662,1.,-3.67777119516438));
#48510=CARTESIAN_POINT('Ctrl Pts',(-0.787758799995426,-1.,-3.672529236635));
#48511=CARTESIAN_POINT('Ctrl Pts',(-0.787758799995426,1.,-3.672529236635));
#48512=CARTESIAN_POINT('Ctrl Pts',(-0.787095252589508,-1.,-3.66879484800625));
#48513=CARTESIAN_POINT('Ctrl Pts',(-0.787095252589508,1.,-3.66879484800625));
#48514=CARTESIAN_POINT('Ctrl Pts',(-0.786698783541658,-1.,-3.66710211819938));
#48515=CARTESIAN_POINT('Ctrl Pts',(-0.786698783541658,1.,-3.66710211819938));
#48516=CARTESIAN_POINT('Ctrl Pts',(-0.786480236184947,-1.,-3.66657784454965));
#48517=CARTESIAN_POINT('Ctrl Pts',(-0.786480236184947,1.,-3.66657784454965));
#48518=CARTESIAN_POINT('Ctrl Pts',(-0.786369528183039,-1.,-3.66655932661846));
#48519=CARTESIAN_POINT('Ctrl Pts',(-0.786369528183039,1.,-3.66655932661846));
#48520=CARTESIAN_POINT('Ctrl Pts',(-0.786322922920599,-1.,-3.66663282329846));
#48521=CARTESIAN_POINT('Ctrl Pts',(-0.786322922920599,1.,-3.66663282329846));
#48522=CARTESIAN_POINT('',(-0.732042837400619,1.,-4.13571194405636));
#48523=CARTESIAN_POINT('Ctrl Pts',(-0.732042837400619,1.,-4.13571194405636));
#48524=CARTESIAN_POINT('Ctrl Pts',(-0.732488575135926,1.,-4.13420383737278));
#48525=CARTESIAN_POINT('Ctrl Pts',(-0.733376589325634,1.,-4.13118752796397));
#48526=CARTESIAN_POINT('Ctrl Pts',(-0.734698226767512,1.,-4.12666277572794));
#48527=CARTESIAN_POINT('Ctrl Pts',(-0.736439634335347,1.,-4.12062919626082));
#48528=CARTESIAN_POINT('Ctrl Pts',(-0.738581708229119,1.,-4.11308626953795));
#48529=CARTESIAN_POINT('Ctrl Pts',(-0.740688998555152,1.,-4.1055424175856));
#48530=CARTESIAN_POINT('Ctrl Pts',(-0.742761369690018,1.,-4.09799769702712));
#48531=CARTESIAN_POINT('Ctrl Pts',(-0.744798649705514,1.,-4.09045220253011));
#48532=CARTESIAN_POINT('Ctrl Pts',(-0.746800631490822,1.,-4.08290608094789));
#48533=CARTESIAN_POINT('Ctrl Pts',(-0.748767076679177,1.,-4.07535951055363));
#48534=CARTESIAN_POINT('Ctrl Pts',(-0.750697720483176,1.,-4.06781267241886));
#48535=CARTESIAN_POINT('Ctrl Pts',(-0.752592276482869,1.,-4.06026572221399));
#48536=CARTESIAN_POINT('Ctrl Pts',(-0.754450441816412,1.,-4.05271876688106));
#48537=CARTESIAN_POINT('Ctrl Pts',(-0.756271902370187,1.,-4.04517182654344));
#48538=CARTESIAN_POINT('Ctrl Pts',(-0.758056338885554,1.,-4.03762485803468));
#48539=CARTESIAN_POINT('Ctrl Pts',(-0.759803433244166,1.,-4.0300778195465));
#48540=CARTESIAN_POINT('Ctrl Pts',(-0.761512875859942,1.,-4.02253072741347));
#48541=CARTESIAN_POINT('Ctrl Pts',(-0.763184371182827,1.,-4.01498370680434));
#48542=CARTESIAN_POINT('Ctrl Pts',(-0.764817648784946,1.,-4.00743706791366));
#48543=CARTESIAN_POINT('Ctrl Pts',(-0.766412457135786,1.,-3.99989129179464));
#48544=CARTESIAN_POINT('Ctrl Pts',(-0.767968531377708,1.,-3.99234687880892));
#48545=CARTESIAN_POINT('Ctrl Pts',(-0.769485566245459,1.,-3.98480422348403));
#48546=CARTESIAN_POINT('Ctrl Pts',(-0.770963190030504,1.,-3.97726349165507));
#48547=CARTESIAN_POINT('Ctrl Pts',(-0.772400931772239,1.,-3.96972446532832));
#48548=CARTESIAN_POINT('Ctrl Pts',(-0.773798212026683,1.,-3.96218649639876));
#48549=CARTESIAN_POINT('Ctrl Pts',(-0.775154418039441,1.,-3.95464885452364));
#48550=CARTESIAN_POINT('Ctrl Pts',(-0.77646896669796,1.,-3.94711101619471));
#48551=CARTESIAN_POINT('Ctrl Pts',(-0.77774137056855,1.,-3.93957296768098));
#48552=CARTESIAN_POINT('Ctrl Pts',(-0.778971308134786,1.,-3.93203552473153));
#48553=CARTESIAN_POINT('Ctrl Pts',(-0.780158678615507,1.,-3.92450058323799));
#48554=CARTESIAN_POINT('Ctrl Pts',(-0.781303428618344,1.,-3.9169703605466));
#48555=CARTESIAN_POINT('Ctrl Pts',(-0.782405395622759,1.,-3.90944671004536));
#48556=CARTESIAN_POINT('Ctrl Pts',(-0.783464141529082,1.,-3.90193039043971));
#48557=CARTESIAN_POINT('Ctrl Pts',(-0.784478799358336,1.,-3.89442039235105));
#48558=CARTESIAN_POINT('Ctrl Pts',(-0.785447890340723,1.,-3.88691313167399));
#48559=CARTESIAN_POINT('Ctrl Pts',(-0.786369675812592,1.,-3.87940402818186));
#48560=CARTESIAN_POINT('Ctrl Pts',(-0.78724252761798,1.,-3.87188916600905));
#48561=CARTESIAN_POINT('Ctrl Pts',(-0.788065315093771,1.,-3.86436702561342));
#48562=CARTESIAN_POINT('Ctrl Pts',(-0.788837734090688,1.,-3.85683995872536));
#48563=CARTESIAN_POINT('Ctrl Pts',(-0.789560798155619,1.,-3.8493163780891));
#48564=CARTESIAN_POINT('Ctrl Pts',(-0.790236124191289,1.,-3.84180762342476));
#48565=CARTESIAN_POINT('Ctrl Pts',(-0.79086501270534,1.,-3.83432392054804));
#48566=CARTESIAN_POINT('Ctrl Pts',(-0.791447528662381,1.,-3.82687033899799));
#48567=CARTESIAN_POINT('Ctrl Pts',(-0.791981740718606,1.,-3.81944345442237));
#48568=CARTESIAN_POINT('Ctrl Pts',(-0.792462483517568,1.,-3.81202588694726));
#48569=CARTESIAN_POINT('Ctrl Pts',(-0.792882695234693,1.,-3.80459229925598));
#48570=CARTESIAN_POINT('Ctrl Pts',(-0.7932356129732,1.,-3.79711921389862));
#48571=CARTESIAN_POINT('Ctrl Pts',(-0.793516871680966,1.,-3.78959439439222));
#48572=CARTESIAN_POINT('Ctrl Pts',(-0.793726235781339,1.,-3.78202460377617));
#48573=CARTESIAN_POINT('Ctrl Pts',(-0.793870523787515,1.,-3.77444863801264));
#48574=CARTESIAN_POINT('Ctrl Pts',(-0.793961083689141,1.,-3.76692626931184));
#48575=CARTESIAN_POINT('Ctrl Pts',(-0.794008429135047,1.,-3.75951468666325));
#48576=CARTESIAN_POINT('Ctrl Pts',(-0.794017347371441,1.,-3.75224692493895));
#48577=CARTESIAN_POINT('Ctrl Pts',(-0.79398270045988,1.,-3.74511357728827));
#48578=CARTESIAN_POINT('Ctrl Pts',(-0.79388270093679,1.,-3.73803280541576));
#48579=CARTESIAN_POINT('Ctrl Pts',(-0.793682750269347,1.,-3.7308691469564));
#48580=CARTESIAN_POINT('Ctrl Pts',(-0.79334702378387,1.,-3.7234879729357));
#48581=CARTESIAN_POINT('Ctrl Pts',(-0.792848377370115,1.,-3.7158024239604));
#48582=CARTESIAN_POINT('Ctrl Pts',(-0.792177688845968,1.,-3.70781724021879));
#48583=CARTESIAN_POINT('Ctrl Pts',(-0.791356575696509,1.,-3.69968940808982));
#48584=CARTESIAN_POINT('Ctrl Pts',(-0.79043628498958,1.,-3.69172044327754));
#48585=CARTESIAN_POINT('Ctrl Pts',(-0.789483546065158,1.,-3.68428439784285));
#48586=CARTESIAN_POINT('Ctrl Pts',(-0.788569566220662,1.,-3.67777119516438));
#48587=CARTESIAN_POINT('Ctrl Pts',(-0.787758799995426,1.,-3.672529236635));
#48588=CARTESIAN_POINT('Ctrl Pts',(-0.787145041181589,1.,-3.66907505398769));
#48589=CARTESIAN_POINT('Ctrl Pts',(-0.7867743371985,1.,-3.66743103898844));
#48590=CARTESIAN_POINT('Ctrl Pts',(-0.78656591955989,1.,-3.66680946938396));
#48591=CARTESIAN_POINT('Ctrl Pts',(-0.786459983896781,1.,-3.66664310415236));
#48592=CARTESIAN_POINT('Ctrl Pts',(-0.786422660833743,1.,-3.66661143271648));
#48593=CARTESIAN_POINT('',(-0.732042837400619,0.,-4.13571194405636));
#48594=CARTESIAN_POINT('Ctrl Pts',(-0.385214314776329,-1.,-3.73016218570874));
#48595=CARTESIAN_POINT('Ctrl Pts',(-0.385214314776329,1.,-3.73016218570874));
#48596=CARTESIAN_POINT('Ctrl Pts',(-0.385147278814804,-1.,-3.73010668803185));
#48597=CARTESIAN_POINT('Ctrl Pts',(-0.385147278814804,1.,-3.73010668803185));
#48598=CARTESIAN_POINT('Ctrl Pts',(-0.385047711603887,-1.,-3.73015851028729));
#48599=CARTESIAN_POINT('Ctrl Pts',(-0.385047711603887,1.,-3.73015851028729));
#48600=CARTESIAN_POINT('Ctrl Pts',(-0.385001870183841,-1.,-3.73072465900727));
#48601=CARTESIAN_POINT('Ctrl Pts',(-0.385001870183841,1.,-3.73072465900727));
#48602=CARTESIAN_POINT('Ctrl Pts',(-0.385147887989515,-1.,-3.73245705639337));
#48603=CARTESIAN_POINT('Ctrl Pts',(-0.385147887989515,1.,-3.73245705639337));
#48604=CARTESIAN_POINT('Ctrl Pts',(-0.385670806454744,-1.,-3.73621371845475));
#48605=CARTESIAN_POINT('Ctrl Pts',(-0.385670806454744,1.,-3.73621371845475));
#48606=CARTESIAN_POINT('Ctrl Pts',(-0.386519576222035,-1.,-3.74144965781088));
#48607=CARTESIAN_POINT('Ctrl Pts',(-0.386519576222035,1.,-3.74144965781088));
#48608=CARTESIAN_POINT('Ctrl Pts',(-0.387663020050396,-1.,-3.74792651696269));
#48609=CARTESIAN_POINT('Ctrl Pts',(-0.387663020050396,1.,-3.74792651696269));
#48610=CARTESIAN_POINT('Ctrl Pts',(-0.389054775898251,-1.,-3.75529302894757));
#48611=CARTESIAN_POINT('Ctrl Pts',(-0.389054775898251,1.,-3.75529302894757));
#48612=CARTESIAN_POINT('Ctrl Pts',(-0.390642072979259,-1.,-3.76315635032993));
#48613=CARTESIAN_POINT('Ctrl Pts',(-0.390642072979259,1.,-3.76315635032993));
#48614=CARTESIAN_POINT('Ctrl Pts',(-0.392372786223347,-1.,-3.77114011595892));
#48615=CARTESIAN_POINT('Ctrl Pts',(-0.392372786223347,1.,-3.77114011595892));
#48616=CARTESIAN_POINT('Ctrl Pts',(-0.394202481011595,-1.,-3.77894173114368));
#48617=CARTESIAN_POINT('Ctrl Pts',(-0.394202481011595,1.,-3.77894173114368));
#48618=CARTESIAN_POINT('Ctrl Pts',(-0.396103205335029,-1.,-3.78640521279479));
#48619=CARTESIAN_POINT('Ctrl Pts',(-0.396103205335029,1.,-3.78640521279479));
#48620=CARTESIAN_POINT('Ctrl Pts',(-0.398064818684158,-1.,-3.79352887163457));
#48621=CARTESIAN_POINT('Ctrl Pts',(-0.398064818684158,1.,-3.79352887163457));
#48622=CARTESIAN_POINT('Ctrl Pts',(-0.400088346504727,-1.,-3.80040370384659));
#48623=CARTESIAN_POINT('Ctrl Pts',(-0.400088346504727,1.,-3.80040370384659));
#48624=CARTESIAN_POINT('Ctrl Pts',(-0.402181320148475,-1.,-3.80716881962763));
#48625=CARTESIAN_POINT('Ctrl Pts',(-0.402181320148475,1.,-3.80716881962763));
#48626=CARTESIAN_POINT('Ctrl Pts',(-0.404352694628236,-1.,-3.81396374287762));
#48627=CARTESIAN_POINT('Ctrl Pts',(-0.404352694628236,1.,-3.81396374287762));
#48628=CARTESIAN_POINT('Ctrl Pts',(-0.406607038258906,-1.,-3.82087303913741));
#48629=CARTESIAN_POINT('Ctrl Pts',(-0.406607038258906,1.,-3.82087303913741));
#48630=CARTESIAN_POINT('Ctrl Pts',(-0.408942371447377,-1.,-3.82790724256397));
#48631=CARTESIAN_POINT('Ctrl Pts',(-0.408942371447377,1.,-3.82790724256397));
#48632=CARTESIAN_POINT('Ctrl Pts',(-0.41135303879846,-1.,-3.83503345578645));
#48633=CARTESIAN_POINT('Ctrl Pts',(-0.41135303879846,1.,-3.83503345578645));
#48634=CARTESIAN_POINT('Ctrl Pts',(-0.413831367016727,-1.,-3.84219403994742));
#48635=CARTESIAN_POINT('Ctrl Pts',(-0.413831367016727,1.,-3.84219403994742));
#48636=CARTESIAN_POINT('Ctrl Pts',(-0.41636967805292,-1.,-3.8493286415751));
#48637=CARTESIAN_POINT('Ctrl Pts',(-0.41636967805292,1.,-3.8493286415751));
#48638=CARTESIAN_POINT('Ctrl Pts',(-0.41896246808681,-1.,-3.85639825648031));
#48639=CARTESIAN_POINT('Ctrl Pts',(-0.41896246808681,1.,-3.85639825648031));
#48640=CARTESIAN_POINT('Ctrl Pts',(-0.421607423177576,-1.,-3.86339652542749));
#48641=CARTESIAN_POINT('Ctrl Pts',(-0.421607423177576,1.,-3.86339652542749));
#48642=CARTESIAN_POINT('Ctrl Pts',(-0.424304173195142,-1.,-3.87033643487882));
#48643=CARTESIAN_POINT('Ctrl Pts',(-0.424304173195142,1.,-3.87033643487882));
#48644=CARTESIAN_POINT('Ctrl Pts',(-0.427053541173469,-1.,-3.87724240306609));
#48645=CARTESIAN_POINT('Ctrl Pts',(-0.427053541173469,1.,-3.87724240306609));
#48646=CARTESIAN_POINT('Ctrl Pts',(-0.429856640579734,-1.,-3.88414070943334));
#48647=CARTESIAN_POINT('Ctrl Pts',(-0.429856640579734,1.,-3.88414070943334));
#48648=CARTESIAN_POINT('Ctrl Pts',(-0.432713929544439,-1.,-3.89104947940592));
#48649=CARTESIAN_POINT('Ctrl Pts',(-0.432713929544439,1.,-3.89104947940592));
#48650=CARTESIAN_POINT('Ctrl Pts',(-0.435624629433506,-1.,-3.8979725665544));
#48651=CARTESIAN_POINT('Ctrl Pts',(-0.435624629433506,1.,-3.8979725665544));
#48652=CARTESIAN_POINT('Ctrl Pts',(-0.438587235458233,-1.,-3.90490512938546));
#48653=CARTESIAN_POINT('Ctrl Pts',(-0.438587235458233,1.,-3.90490512938546));
#48654=CARTESIAN_POINT('Ctrl Pts',(-0.441599824524047,-1.,-3.91183704069146));
#48655=CARTESIAN_POINT('Ctrl Pts',(-0.441599824524047,1.,-3.91183704069146));
#48656=CARTESIAN_POINT('Ctrl Pts',(-0.444660430230593,-1.,-3.91875701610721));
#48657=CARTESIAN_POINT('Ctrl Pts',(-0.444660430230593,1.,-3.91875701610721));
#48658=CARTESIAN_POINT('Ctrl Pts',(-0.447767416837297,-1.,-3.92565674143424));
#48659=CARTESIAN_POINT('Ctrl Pts',(-0.447767416837297,1.,-3.92565674143424));
#48660=CARTESIAN_POINT('Ctrl Pts',(-0.450919768356347,-1.,-3.93253407403128));
#48661=CARTESIAN_POINT('Ctrl Pts',(-0.450919768356347,1.,-3.93253407403128));
#48662=CARTESIAN_POINT('Ctrl Pts',(-0.454116879027576,-1.,-3.93939080846298));
#48663=CARTESIAN_POINT('Ctrl Pts',(-0.454116879027576,1.,-3.93939080846298));
#48664=CARTESIAN_POINT('Ctrl Pts',(-0.457358410451674,-1.,-3.94623117206675));
#48665=CARTESIAN_POINT('Ctrl Pts',(-0.457358410451674,1.,-3.94623117206675));
#48666=CARTESIAN_POINT('Ctrl Pts',(-0.460644124429119,-1.,-3.95306005817363));
#48667=CARTESIAN_POINT('Ctrl Pts',(-0.460644124429119,1.,-3.95306005817363));
#48668=CARTESIAN_POINT('Ctrl Pts',(-0.463973722115744,-1.,-3.95988133243543));
#48669=CARTESIAN_POINT('Ctrl Pts',(-0.463973722115744,1.,-3.95988133243543));
#48670=CARTESIAN_POINT('Ctrl Pts',(-0.467346690880672,-1.,-3.96669622273946));
#48671=CARTESIAN_POINT('Ctrl Pts',(-0.467346690880672,1.,-3.96669622273946));
#48672=CARTESIAN_POINT('Ctrl Pts',(-0.470762379613477,-1.,-3.97350414289415));
#48673=CARTESIAN_POINT('Ctrl Pts',(-0.470762379613477,1.,-3.97350414289415));
#48674=CARTESIAN_POINT('Ctrl Pts',(-0.474220061019542,-1.,-3.9803033804443));
#48675=CARTESIAN_POINT('Ctrl Pts',(-0.474220061019542,1.,-3.9803033804443));
#48676=CARTESIAN_POINT('Ctrl Pts',(-0.477718999122033,-1.,-3.98709184306743));
#48677=CARTESIAN_POINT('Ctrl Pts',(-0.477718999122033,1.,-3.98709184306743));
#48678=CARTESIAN_POINT('Ctrl Pts',(-0.481258512209638,-1.,-3.99386775880655));
#48679=CARTESIAN_POINT('Ctrl Pts',(-0.481258512209638,1.,-3.99386775880655));
#48680=CARTESIAN_POINT('Ctrl Pts',(-0.484838042421754,-1.,-4.00063045119234));
#48681=CARTESIAN_POINT('Ctrl Pts',(-0.484838042421754,1.,-4.00063045119234));
#48682=CARTESIAN_POINT('Ctrl Pts',(-0.488457130424531,-1.,-4.0073800839092));
#48683=CARTESIAN_POINT('Ctrl Pts',(-0.488457130424531,1.,-4.0073800839092));
#48684=CARTESIAN_POINT('Ctrl Pts',(-0.492115383417931,-1.,-4.01411733503486));
#48685=CARTESIAN_POINT('Ctrl Pts',(-0.492115383417931,1.,-4.01411733503486));
#48686=CARTESIAN_POINT('Ctrl Pts',(-0.495812444326223,-1.,-4.02084308851813));
#48687=CARTESIAN_POINT('Ctrl Pts',(-0.495812444326223,1.,-4.02084308851813));
#48688=CARTESIAN_POINT('Ctrl Pts',(-0.49954796234089,-1.,-4.0275581398015));
#48689=CARTESIAN_POINT('Ctrl Pts',(-0.49954796234089,1.,-4.0275581398015));
#48690=CARTESIAN_POINT('Ctrl Pts',(-0.503321556915514,-1.,-4.0342628417439));
#48691=CARTESIAN_POINT('Ctrl Pts',(-0.503321556915514,1.,-4.0342628417439));
#48692=CARTESIAN_POINT('Ctrl Pts',(-0.507132823288362,-1.,-4.04095715149074));
#48693=CARTESIAN_POINT('Ctrl Pts',(-0.507132823288362,1.,-4.04095715149074));
#48694=CARTESIAN_POINT('Ctrl Pts',(-0.510981349219174,-1.,-4.04764078815591));
#48695=CARTESIAN_POINT('Ctrl Pts',(-0.510981349219174,1.,-4.04764078815591));
#48696=CARTESIAN_POINT('Ctrl Pts',(-0.514866728193104,-1.,-4.05431335771261));
#48697=CARTESIAN_POINT('Ctrl Pts',(-0.514866728193104,1.,-4.05431335771261));
#48698=CARTESIAN_POINT('Ctrl Pts',(-0.51878857233681,-1.,-4.06097448037934));
#48699=CARTESIAN_POINT('Ctrl Pts',(-0.51878857233681,1.,-4.06097448037934));
#48700=CARTESIAN_POINT('Ctrl Pts',(-0.522746528602768,-1.,-4.06762394471075));
#48701=CARTESIAN_POINT('Ctrl Pts',(-0.522746528602768,1.,-4.06762394471075));
#48702=CARTESIAN_POINT('Ctrl Pts',(-0.526740277227,-1.,-4.07426172299496));
#48703=CARTESIAN_POINT('Ctrl Pts',(-0.526740277227,1.,-4.07426172299496));
#48704=CARTESIAN_POINT('Ctrl Pts',(-0.530769518728075,-1.,-4.08088789536488));
#48705=CARTESIAN_POINT('Ctrl Pts',(-0.530769518728075,1.,-4.08088789536488));
#48706=CARTESIAN_POINT('Ctrl Pts',(-0.534833963476999,-1.,-4.08750259988693));
#48707=CARTESIAN_POINT('Ctrl Pts',(-0.534833963476999,1.,-4.08750259988693));
#48708=CARTESIAN_POINT('Ctrl Pts',(-0.538933321179921,-1.,-4.09410597627116));
#48709=CARTESIAN_POINT('Ctrl Pts',(-0.538933321179921,1.,-4.09410597627116));
#48710=CARTESIAN_POINT('Ctrl Pts',(-0.543067286878457,-1.,-4.10069810244473));
#48711=CARTESIAN_POINT('Ctrl Pts',(-0.543067286878457,1.,-4.10069810244473));
#48712=CARTESIAN_POINT('Ctrl Pts',(-0.54723553948676,-1.,-4.1072789702877));
#48713=CARTESIAN_POINT('Ctrl Pts',(-0.54723553948676,1.,-4.1072789702877));
#48714=CARTESIAN_POINT('Ctrl Pts',(-0.551437758498247,-1.,-4.11384852025578));
#48715=CARTESIAN_POINT('Ctrl Pts',(-0.551437758498247,1.,-4.11384852025578));
#48716=CARTESIAN_POINT('Ctrl Pts',(-0.555673636130778,-1.,-4.1204066619623));
#48717=CARTESIAN_POINT('Ctrl Pts',(-0.555673636130778,1.,-4.1204066619623));
#48718=CARTESIAN_POINT('Ctrl Pts',(-0.559942890594628,-1.,-4.12695329951859));
#48719=CARTESIAN_POINT('Ctrl Pts',(-0.559942890594628,1.,-4.12695329951859));
#48720=CARTESIAN_POINT('Ctrl Pts',(-0.564245279535705,-1.,-4.13348835726086));
#48721=CARTESIAN_POINT('Ctrl Pts',(-0.564245279535705,1.,-4.13348835726086));
#48722=CARTESIAN_POINT('Ctrl Pts',(-0.568580610187116,-1.,-4.14001179828669));
#48723=CARTESIAN_POINT('Ctrl Pts',(-0.568580610187116,1.,-4.14001179828669));
#48724=CARTESIAN_POINT('Ctrl Pts',(-0.572948736066277,-1.,-4.14652361065787));
#48725=CARTESIAN_POINT('Ctrl Pts',(-0.572948736066277,1.,-4.14652361065787));
#48726=CARTESIAN_POINT('Ctrl Pts',(-0.576469391673917,-1.,-4.1517237611974));
#48727=CARTESIAN_POINT('Ctrl Pts',(-0.576469391673917,1.,-4.1517237611974));
#48728=CARTESIAN_POINT('Ctrl Pts',(-0.579124568912543,-1.,-4.15561864787379));
#48729=CARTESIAN_POINT('Ctrl Pts',(-0.579124568912543,1.,-4.15561864787379));
#48730=CARTESIAN_POINT('Ctrl Pts',(-0.580901211462913,-1.,-4.15821291712391));
#48731=CARTESIAN_POINT('Ctrl Pts',(-0.580901211462913,1.,-4.15821291712391));
#48732=CARTESIAN_POINT('Ctrl Pts',(-0.581791163835814,-1.,-4.15950947128175));
#48733=CARTESIAN_POINT('Ctrl Pts',(-0.581791163835814,1.,-4.15950947128175));
#48734=CARTESIAN_POINT('',(-0.385112848332548,1.,-3.73017266276632));
#48735=CARTESIAN_POINT('Ctrl Pts',(-0.385112848332549,-1.,-3.73017266276632));
#48736=CARTESIAN_POINT('Ctrl Pts',(-0.385112848332549,-0.666666666666667,
-3.73017266276632));
#48737=CARTESIAN_POINT('Ctrl Pts',(-0.385112848332549,-0.333333333333333,
-3.73017266276632));
#48738=CARTESIAN_POINT('Ctrl Pts',(-0.385112848332549,0.333333333333333,
-3.73017266276632));
#48739=CARTESIAN_POINT('Ctrl Pts',(-0.385112848332549,0.666666666666667,
-3.73017266276632));
#48740=CARTESIAN_POINT('Ctrl Pts',(-0.385112848332549,1.,-3.73017266276632));
#48741=CARTESIAN_POINT('',(-0.581791163835814,1.,-4.15950947128175));
#48742=CARTESIAN_POINT('',(-0.581791163835814,0.,-4.15950947128175));
#48743=CARTESIAN_POINT('Ctrl Pts',(-0.385112848332549,1.,-3.73017266276632));
#48744=CARTESIAN_POINT('Ctrl Pts',(-0.385087139001609,1.,-3.73021431755218));
#48745=CARTESIAN_POINT('Ctrl Pts',(-0.385037797882046,1.,-3.73040527620929));
#48746=CARTESIAN_POINT('Ctrl Pts',(-0.385031656499142,1.,-3.731060828624));
#48747=CARTESIAN_POINT('Ctrl Pts',(-0.385187124633965,1.,-3.73273893363318));
#48748=CARTESIAN_POINT('Ctrl Pts',(-0.385670806454744,1.,-3.73621371845475));
#48749=CARTESIAN_POINT('Ctrl Pts',(-0.386519576222035,1.,-3.74144965781088));
#48750=CARTESIAN_POINT('Ctrl Pts',(-0.387663020050396,1.,-3.74792651696269));
#48751=CARTESIAN_POINT('Ctrl Pts',(-0.389054775898251,1.,-3.75529302894757));
#48752=CARTESIAN_POINT('Ctrl Pts',(-0.390642072979259,1.,-3.76315635032993));
#48753=CARTESIAN_POINT('Ctrl Pts',(-0.392372786223347,1.,-3.77114011595892));
#48754=CARTESIAN_POINT('Ctrl Pts',(-0.394202481011595,1.,-3.77894173114368));
#48755=CARTESIAN_POINT('Ctrl Pts',(-0.396103205335029,1.,-3.78640521279479));
#48756=CARTESIAN_POINT('Ctrl Pts',(-0.398064818684158,1.,-3.79352887163457));
#48757=CARTESIAN_POINT('Ctrl Pts',(-0.400088346504727,1.,-3.80040370384659));
#48758=CARTESIAN_POINT('Ctrl Pts',(-0.402181320148475,1.,-3.80716881962763));
#48759=CARTESIAN_POINT('Ctrl Pts',(-0.404352694628236,1.,-3.81396374287762));
#48760=CARTESIAN_POINT('Ctrl Pts',(-0.406607038258906,1.,-3.82087303913741));
#48761=CARTESIAN_POINT('Ctrl Pts',(-0.408942371447377,1.,-3.82790724256397));
#48762=CARTESIAN_POINT('Ctrl Pts',(-0.41135303879846,1.,-3.83503345578645));
#48763=CARTESIAN_POINT('Ctrl Pts',(-0.413831367016727,1.,-3.84219403994742));
#48764=CARTESIAN_POINT('Ctrl Pts',(-0.41636967805292,1.,-3.8493286415751));
#48765=CARTESIAN_POINT('Ctrl Pts',(-0.41896246808681,1.,-3.85639825648031));
#48766=CARTESIAN_POINT('Ctrl Pts',(-0.421607423177576,1.,-3.86339652542749));
#48767=CARTESIAN_POINT('Ctrl Pts',(-0.424304173195142,1.,-3.87033643487882));
#48768=CARTESIAN_POINT('Ctrl Pts',(-0.427053541173469,1.,-3.87724240306609));
#48769=CARTESIAN_POINT('Ctrl Pts',(-0.429856640579734,1.,-3.88414070943334));
#48770=CARTESIAN_POINT('Ctrl Pts',(-0.432713929544439,1.,-3.89104947940592));
#48771=CARTESIAN_POINT('Ctrl Pts',(-0.435624629433506,1.,-3.8979725665544));
#48772=CARTESIAN_POINT('Ctrl Pts',(-0.438587235458233,1.,-3.90490512938546));
#48773=CARTESIAN_POINT('Ctrl Pts',(-0.441599824524047,1.,-3.91183704069146));
#48774=CARTESIAN_POINT('Ctrl Pts',(-0.444660430230593,1.,-3.91875701610721));
#48775=CARTESIAN_POINT('Ctrl Pts',(-0.447767416837297,1.,-3.92565674143424));
#48776=CARTESIAN_POINT('Ctrl Pts',(-0.450919768356347,1.,-3.93253407403128));
#48777=CARTESIAN_POINT('Ctrl Pts',(-0.454116879027576,1.,-3.93939080846298));
#48778=CARTESIAN_POINT('Ctrl Pts',(-0.457358410451674,1.,-3.94623117206675));
#48779=CARTESIAN_POINT('Ctrl Pts',(-0.460644124429119,1.,-3.95306005817363));
#48780=CARTESIAN_POINT('Ctrl Pts',(-0.463973722115744,1.,-3.95988133243543));
#48781=CARTESIAN_POINT('Ctrl Pts',(-0.467346690880672,1.,-3.96669622273946));
#48782=CARTESIAN_POINT('Ctrl Pts',(-0.470762379613477,1.,-3.97350414289415));
#48783=CARTESIAN_POINT('Ctrl Pts',(-0.474220061019542,1.,-3.9803033804443));
#48784=CARTESIAN_POINT('Ctrl Pts',(-0.477718999122033,1.,-3.98709184306743));
#48785=CARTESIAN_POINT('Ctrl Pts',(-0.481258512209638,1.,-3.99386775880655));
#48786=CARTESIAN_POINT('Ctrl Pts',(-0.484838042421754,1.,-4.00063045119234));
#48787=CARTESIAN_POINT('Ctrl Pts',(-0.488457130424531,1.,-4.0073800839092));
#48788=CARTESIAN_POINT('Ctrl Pts',(-0.492115383417931,1.,-4.01411733503486));
#48789=CARTESIAN_POINT('Ctrl Pts',(-0.495812444326223,1.,-4.02084308851813));
#48790=CARTESIAN_POINT('Ctrl Pts',(-0.49954796234089,1.,-4.0275581398015));
#48791=CARTESIAN_POINT('Ctrl Pts',(-0.503321556915514,1.,-4.0342628417439));
#48792=CARTESIAN_POINT('Ctrl Pts',(-0.507132823288362,1.,-4.04095715149074));
#48793=CARTESIAN_POINT('Ctrl Pts',(-0.510981349219174,1.,-4.04764078815591));
#48794=CARTESIAN_POINT('Ctrl Pts',(-0.514866728193104,1.,-4.05431335771261));
#48795=CARTESIAN_POINT('Ctrl Pts',(-0.51878857233681,1.,-4.06097448037934));
#48796=CARTESIAN_POINT('Ctrl Pts',(-0.522746528602768,1.,-4.06762394471075));
#48797=CARTESIAN_POINT('Ctrl Pts',(-0.526740277227,1.,-4.07426172299496));
#48798=CARTESIAN_POINT('Ctrl Pts',(-0.530769518728075,1.,-4.08088789536488));
#48799=CARTESIAN_POINT('Ctrl Pts',(-0.534833963476999,1.,-4.08750259988693));
#48800=CARTESIAN_POINT('Ctrl Pts',(-0.538933321179921,1.,-4.09410597627116));
#48801=CARTESIAN_POINT('Ctrl Pts',(-0.543067286878457,1.,-4.10069810244473));
#48802=CARTESIAN_POINT('Ctrl Pts',(-0.54723553948676,1.,-4.1072789702877));
#48803=CARTESIAN_POINT('Ctrl Pts',(-0.551437758498247,1.,-4.11384852025578));
#48804=CARTESIAN_POINT('Ctrl Pts',(-0.555673636130778,1.,-4.1204066619623));
#48805=CARTESIAN_POINT('Ctrl Pts',(-0.559942890594628,1.,-4.12695329951859));
#48806=CARTESIAN_POINT('Ctrl Pts',(-0.564245279535705,1.,-4.13348835726086));
#48807=CARTESIAN_POINT('Ctrl Pts',(-0.568580610187116,1.,-4.14001179828669));
#48808=CARTESIAN_POINT('Ctrl Pts',(-0.572948736066277,1.,-4.14652361065787));
#48809=CARTESIAN_POINT('Ctrl Pts',(-0.576469391673917,1.,-4.1517237611974));
#48810=CARTESIAN_POINT('Ctrl Pts',(-0.579124568912543,1.,-4.15561864787379));
#48811=CARTESIAN_POINT('Ctrl Pts',(-0.580901211462913,1.,-4.15821291712391));
#48812=CARTESIAN_POINT('Ctrl Pts',(-0.581791163835814,1.,-4.15950947128175));
#48813=CARTESIAN_POINT('Origin',(-0.581791163835814,0.,-4.15950947128175));
#48814=CARTESIAN_POINT('',(-0.732042837400619,1.,-4.13571194405636));
#48815=CARTESIAN_POINT('Origin',(0.,0.,0.));
#48816=CARTESIAN_POINT('',(-0.203156094897896,1.,-3.74449296982994));
#48817=CARTESIAN_POINT('Origin',(0.,1.,0.));
#48818=CARTESIAN_POINT('Ctrl Pts',(-0.203156094897896,1.,-3.74449296982994));
#48819=CARTESIAN_POINT('Ctrl Pts',(-0.203156094897896,0.666666666666667,
-3.74449296982994));
#48820=CARTESIAN_POINT('Ctrl Pts',(-0.203156094897896,0.333333333333333,
-3.74449296982994));
#48821=CARTESIAN_POINT('Ctrl Pts',(-0.203156094897896,-0.333333333333333,
-3.74449296982994));
#48822=CARTESIAN_POINT('Ctrl Pts',(-0.203156094897896,-0.666666666666667,
-3.74449296982994));
#48823=CARTESIAN_POINT('Ctrl Pts',(-0.203156094897896,-1.,-3.74449296982994));
#48824=CARTESIAN_POINT('Ctrl Pts',(-0.0760622897878238,-1.,-4.19931119685982));
#48825=CARTESIAN_POINT('Ctrl Pts',(-0.0760622897878238,1.,-4.19931119685982));
#48826=CARTESIAN_POINT('Ctrl Pts',(-0.0767384596142197,-1.,-4.19789138621624));
#48827=CARTESIAN_POINT('Ctrl Pts',(-0.0767384596142197,1.,-4.19789138621624));
#48828=CARTESIAN_POINT('Ctrl Pts',(-0.0780873956244405,-1.,-4.19505112860624));
#48829=CARTESIAN_POINT('Ctrl Pts',(-0.0780873956244405,1.,-4.19505112860624));
#48830=CARTESIAN_POINT('Ctrl Pts',(-0.0801005887117605,-1.,-4.19078883322483));
#48831=CARTESIAN_POINT('Ctrl Pts',(-0.0801005887117605,1.,-4.19078883322483));
#48832=CARTESIAN_POINT('Ctrl Pts',(-0.0827644164389512,-1.,-4.1851019532944));
#48833=CARTESIAN_POINT('Ctrl Pts',(-0.0827644164389512,1.,-4.1851019532944));
#48834=CARTESIAN_POINT('Ctrl Pts',(-0.0860600915552517,-1.,-4.17798698669991));
#48835=CARTESIAN_POINT('Ctrl Pts',(-0.0860600915552517,1.,-4.17798698669991));
#48836=CARTESIAN_POINT('Ctrl Pts',(-0.089321556085033,-1.,-4.17086566491823));
#48837=CARTESIAN_POINT('Ctrl Pts',(-0.089321556085033,1.,-4.17086566491823));
#48838=CARTESIAN_POINT('Ctrl Pts',(-0.0925486672167692,-1.,-4.16373802265942));
#48839=CARTESIAN_POINT('Ctrl Pts',(-0.0925486672167692,1.,-4.16373802265942));
#48840=CARTESIAN_POINT('Ctrl Pts',(-0.095741240329707,-1.,-4.15660412653006));
#48841=CARTESIAN_POINT('Ctrl Pts',(-0.095741240329707,1.,-4.15660412653006));
#48842=CARTESIAN_POINT('Ctrl Pts',(-0.0988990478899814,-1.,-4.1494640891762));
#48843=CARTESIAN_POINT('Ctrl Pts',(-0.0988990478899814,1.,-4.1494640891762));
#48844=CARTESIAN_POINT('Ctrl Pts',(-0.102021826577454,-1.,-4.14231804938737));
#48845=CARTESIAN_POINT('Ctrl Pts',(-0.102021826577454,1.,-4.14231804938737));
#48846=CARTESIAN_POINT('Ctrl Pts',(-0.105109286538864,-1.,-4.13516614458396));
#48847=CARTESIAN_POINT('Ctrl Pts',(-0.105109286538864,1.,-4.13516614458396));
#48848=CARTESIAN_POINT('Ctrl Pts',(-0.10816112052835,-1.,-4.12800848371386));
#48849=CARTESIAN_POINT('Ctrl Pts',(-0.10816112052835,1.,-4.12800848371386));
#48850=CARTESIAN_POINT('Ctrl Pts',(-0.111177012683377,-1.,-4.12084512502444));
#48851=CARTESIAN_POINT('Ctrl Pts',(-0.111177012683377,1.,-4.12084512502444));
#48852=CARTESIAN_POINT('Ctrl Pts',(-0.114156649609602,-1.,-4.11367603925313));
#48853=CARTESIAN_POINT('Ctrl Pts',(-0.114156649609602,1.,-4.11367603925313));
#48854=CARTESIAN_POINT('Ctrl Pts',(-0.117099722731705,-1.,-4.10650113382187));
#48855=CARTESIAN_POINT('Ctrl Pts',(-0.117099722731705,1.,-4.10650113382187));
#48856=CARTESIAN_POINT('Ctrl Pts',(-0.120005924388162,-1.,-4.09932031767243));
#48857=CARTESIAN_POINT('Ctrl Pts',(-0.120005924388162,1.,-4.09932031767243));
#48858=CARTESIAN_POINT('Ctrl Pts',(-0.122874946249119,-1.,-4.09213355850836));
#48859=CARTESIAN_POINT('Ctrl Pts',(-0.122874946249119,1.,-4.09213355850836));
#48860=CARTESIAN_POINT('Ctrl Pts',(-0.125706476822529,-1.,-4.08494093372315));
#48861=CARTESIAN_POINT('Ctrl Pts',(-0.125706476822529,1.,-4.08494093372315));
#48862=CARTESIAN_POINT('Ctrl Pts',(-0.128500200484814,-1.,-4.07774270738809));
#48863=CARTESIAN_POINT('Ctrl Pts',(-0.128500200484814,1.,-4.07774270738809));
#48864=CARTESIAN_POINT('Ctrl Pts',(-0.131255793548914,-1.,-4.07053931528579));
#48865=CARTESIAN_POINT('Ctrl Pts',(-0.131255793548914,1.,-4.07053931528579));
#48866=CARTESIAN_POINT('Ctrl Pts',(-0.133972916144225,-1.,-4.06333121018476));
#48867=CARTESIAN_POINT('Ctrl Pts',(-0.133972916144225,1.,-4.06333121018476));
#48868=CARTESIAN_POINT('Ctrl Pts',(-0.136651205046111,-1.,-4.05611873400122));
#48869=CARTESIAN_POINT('Ctrl Pts',(-0.136651205046111,1.,-4.05611873400122));
#48870=CARTESIAN_POINT('Ctrl Pts',(-0.13929026718006,-1.,-4.04890199238056));
#48871=CARTESIAN_POINT('Ctrl Pts',(-0.13929026718006,1.,-4.04890199238056));
#48872=CARTESIAN_POINT('Ctrl Pts',(-0.141889671485508,-1.,-4.04168069633842));
#48873=CARTESIAN_POINT('Ctrl Pts',(-0.141889671485508,1.,-4.04168069633842));
#48874=CARTESIAN_POINT('Ctrl Pts',(-0.144448947038352,-1.,-4.03445411510403));
#48875=CARTESIAN_POINT('Ctrl Pts',(-0.144448947038352,1.,-4.03445411510403));
#48876=CARTESIAN_POINT('Ctrl Pts',(-0.146967602878999,-1.,-4.02722143147048));
#48877=CARTESIAN_POINT('Ctrl Pts',(-0.146967602878999,1.,-4.02722143147048));
#48878=CARTESIAN_POINT('Ctrl Pts',(-0.149445144968708,-1.,-4.01998203715588));
#48879=CARTESIAN_POINT('Ctrl Pts',(-0.149445144968708,1.,-4.01998203715588));
#48880=CARTESIAN_POINT('Ctrl Pts',(-0.151881094022909,-1.,-4.01273584234684));
#48881=CARTESIAN_POINT('Ctrl Pts',(-0.151881094022909,1.,-4.01273584234684));
#48882=CARTESIAN_POINT('Ctrl Pts',(-0.15427500487231,-1.,-4.00548360245297));
#48883=CARTESIAN_POINT('Ctrl Pts',(-0.15427500487231,1.,-4.00548360245297));
#48884=CARTESIAN_POINT('Ctrl Pts',(-0.156626481393736,-1.,-3.99822717425869));
#48885=CARTESIAN_POINT('Ctrl Pts',(-0.156626481393736,1.,-3.99822717425869));
#48886=CARTESIAN_POINT('Ctrl Pts',(-0.158935123982796,-1.,-3.99096873945862));
#48887=CARTESIAN_POINT('Ctrl Pts',(-0.158935123982796,1.,-3.99096873945862));
#48888=CARTESIAN_POINT('Ctrl Pts',(-0.161200482186088,-1.,-3.98371010319866));
#48889=CARTESIAN_POINT('Ctrl Pts',(-0.161200482186088,1.,-3.98371010319866));
#48890=CARTESIAN_POINT('Ctrl Pts',(-0.163422004609999,-1.,-3.97645194630944));
#48891=CARTESIAN_POINT('Ctrl Pts',(-0.163422004609999,1.,-3.97645194630944));
#48892=CARTESIAN_POINT('Ctrl Pts',(-0.165598992851098,-1.,-3.9691931362141));
#48893=CARTESIAN_POINT('Ctrl Pts',(-0.165598992851098,1.,-3.9691931362141));
#48894=CARTESIAN_POINT('Ctrl Pts',(-0.167730547023312,-1.,-3.96192990160296));
#48895=CARTESIAN_POINT('Ctrl Pts',(-0.167730547023312,1.,-3.96192990160296));
#48896=CARTESIAN_POINT('Ctrl Pts',(-0.16981566637413,-1.,-3.95465744665263));
#48897=CARTESIAN_POINT('Ctrl Pts',(-0.16981566637413,1.,-3.95465744665263));
#48898=CARTESIAN_POINT('Ctrl Pts',(-0.171853355369233,-1.,-3.94737164900861));
#48899=CARTESIAN_POINT('Ctrl Pts',(-0.171853355369233,1.,-3.94737164900861));
#48900=CARTESIAN_POINT('Ctrl Pts',(-0.173842734974607,-1.,-3.94007083096214));
#48901=CARTESIAN_POINT('Ctrl Pts',(-0.173842734974607,1.,-3.94007083096214));
#48902=CARTESIAN_POINT('Ctrl Pts',(-0.175783136893873,-1.,-3.93275726771049));
#48903=CARTESIAN_POINT('Ctrl Pts',(-0.175783136893873,1.,-3.93275726771049));
#48904=CARTESIAN_POINT('Ctrl Pts',(-0.177674246152328,-1.,-3.92543942697672));
#48905=CARTESIAN_POINT('Ctrl Pts',(-0.177674246152328,1.,-3.92543942697672));
#48906=CARTESIAN_POINT('Ctrl Pts',(-0.179515885822895,-1.,-3.91812876180948));
#48907=CARTESIAN_POINT('Ctrl Pts',(-0.179515885822895,1.,-3.91812876180948));
#48908=CARTESIAN_POINT('Ctrl Pts',(-0.181307740731796,-1.,-3.91083557557193));
#48909=CARTESIAN_POINT('Ctrl Pts',(-0.181307740731796,1.,-3.91083557557193));
#48910=CARTESIAN_POINT('Ctrl Pts',(-0.183049081993193,-1.,-3.90356488555138));
#48911=CARTESIAN_POINT('Ctrl Pts',(-0.183049081993193,1.,-3.90356488555138));
#48912=CARTESIAN_POINT('Ctrl Pts',(-0.184738537728035,-1.,-3.89631300742633));
#48913=CARTESIAN_POINT('Ctrl Pts',(-0.184738537728035,1.,-3.89631300742633));
#48914=CARTESIAN_POINT('Ctrl Pts',(-0.186373724985263,-1.,-3.88906196725817));
#48915=CARTESIAN_POINT('Ctrl Pts',(-0.186373724985263,1.,-3.88906196725817));
#48916=CARTESIAN_POINT('Ctrl Pts',(-0.187951632512663,-1.,-3.88178563496187));
#48917=CARTESIAN_POINT('Ctrl Pts',(-0.187951632512663,1.,-3.88178563496187));
#48918=CARTESIAN_POINT('Ctrl Pts',(-0.189469253358254,-1.,-3.87445976418377));
#48919=CARTESIAN_POINT('Ctrl Pts',(-0.189469253358254,1.,-3.87445976418377));
#48920=CARTESIAN_POINT('Ctrl Pts',(-0.190924190418613,-1.,-3.8670715862477));
#48921=CARTESIAN_POINT('Ctrl Pts',(-0.190924190418613,1.,-3.8670715862477));
#48922=CARTESIAN_POINT('Ctrl Pts',(-0.19231515304498,-1.,-3.85962774407652));
#48923=CARTESIAN_POINT('Ctrl Pts',(-0.19231515304498,1.,-3.85962774407652));
#48924=CARTESIAN_POINT('Ctrl Pts',(-0.193642806777748,-1.,-3.85216762264019));
#48925=CARTESIAN_POINT('Ctrl Pts',(-0.193642806777748,1.,-3.85216762264019));
#48926=CARTESIAN_POINT('Ctrl Pts',(-0.194909009460255,-1.,-3.84475203347052));
#48927=CARTESIAN_POINT('Ctrl Pts',(-0.194909009460255,1.,-3.84475203347052));
#48928=CARTESIAN_POINT('Ctrl Pts',(-0.19611519897189,-1.,-3.83743910616265));
#48929=CARTESIAN_POINT('Ctrl Pts',(-0.19611519897189,1.,-3.83743910616265));
#48930=CARTESIAN_POINT('Ctrl Pts',(-0.197260935827375,-1.,-3.83026221776488));
#48931=CARTESIAN_POINT('Ctrl Pts',(-0.197260935827375,1.,-3.83026221776488));
#48932=CARTESIAN_POINT('Ctrl Pts',(-0.19834261690047,-1.,-3.82321127348981));
#48933=CARTESIAN_POINT('Ctrl Pts',(-0.19834261690047,1.,-3.82321127348981));
#48934=CARTESIAN_POINT('Ctrl Pts',(-0.199351525297396,-1.,-3.81620203429702));
#48935=CARTESIAN_POINT('Ctrl Pts',(-0.199351525297396,1.,-3.81620203429702));
#48936=CARTESIAN_POINT('Ctrl Pts',(-0.20027467943329,-1.,-3.80909529318501));
#48937=CARTESIAN_POINT('Ctrl Pts',(-0.20027467943329,1.,-3.80909529318501));
#48938=CARTESIAN_POINT('Ctrl Pts',(-0.201097756307252,-1.,-3.80175247447171));
#48939=CARTESIAN_POINT('Ctrl Pts',(-0.201097756307252,1.,-3.80175247447171));
#48940=CARTESIAN_POINT('Ctrl Pts',(-0.201807533800799,-1.,-3.79408354187274));
#48941=CARTESIAN_POINT('Ctrl Pts',(-0.201807533800799,1.,-3.79408354187274));
#48942=CARTESIAN_POINT('Ctrl Pts',(-0.202394260512193,-1.,-3.78609175019317));
#48943=CARTESIAN_POINT('Ctrl Pts',(-0.202394260512193,1.,-3.78609175019317));
#48944=CARTESIAN_POINT('Ctrl Pts',(-0.202854729699197,-1.,-3.77793553476879));
#48945=CARTESIAN_POINT('Ctrl Pts',(-0.202854729699197,1.,-3.77793553476879));
#48946=CARTESIAN_POINT('Ctrl Pts',(-0.203192390045337,-1.,-3.76992071595267));
#48947=CARTESIAN_POINT('Ctrl Pts',(-0.203192390045337,1.,-3.76992071595267));
#48948=CARTESIAN_POINT('Ctrl Pts',(-0.203414634707646,-1.,-3.76242717937273));
#48949=CARTESIAN_POINT('Ctrl Pts',(-0.203414634707646,1.,-3.76242717937273));
#48950=CARTESIAN_POINT('Ctrl Pts',(-0.203530796848404,-1.,-3.75585118707924));
#48951=CARTESIAN_POINT('Ctrl Pts',(-0.203530796848404,1.,-3.75585118707924));
#48952=CARTESIAN_POINT('Ctrl Pts',(-0.203550035479097,-1.,-3.75054693397716));
#48953=CARTESIAN_POINT('Ctrl Pts',(-0.203550035479097,1.,-3.75054693397716));
#48954=CARTESIAN_POINT('Ctrl Pts',(-0.20347884453023,-1.,-3.74675472018582));
#48955=CARTESIAN_POINT('Ctrl Pts',(-0.20347884453023,1.,-3.74675472018582));
#48956=CARTESIAN_POINT('Ctrl Pts',(-0.203352057956055,-1.,-3.7450208092684));
#48957=CARTESIAN_POINT('Ctrl Pts',(-0.203352057956055,1.,-3.7450208092684));
#48958=CARTESIAN_POINT('Ctrl Pts',(-0.203218215747895,-1.,-3.74446880195845));
#48959=CARTESIAN_POINT('Ctrl Pts',(-0.203218215747895,1.,-3.74446880195845));
#48960=CARTESIAN_POINT('Ctrl Pts',(-0.20311176758786,-1.,-3.74443319346666));
#48961=CARTESIAN_POINT('Ctrl Pts',(-0.20311176758786,1.,-3.74443319346666));
#48962=CARTESIAN_POINT('Ctrl Pts',(-0.203054238699719,-1.,-3.74449849461127));
#48963=CARTESIAN_POINT('Ctrl Pts',(-0.203054238699719,1.,-3.74449849461127));
#48964=CARTESIAN_POINT('',(-0.0760622897878238,1.,-4.19931119685982));
#48965=CARTESIAN_POINT('Ctrl Pts',(-0.0760622897878238,1.,-4.19931119685982));
#48966=CARTESIAN_POINT('Ctrl Pts',(-0.0767384596142197,1.,-4.19789138621624));
#48967=CARTESIAN_POINT('Ctrl Pts',(-0.0780873956244405,1.,-4.19505112860624));
#48968=CARTESIAN_POINT('Ctrl Pts',(-0.0801005887117605,1.,-4.19078883322483));
#48969=CARTESIAN_POINT('Ctrl Pts',(-0.0827644164389512,1.,-4.1851019532944));
#48970=CARTESIAN_POINT('Ctrl Pts',(-0.0860600915552517,1.,-4.17798698669991));
#48971=CARTESIAN_POINT('Ctrl Pts',(-0.089321556085033,1.,-4.17086566491823));
#48972=CARTESIAN_POINT('Ctrl Pts',(-0.0925486672167692,1.,-4.16373802265942));
#48973=CARTESIAN_POINT('Ctrl Pts',(-0.095741240329707,1.,-4.15660412653006));
#48974=CARTESIAN_POINT('Ctrl Pts',(-0.0988990478899814,1.,-4.1494640891762));
#48975=CARTESIAN_POINT('Ctrl Pts',(-0.102021826577454,1.,-4.14231804938737));
#48976=CARTESIAN_POINT('Ctrl Pts',(-0.105109286538864,1.,-4.13516614458396));
#48977=CARTESIAN_POINT('Ctrl Pts',(-0.10816112052835,1.,-4.12800848371386));
#48978=CARTESIAN_POINT('Ctrl Pts',(-0.111177012683377,1.,-4.12084512502444));
#48979=CARTESIAN_POINT('Ctrl Pts',(-0.114156649609602,1.,-4.11367603925313));
#48980=CARTESIAN_POINT('Ctrl Pts',(-0.117099722731705,1.,-4.10650113382187));
#48981=CARTESIAN_POINT('Ctrl Pts',(-0.120005924388162,1.,-4.09932031767243));
#48982=CARTESIAN_POINT('Ctrl Pts',(-0.122874946249119,1.,-4.09213355850836));
#48983=CARTESIAN_POINT('Ctrl Pts',(-0.125706476822529,1.,-4.08494093372315));
#48984=CARTESIAN_POINT('Ctrl Pts',(-0.128500200484814,1.,-4.07774270738809));
#48985=CARTESIAN_POINT('Ctrl Pts',(-0.131255793548914,1.,-4.07053931528579));
#48986=CARTESIAN_POINT('Ctrl Pts',(-0.133972916144225,1.,-4.06333121018476));
#48987=CARTESIAN_POINT('Ctrl Pts',(-0.136651205046111,1.,-4.05611873400122));
#48988=CARTESIAN_POINT('Ctrl Pts',(-0.13929026718006,1.,-4.04890199238056));
#48989=CARTESIAN_POINT('Ctrl Pts',(-0.141889671485508,1.,-4.04168069633842));
#48990=CARTESIAN_POINT('Ctrl Pts',(-0.144448947038352,1.,-4.03445411510403));
#48991=CARTESIAN_POINT('Ctrl Pts',(-0.146967602878999,1.,-4.02722143147048));
#48992=CARTESIAN_POINT('Ctrl Pts',(-0.149445144968708,1.,-4.01998203715588));
#48993=CARTESIAN_POINT('Ctrl Pts',(-0.151881094022909,1.,-4.01273584234684));
#48994=CARTESIAN_POINT('Ctrl Pts',(-0.15427500487231,1.,-4.00548360245297));
#48995=CARTESIAN_POINT('Ctrl Pts',(-0.156626481393736,1.,-3.99822717425869));
#48996=CARTESIAN_POINT('Ctrl Pts',(-0.158935123982796,1.,-3.99096873945862));
#48997=CARTESIAN_POINT('Ctrl Pts',(-0.161200482186088,1.,-3.98371010319866));
#48998=CARTESIAN_POINT('Ctrl Pts',(-0.163422004609999,1.,-3.97645194630944));
#48999=CARTESIAN_POINT('Ctrl Pts',(-0.165598992851098,1.,-3.9691931362141));
#49000=CARTESIAN_POINT('Ctrl Pts',(-0.167730547023312,1.,-3.96192990160296));
#49001=CARTESIAN_POINT('Ctrl Pts',(-0.16981566637413,1.,-3.95465744665263));
#49002=CARTESIAN_POINT('Ctrl Pts',(-0.171853355369233,1.,-3.94737164900861));
#49003=CARTESIAN_POINT('Ctrl Pts',(-0.173842734974607,1.,-3.94007083096214));
#49004=CARTESIAN_POINT('Ctrl Pts',(-0.175783136893873,1.,-3.93275726771049));
#49005=CARTESIAN_POINT('Ctrl Pts',(-0.177674246152328,1.,-3.92543942697672));
#49006=CARTESIAN_POINT('Ctrl Pts',(-0.179515885822895,1.,-3.91812876180948));
#49007=CARTESIAN_POINT('Ctrl Pts',(-0.181307740731796,1.,-3.91083557557193));
#49008=CARTESIAN_POINT('Ctrl Pts',(-0.183049081993193,1.,-3.90356488555138));
#49009=CARTESIAN_POINT('Ctrl Pts',(-0.184738537728035,1.,-3.89631300742633));
#49010=CARTESIAN_POINT('Ctrl Pts',(-0.186373724985263,1.,-3.88906196725817));
#49011=CARTESIAN_POINT('Ctrl Pts',(-0.187951632512663,1.,-3.88178563496187));
#49012=CARTESIAN_POINT('Ctrl Pts',(-0.189469253358254,1.,-3.87445976418377));
#49013=CARTESIAN_POINT('Ctrl Pts',(-0.190924190418613,1.,-3.8670715862477));
#49014=CARTESIAN_POINT('Ctrl Pts',(-0.19231515304498,1.,-3.85962774407652));
#49015=CARTESIAN_POINT('Ctrl Pts',(-0.193642806777748,1.,-3.85216762264019));
#49016=CARTESIAN_POINT('Ctrl Pts',(-0.194909009460255,1.,-3.84475203347052));
#49017=CARTESIAN_POINT('Ctrl Pts',(-0.19611519897189,1.,-3.83743910616265));
#49018=CARTESIAN_POINT('Ctrl Pts',(-0.197260935827375,1.,-3.83026221776488));
#49019=CARTESIAN_POINT('Ctrl Pts',(-0.19834261690047,1.,-3.82321127348981));
#49020=CARTESIAN_POINT('Ctrl Pts',(-0.199351525297396,1.,-3.81620203429702));
#49021=CARTESIAN_POINT('Ctrl Pts',(-0.20027467943329,1.,-3.80909529318501));
#49022=CARTESIAN_POINT('Ctrl Pts',(-0.201097756307252,1.,-3.80175247447171));
#49023=CARTESIAN_POINT('Ctrl Pts',(-0.201807533800799,1.,-3.79408354187274));
#49024=CARTESIAN_POINT('Ctrl Pts',(-0.202394260512193,1.,-3.78609175019317));
#49025=CARTESIAN_POINT('Ctrl Pts',(-0.202854729699197,1.,-3.77793553476879));
#49026=CARTESIAN_POINT('Ctrl Pts',(-0.203192390045337,1.,-3.76992071595267));
#49027=CARTESIAN_POINT('Ctrl Pts',(-0.203414634707646,1.,-3.76242717937273));
#49028=CARTESIAN_POINT('Ctrl Pts',(-0.203530796848404,1.,-3.75585118707924));
#49029=CARTESIAN_POINT('Ctrl Pts',(-0.203550035479097,1.,-3.75054693397716));
#49030=CARTESIAN_POINT('Ctrl Pts',(-0.203484186269315,1.,-3.74703926501843));
#49031=CARTESIAN_POINT('Ctrl Pts',(-0.203375226874331,1.,-3.74535749969262));
#49032=CARTESIAN_POINT('Ctrl Pts',(-0.203266610111264,1.,-3.74471097893961));
#49033=CARTESIAN_POINT('Ctrl Pts',(-0.203188003947965,1.,-3.74453008995129));
#49034=CARTESIAN_POINT('Ctrl Pts',(-0.203156094897896,1.,-3.74449296982994));
#49035=CARTESIAN_POINT('',(-0.0760622897878238,0.,-4.19931119685982));
#49036=CARTESIAN_POINT('Ctrl Pts',(0.20305423869972,-1.,-3.74449849461127));
#49037=CARTESIAN_POINT('Ctrl Pts',(0.20305423869972,1.,-3.74449849461127));
#49038=CARTESIAN_POINT('Ctrl Pts',(0.203111767587923,-1.,-3.7444331934681));
#49039=CARTESIAN_POINT('Ctrl Pts',(0.203111767587923,1.,-3.7444331934681));
#49040=CARTESIAN_POINT('Ctrl Pts',(0.203218215748058,-1.,-3.7444688019622));
#49041=CARTESIAN_POINT('Ctrl Pts',(0.203218215748058,1.,-3.7444688019622));
#49042=CARTESIAN_POINT('Ctrl Pts',(0.203352057956297,-1.,-3.74502080927395));
#49043=CARTESIAN_POINT('Ctrl Pts',(0.203352057956297,1.,-3.74502080927395));
#49044=CARTESIAN_POINT('Ctrl Pts',(0.203478844530447,-1.,-3.7467547201908));
#49045=CARTESIAN_POINT('Ctrl Pts',(0.203478844530447,1.,-3.7467547201908));
#49046=CARTESIAN_POINT('Ctrl Pts',(0.203550035479166,-1.,-3.75054693397875));
#49047=CARTESIAN_POINT('Ctrl Pts',(0.203550035479166,1.,-3.75054693397875));
#49048=CARTESIAN_POINT('Ctrl Pts',(0.203530796848321,-1.,-3.75585118707734));
#49049=CARTESIAN_POINT('Ctrl Pts',(0.203530796848321,1.,-3.75585118707734));
#49050=CARTESIAN_POINT('Ctrl Pts',(0.203414634707478,-1.,-3.76242717936885));
#49051=CARTESIAN_POINT('Ctrl Pts',(0.203414634707478,1.,-3.76242717936885));
#49052=CARTESIAN_POINT('Ctrl Pts',(0.203192390045164,-1.,-3.7699207159487));
#49053=CARTESIAN_POINT('Ctrl Pts',(0.203192390045164,1.,-3.7699207159487));
#49054=CARTESIAN_POINT('Ctrl Pts',(0.202854729699081,-1.,-3.77793553476614));
#49055=CARTESIAN_POINT('Ctrl Pts',(0.202854729699081,1.,-3.77793553476614));
#49056=CARTESIAN_POINT('Ctrl Pts',(0.20239426051216,-1.,-3.78609175019242));
#49057=CARTESIAN_POINT('Ctrl Pts',(0.20239426051216,1.,-3.78609175019242));
#49058=CARTESIAN_POINT('Ctrl Pts',(0.201807533800837,-1.,-3.7940835418736));
#49059=CARTESIAN_POINT('Ctrl Pts',(0.201807533800837,1.,-3.7940835418736));
#49060=CARTESIAN_POINT('Ctrl Pts',(0.201097756307326,-1.,-3.80175247447337));
#49061=CARTESIAN_POINT('Ctrl Pts',(0.201097756307326,1.,-3.80175247447337));
#49062=CARTESIAN_POINT('Ctrl Pts',(0.200274679433364,-1.,-3.80909529318669));
#49063=CARTESIAN_POINT('Ctrl Pts',(0.200274679433364,1.,-3.80909529318669));
#49064=CARTESIAN_POINT('Ctrl Pts',(0.199351525297447,-1.,-3.81620203429815));
#49065=CARTESIAN_POINT('Ctrl Pts',(0.199351525297447,1.,-3.81620203429815));
#49066=CARTESIAN_POINT('Ctrl Pts',(0.198342616900486,-1.,-3.82321127349016));
#49067=CARTESIAN_POINT('Ctrl Pts',(0.198342616900486,1.,-3.82321127349016));
#49068=CARTESIAN_POINT('Ctrl Pts',(0.197260935827361,-1.,-3.83026221776456));
#49069=CARTESIAN_POINT('Ctrl Pts',(0.197260935827361,1.,-3.83026221776456));
#49070=CARTESIAN_POINT('Ctrl Pts',(0.196115198971859,-1.,-3.83743910616195));
#49071=CARTESIAN_POINT('Ctrl Pts',(0.196115198971859,1.,-3.83743910616195));
#49072=CARTESIAN_POINT('Ctrl Pts',(0.19490900946022,-1.,-3.84475203346977));
#49073=CARTESIAN_POINT('Ctrl Pts',(0.19490900946022,1.,-3.84475203346977));
#49074=CARTESIAN_POINT('Ctrl Pts',(0.193642806777723,-1.,-3.85216762263966));
#49075=CARTESIAN_POINT('Ctrl Pts',(0.193642806777723,1.,-3.85216762263966));
#49076=CARTESIAN_POINT('Ctrl Pts',(0.19231515304497,-1.,-3.85962774407633));
#49077=CARTESIAN_POINT('Ctrl Pts',(0.19231515304497,1.,-3.85962774407633));
#49078=CARTESIAN_POINT('Ctrl Pts',(0.19092419041862,-1.,-3.86707158624783));
#49079=CARTESIAN_POINT('Ctrl Pts',(0.19092419041862,1.,-3.86707158624783));
#49080=CARTESIAN_POINT('Ctrl Pts',(0.189469253358272,-1.,-3.87445976418412));
#49081=CARTESIAN_POINT('Ctrl Pts',(0.189469253358272,1.,-3.87445976418412));
#49082=CARTESIAN_POINT('Ctrl Pts',(0.187951632512685,-1.,-3.88178563496228));
#49083=CARTESIAN_POINT('Ctrl Pts',(0.187951632512685,1.,-3.88178563496228));
#49084=CARTESIAN_POINT('Ctrl Pts',(0.18637372498528,-1.,-3.88906196725848));
#49085=CARTESIAN_POINT('Ctrl Pts',(0.18637372498528,1.,-3.88906196725848));
#49086=CARTESIAN_POINT('Ctrl Pts',(0.184738537728043,-1.,-3.89631300742646));
#49087=CARTESIAN_POINT('Ctrl Pts',(0.184738537728043,1.,-3.89631300742646));
#49088=CARTESIAN_POINT('Ctrl Pts',(0.18304908199319,-1.,-3.90356488555132));
#49089=CARTESIAN_POINT('Ctrl Pts',(0.18304908199319,1.,-3.90356488555132));
#49090=CARTESIAN_POINT('Ctrl Pts',(0.181307740731785,-1.,-3.91083557557175));
#49091=CARTESIAN_POINT('Ctrl Pts',(0.181307740731785,1.,-3.91083557557175));
#49092=CARTESIAN_POINT('Ctrl Pts',(0.179515885822881,-1.,-3.91812876180926));
#49093=CARTESIAN_POINT('Ctrl Pts',(0.179515885822881,1.,-3.91812876180926));
#49094=CARTESIAN_POINT('Ctrl Pts',(0.177674246152317,-1.,-3.92543942697655));
#49095=CARTESIAN_POINT('Ctrl Pts',(0.177674246152317,1.,-3.92543942697655));
#49096=CARTESIAN_POINT('Ctrl Pts',(0.175783136893868,-1.,-3.93275726771042));
#49097=CARTESIAN_POINT('Ctrl Pts',(0.175783136893868,1.,-3.93275726771042));
#49098=CARTESIAN_POINT('Ctrl Pts',(0.173842734974609,-1.,-3.94007083096217));
#49099=CARTESIAN_POINT('Ctrl Pts',(0.173842734974609,1.,-3.94007083096217));
#49100=CARTESIAN_POINT('Ctrl Pts',(0.17185335536924,-1.,-3.94737164900868));
#49101=CARTESIAN_POINT('Ctrl Pts',(0.17185335536924,1.,-3.94737164900868));
#49102=CARTESIAN_POINT('Ctrl Pts',(0.169815666374139,-1.,-3.95465744665268));
#49103=CARTESIAN_POINT('Ctrl Pts',(0.169815666374139,1.,-3.95465744665268));
#49104=CARTESIAN_POINT('Ctrl Pts',(0.167730547023319,-1.,-3.96192990160296));
#49105=CARTESIAN_POINT('Ctrl Pts',(0.167730547023319,1.,-3.96192990160296));
#49106=CARTESIAN_POINT('Ctrl Pts',(0.165598992851102,-1.,-3.96919313621407));
#49107=CARTESIAN_POINT('Ctrl Pts',(0.165598992851102,1.,-3.96919313621407));
#49108=CARTESIAN_POINT('Ctrl Pts',(0.163422004609999,-1.,-3.97645194630943));
#49109=CARTESIAN_POINT('Ctrl Pts',(0.163422004609999,1.,-3.97645194630943));
#49110=CARTESIAN_POINT('Ctrl Pts',(0.161200482186084,-1.,-3.98371010319872));
#49111=CARTESIAN_POINT('Ctrl Pts',(0.161200482186084,1.,-3.98371010319872));
#49112=CARTESIAN_POINT('Ctrl Pts',(0.158935123982793,-1.,-3.99096873945878));
#49113=CARTESIAN_POINT('Ctrl Pts',(0.158935123982793,1.,-3.99096873945878));
#49114=CARTESIAN_POINT('Ctrl Pts',(0.156626481393734,-1.,-3.99822717425893));
#49115=CARTESIAN_POINT('Ctrl Pts',(0.156626481393734,1.,-3.99822717425893));
#49116=CARTESIAN_POINT('Ctrl Pts',(0.15427500487231,-1.,-4.00548360245319));
#49117=CARTESIAN_POINT('Ctrl Pts',(0.15427500487231,1.,-4.00548360245319));
#49118=CARTESIAN_POINT('Ctrl Pts',(0.15188109402291,-1.,-4.01273584234689));
#49119=CARTESIAN_POINT('Ctrl Pts',(0.15188109402291,1.,-4.01273584234689));
#49120=CARTESIAN_POINT('Ctrl Pts',(0.149445144968707,-1.,-4.01998203715564));
#49121=CARTESIAN_POINT('Ctrl Pts',(0.149445144968707,1.,-4.01998203715564));
#49122=CARTESIAN_POINT('Ctrl Pts',(0.146967602878994,-1.,-4.02722143146994));
#49123=CARTESIAN_POINT('Ctrl Pts',(0.146967602878994,1.,-4.02722143146994));
#49124=CARTESIAN_POINT('Ctrl Pts',(0.144448947038344,-1.,-4.03445411510333));
#49125=CARTESIAN_POINT('Ctrl Pts',(0.144448947038344,1.,-4.03445411510333));
#49126=CARTESIAN_POINT('Ctrl Pts',(0.1418896714855,-1.,-4.04168069633781));
#49127=CARTESIAN_POINT('Ctrl Pts',(0.1418896714855,1.,-4.04168069633781));
#49128=CARTESIAN_POINT('Ctrl Pts',(0.139290267180057,-1.,-4.04890199238036));
#49129=CARTESIAN_POINT('Ctrl Pts',(0.139290267180057,1.,-4.04890199238036));
#49130=CARTESIAN_POINT('Ctrl Pts',(0.136651205046119,-1.,-4.05611873400172));
#49131=CARTESIAN_POINT('Ctrl Pts',(0.136651205046119,1.,-4.05611873400172));
#49132=CARTESIAN_POINT('Ctrl Pts',(0.133972916144245,-1.,-4.06333121018596));
#49133=CARTESIAN_POINT('Ctrl Pts',(0.133972916144245,1.,-4.06333121018596));
#49134=CARTESIAN_POINT('Ctrl Pts',(0.13125579354894,-1.,-4.0705393152874));
#49135=CARTESIAN_POINT('Ctrl Pts',(0.13125579354894,1.,-4.0705393152874));
#49136=CARTESIAN_POINT('Ctrl Pts',(0.128500200484837,-1.,-4.07774270738954));
#49137=CARTESIAN_POINT('Ctrl Pts',(0.128500200484837,1.,-4.07774270738954));
#49138=CARTESIAN_POINT('Ctrl Pts',(0.12570647682254,-1.,-4.08494093372377));
#49139=CARTESIAN_POINT('Ctrl Pts',(0.12570647682254,1.,-4.08494093372377));
#49140=CARTESIAN_POINT('Ctrl Pts',(0.122874946249107,-1.,-4.09213355850756));
#49141=CARTESIAN_POINT('Ctrl Pts',(0.122874946249107,1.,-4.09213355850756));
#49142=CARTESIAN_POINT('Ctrl Pts',(0.120005924388124,-1.,-4.09932031767002));
#49143=CARTESIAN_POINT('Ctrl Pts',(0.120005924388124,1.,-4.09932031767002));
#49144=CARTESIAN_POINT('Ctrl Pts',(0.117099722731648,-1.,-4.10650113381833));
#49145=CARTESIAN_POINT('Ctrl Pts',(0.117099722731648,1.,-4.10650113381833));
#49146=CARTESIAN_POINT('Ctrl Pts',(0.114156649609545,-1.,-4.11367603924961));
#49147=CARTESIAN_POINT('Ctrl Pts',(0.114156649609545,1.,-4.11367603924961));
#49148=CARTESIAN_POINT('Ctrl Pts',(0.111177012683346,-1.,-4.1208451250225));
#49149=CARTESIAN_POINT('Ctrl Pts',(0.111177012683346,1.,-4.1208451250225));
#49150=CARTESIAN_POINT('Ctrl Pts',(0.108161120528369,-1.,-4.12800848371504));
#49151=CARTESIAN_POINT('Ctrl Pts',(0.108161120528369,1.,-4.12800848371504));
#49152=CARTESIAN_POINT('Ctrl Pts',(0.105109286538945,-1.,-4.13516614458895));
#49153=CARTESIAN_POINT('Ctrl Pts',(0.105109286538945,1.,-4.13516614458895));
#49154=CARTESIAN_POINT('Ctrl Pts',(0.102021826577584,-1.,-4.14231804939538));
#49155=CARTESIAN_POINT('Ctrl Pts',(0.102021826577584,1.,-4.14231804939538));
#49156=CARTESIAN_POINT('Ctrl Pts',(0.0988990478901223,-1.,-4.14946408918485));
#49157=CARTESIAN_POINT('Ctrl Pts',(0.0988990478901223,1.,-4.14946408918485));
#49158=CARTESIAN_POINT('Ctrl Pts',(0.0957412403298004,-1.,-4.15660412653577));
#49159=CARTESIAN_POINT('Ctrl Pts',(0.0957412403298004,1.,-4.15660412653577));
#49160=CARTESIAN_POINT('Ctrl Pts',(0.0925486672167528,-1.,-4.16373802265839));
#49161=CARTESIAN_POINT('Ctrl Pts',(0.0925486672167528,1.,-4.16373802265839));
#49162=CARTESIAN_POINT('Ctrl Pts',(0.0893215560848647,-1.,-4.17086566490794));
#49163=CARTESIAN_POINT('Ctrl Pts',(0.0893215560848647,1.,-4.17086566490794));
#49164=CARTESIAN_POINT('Ctrl Pts',(0.0860600915549394,-1.,-4.17798698668094));
#49165=CARTESIAN_POINT('Ctrl Pts',(0.0860600915549394,1.,-4.17798698668094));
#49166=CARTESIAN_POINT('Ctrl Pts',(0.0827644164385676,-1.,-4.18510195327123));
#49167=CARTESIAN_POINT('Ctrl Pts',(0.0827644164385676,1.,-4.18510195327123));
#49168=CARTESIAN_POINT('Ctrl Pts',(0.0801005887114317,-1.,-4.19078883320504));
#49169=CARTESIAN_POINT('Ctrl Pts',(0.0801005887114317,1.,-4.19078883320504));
#49170=CARTESIAN_POINT('Ctrl Pts',(0.0780873956242395,-1.,-4.19505112859416));
#49171=CARTESIAN_POINT('Ctrl Pts',(0.0780873956242395,1.,-4.19505112859416));
#49172=CARTESIAN_POINT('Ctrl Pts',(0.0767384596141462,-1.,-4.1978913862118));
#49173=CARTESIAN_POINT('Ctrl Pts',(0.0767384596141462,1.,-4.1978913862118));
#49174=CARTESIAN_POINT('Ctrl Pts',(0.0760622897878244,-1.,-4.19931119685982));
#49175=CARTESIAN_POINT('Ctrl Pts',(0.0760622897878244,1.,-4.19931119685982));
#49176=CARTESIAN_POINT('',(0.203156094896102,1.,-3.74449296983004));
#49177=CARTESIAN_POINT('Ctrl Pts',(0.2031560948961,-1.,-3.74449296983004));
#49178=CARTESIAN_POINT('Ctrl Pts',(0.2031560948961,-0.666666666666667,-3.74449296983004));
#49179=CARTESIAN_POINT('Ctrl Pts',(0.2031560948961,-0.333333333333333,-3.74449296983004));
#49180=CARTESIAN_POINT('Ctrl Pts',(0.2031560948961,0.333333333333333,-3.74449296983004));
#49181=CARTESIAN_POINT('Ctrl Pts',(0.203156094896101,0.666666666666667,
-3.74449296983004));
#49182=CARTESIAN_POINT('Ctrl Pts',(0.203156094896101,1.,-3.74449296983004));
#49183=CARTESIAN_POINT('',(0.0760622897878244,1.,-4.19931119685982));
#49184=CARTESIAN_POINT('',(0.0760622897878244,0.,-4.19931119685982));
#49185=CARTESIAN_POINT('Ctrl Pts',(0.203156094896101,1.,-3.74449296983004));
#49186=CARTESIAN_POINT('Ctrl Pts',(0.203188003946657,1.,-3.74453008995093));
#49187=CARTESIAN_POINT('Ctrl Pts',(0.203266610110531,1.,-3.74471097893845));
#49188=CARTESIAN_POINT('Ctrl Pts',(0.203375226874121,1.,-3.74535749969115));
#49189=CARTESIAN_POINT('Ctrl Pts',(0.203484186269415,1.,-3.74703926501752));
#49190=CARTESIAN_POINT('Ctrl Pts',(0.203550035479166,1.,-3.75054693397875));
#49191=CARTESIAN_POINT('Ctrl Pts',(0.203530796848321,1.,-3.75585118707734));
#49192=CARTESIAN_POINT('Ctrl Pts',(0.203414634707478,1.,-3.76242717936885));
#49193=CARTESIAN_POINT('Ctrl Pts',(0.203192390045164,1.,-3.7699207159487));
#49194=CARTESIAN_POINT('Ctrl Pts',(0.202854729699081,1.,-3.77793553476614));
#49195=CARTESIAN_POINT('Ctrl Pts',(0.20239426051216,1.,-3.78609175019242));
#49196=CARTESIAN_POINT('Ctrl Pts',(0.201807533800837,1.,-3.7940835418736));
#49197=CARTESIAN_POINT('Ctrl Pts',(0.201097756307326,1.,-3.80175247447337));
#49198=CARTESIAN_POINT('Ctrl Pts',(0.200274679433364,1.,-3.80909529318669));
#49199=CARTESIAN_POINT('Ctrl Pts',(0.199351525297447,1.,-3.81620203429815));
#49200=CARTESIAN_POINT('Ctrl Pts',(0.198342616900486,1.,-3.82321127349016));
#49201=CARTESIAN_POINT('Ctrl Pts',(0.197260935827361,1.,-3.83026221776456));
#49202=CARTESIAN_POINT('Ctrl Pts',(0.196115198971859,1.,-3.83743910616195));
#49203=CARTESIAN_POINT('Ctrl Pts',(0.19490900946022,1.,-3.84475203346977));
#49204=CARTESIAN_POINT('Ctrl Pts',(0.193642806777723,1.,-3.85216762263966));
#49205=CARTESIAN_POINT('Ctrl Pts',(0.19231515304497,1.,-3.85962774407633));
#49206=CARTESIAN_POINT('Ctrl Pts',(0.19092419041862,1.,-3.86707158624783));
#49207=CARTESIAN_POINT('Ctrl Pts',(0.189469253358272,1.,-3.87445976418412));
#49208=CARTESIAN_POINT('Ctrl Pts',(0.187951632512685,1.,-3.88178563496228));
#49209=CARTESIAN_POINT('Ctrl Pts',(0.18637372498528,1.,-3.88906196725848));
#49210=CARTESIAN_POINT('Ctrl Pts',(0.184738537728043,1.,-3.89631300742646));
#49211=CARTESIAN_POINT('Ctrl Pts',(0.18304908199319,1.,-3.90356488555132));
#49212=CARTESIAN_POINT('Ctrl Pts',(0.181307740731785,1.,-3.91083557557175));
#49213=CARTESIAN_POINT('Ctrl Pts',(0.179515885822881,1.,-3.91812876180926));
#49214=CARTESIAN_POINT('Ctrl Pts',(0.177674246152317,1.,-3.92543942697655));
#49215=CARTESIAN_POINT('Ctrl Pts',(0.175783136893868,1.,-3.93275726771042));
#49216=CARTESIAN_POINT('Ctrl Pts',(0.173842734974609,1.,-3.94007083096217));
#49217=CARTESIAN_POINT('Ctrl Pts',(0.17185335536924,1.,-3.94737164900868));
#49218=CARTESIAN_POINT('Ctrl Pts',(0.169815666374139,1.,-3.95465744665268));
#49219=CARTESIAN_POINT('Ctrl Pts',(0.167730547023319,1.,-3.96192990160296));
#49220=CARTESIAN_POINT('Ctrl Pts',(0.165598992851102,1.,-3.96919313621407));
#49221=CARTESIAN_POINT('Ctrl Pts',(0.163422004609999,1.,-3.97645194630943));
#49222=CARTESIAN_POINT('Ctrl Pts',(0.161200482186084,1.,-3.98371010319872));
#49223=CARTESIAN_POINT('Ctrl Pts',(0.158935123982793,1.,-3.99096873945878));
#49224=CARTESIAN_POINT('Ctrl Pts',(0.156626481393734,1.,-3.99822717425893));
#49225=CARTESIAN_POINT('Ctrl Pts',(0.15427500487231,1.,-4.00548360245319));
#49226=CARTESIAN_POINT('Ctrl Pts',(0.15188109402291,1.,-4.01273584234689));
#49227=CARTESIAN_POINT('Ctrl Pts',(0.149445144968707,1.,-4.01998203715564));
#49228=CARTESIAN_POINT('Ctrl Pts',(0.146967602878994,1.,-4.02722143146994));
#49229=CARTESIAN_POINT('Ctrl Pts',(0.144448947038344,1.,-4.03445411510333));
#49230=CARTESIAN_POINT('Ctrl Pts',(0.1418896714855,1.,-4.04168069633781));
#49231=CARTESIAN_POINT('Ctrl Pts',(0.139290267180057,1.,-4.04890199238036));
#49232=CARTESIAN_POINT('Ctrl Pts',(0.136651205046119,1.,-4.05611873400172));
#49233=CARTESIAN_POINT('Ctrl Pts',(0.133972916144245,1.,-4.06333121018596));
#49234=CARTESIAN_POINT('Ctrl Pts',(0.13125579354894,1.,-4.0705393152874));
#49235=CARTESIAN_POINT('Ctrl Pts',(0.128500200484837,1.,-4.07774270738954));
#49236=CARTESIAN_POINT('Ctrl Pts',(0.12570647682254,1.,-4.08494093372377));
#49237=CARTESIAN_POINT('Ctrl Pts',(0.122874946249107,1.,-4.09213355850756));
#49238=CARTESIAN_POINT('Ctrl Pts',(0.120005924388124,1.,-4.09932031767002));
#49239=CARTESIAN_POINT('Ctrl Pts',(0.117099722731648,1.,-4.10650113381833));
#49240=CARTESIAN_POINT('Ctrl Pts',(0.114156649609545,1.,-4.11367603924961));
#49241=CARTESIAN_POINT('Ctrl Pts',(0.111177012683346,1.,-4.1208451250225));
#49242=CARTESIAN_POINT('Ctrl Pts',(0.108161120528369,1.,-4.12800848371504));
#49243=CARTESIAN_POINT('Ctrl Pts',(0.105109286538945,1.,-4.13516614458895));
#49244=CARTESIAN_POINT('Ctrl Pts',(0.102021826577584,1.,-4.14231804939538));
#49245=CARTESIAN_POINT('Ctrl Pts',(0.0988990478901223,1.,-4.14946408918485));
#49246=CARTESIAN_POINT('Ctrl Pts',(0.0957412403298004,1.,-4.15660412653577));
#49247=CARTESIAN_POINT('Ctrl Pts',(0.0925486672167528,1.,-4.16373802265839));
#49248=CARTESIAN_POINT('Ctrl Pts',(0.0893215560848647,1.,-4.17086566490794));
#49249=CARTESIAN_POINT('Ctrl Pts',(0.0860600915549394,1.,-4.17798698668094));
#49250=CARTESIAN_POINT('Ctrl Pts',(0.0827644164385676,1.,-4.18510195327123));
#49251=CARTESIAN_POINT('Ctrl Pts',(0.0801005887114317,1.,-4.19078883320504));
#49252=CARTESIAN_POINT('Ctrl Pts',(0.0780873956242395,1.,-4.19505112859416));
#49253=CARTESIAN_POINT('Ctrl Pts',(0.0767384596141462,1.,-4.1978913862118));
#49254=CARTESIAN_POINT('Ctrl Pts',(0.0760622897878244,1.,-4.19931119685982));
#49255=CARTESIAN_POINT('Origin',(0.0760622897878244,0.,-4.19931119685982));
#49256=CARTESIAN_POINT('',(-0.0760622897878238,1.,-4.19931119685982));
#49257=CARTESIAN_POINT('Origin',(0.,0.,0.));
#49258=CARTESIAN_POINT('',(0.385112848330761,1.,-3.73017266276651));
#49259=CARTESIAN_POINT('Origin',(0.,1.,0.));
#49260=CARTESIAN_POINT('Ctrl Pts',(0.385112848330762,1.,-3.73017266276651));
#49261=CARTESIAN_POINT('Ctrl Pts',(0.385112848330762,0.666666666666667,
-3.73017266276651));
#49262=CARTESIAN_POINT('Ctrl Pts',(0.385112848330762,0.333333333333333,
-3.73017266276651));
#49263=CARTESIAN_POINT('Ctrl Pts',(0.385112848330762,-0.333333333333333,
-3.73017266276651));
#49264=CARTESIAN_POINT('Ctrl Pts',(0.385112848330762,-0.666666666666667,
-3.73017266276651));
#49265=CARTESIAN_POINT('Ctrl Pts',(0.385112848330762,-1.,-3.73017266276651));
#49266=CARTESIAN_POINT('Ctrl Pts',(0.581791163835815,-1.,-4.15950947128175));
#49267=CARTESIAN_POINT('Ctrl Pts',(0.581791163835815,1.,-4.15950947128175));
#49268=CARTESIAN_POINT('Ctrl Pts',(0.580901211463535,-1.,-4.1582129171283));
#49269=CARTESIAN_POINT('Ctrl Pts',(0.580901211463535,1.,-4.1582129171283));
#49270=CARTESIAN_POINT('Ctrl Pts',(0.579124568914235,-1.,-4.15561864788576));
#49271=CARTESIAN_POINT('Ctrl Pts',(0.579124568914235,1.,-4.15561864788576));
#49272=CARTESIAN_POINT('Ctrl Pts',(0.576469391676688,-1.,-4.151723761217));
#49273=CARTESIAN_POINT('Ctrl Pts',(0.576469391676688,1.,-4.151723761217));
#49274=CARTESIAN_POINT('Ctrl Pts',(0.572948736069522,-1.,-4.14652361068081));
#49275=CARTESIAN_POINT('Ctrl Pts',(0.572948736069522,1.,-4.14652361068081));
#49276=CARTESIAN_POINT('Ctrl Pts',(0.568580610189774,-1.,-4.14001179830547));
#49277=CARTESIAN_POINT('Ctrl Pts',(0.568580610189774,1.,-4.14001179830547));
#49278=CARTESIAN_POINT('Ctrl Pts',(0.564245279537148,-1.,-4.13348835727104));
#49279=CARTESIAN_POINT('Ctrl Pts',(0.564245279537148,1.,-4.13348835727104));
#49280=CARTESIAN_POINT('Ctrl Pts',(0.559942890594773,-1.,-4.12695329951961));
#49281=CARTESIAN_POINT('Ctrl Pts',(0.559942890594773,1.,-4.12695329951961));
#49282=CARTESIAN_POINT('Ctrl Pts',(0.555673636129977,-1.,-4.12040666195664));
#49283=CARTESIAN_POINT('Ctrl Pts',(0.555673636129977,1.,-4.12040666195664));
#49284=CARTESIAN_POINT('Ctrl Pts',(0.551437758497032,-1.,-4.11384852024721));
#49285=CARTESIAN_POINT('Ctrl Pts',(0.551437758497032,1.,-4.11384852024721));
#49286=CARTESIAN_POINT('Ctrl Pts',(0.547235539485636,-1.,-4.10727897027977));
#49287=CARTESIAN_POINT('Ctrl Pts',(0.547235539485636,1.,-4.10727897027977));
#49288=CARTESIAN_POINT('Ctrl Pts',(0.543067286877757,-1.,-4.10069810243979));
#49289=CARTESIAN_POINT('Ctrl Pts',(0.543067286877757,1.,-4.10069810243979));
#49290=CARTESIAN_POINT('Ctrl Pts',(0.538933321179755,-1.,-4.09410597627));
#49291=CARTESIAN_POINT('Ctrl Pts',(0.538933321179755,1.,-4.09410597627));
#49292=CARTESIAN_POINT('Ctrl Pts',(0.534833963477273,-1.,-4.08750259988885));
#49293=CARTESIAN_POINT('Ctrl Pts',(0.534833963477273,1.,-4.08750259988885));
#49294=CARTESIAN_POINT('Ctrl Pts',(0.53076951872857,-1.,-4.08088789536836));
#49295=CARTESIAN_POINT('Ctrl Pts',(0.53076951872857,1.,-4.08088789536836));
#49296=CARTESIAN_POINT('Ctrl Pts',(0.526740277227498,-1.,-4.07426172299847));
#49297=CARTESIAN_POINT('Ctrl Pts',(0.526740277227498,1.,-4.07426172299847));
#49298=CARTESIAN_POINT('Ctrl Pts',(0.522746528603107,-1.,-4.06762394471314));
#49299=CARTESIAN_POINT('Ctrl Pts',(0.522746528603107,1.,-4.06762394471314));
#49300=CARTESIAN_POINT('Ctrl Pts',(0.518788572336923,-1.,-4.06097448038013));
#49301=CARTESIAN_POINT('Ctrl Pts',(0.518788572336923,1.,-4.06097448038013));
#49302=CARTESIAN_POINT('Ctrl Pts',(0.514866728193016,-1.,-4.05431335771199));
#49303=CARTESIAN_POINT('Ctrl Pts',(0.514866728193016,1.,-4.05431335771199));
#49304=CARTESIAN_POINT('Ctrl Pts',(0.51098134921897,-1.,-4.04764078815447));
#49305=CARTESIAN_POINT('Ctrl Pts',(0.51098134921897,1.,-4.04764078815447));
#49306=CARTESIAN_POINT('Ctrl Pts',(0.507132823288136,-1.,-4.04095715148915));
#49307=CARTESIAN_POINT('Ctrl Pts',(0.507132823288136,1.,-4.04095715148915));
#49308=CARTESIAN_POINT('Ctrl Pts',(0.503321556915346,-1.,-4.03426284174272));
#49309=CARTESIAN_POINT('Ctrl Pts',(0.503321556915346,1.,-4.03426284174272));
#49310=CARTESIAN_POINT('Ctrl Pts',(0.499547962340821,-1.,-4.02755813980101));
#49311=CARTESIAN_POINT('Ctrl Pts',(0.499547962340821,1.,-4.02755813980101));
#49312=CARTESIAN_POINT('Ctrl Pts',(0.495812444326251,-1.,-4.02084308851832));
#49313=CARTESIAN_POINT('Ctrl Pts',(0.495812444326251,1.,-4.02084308851832));
#49314=CARTESIAN_POINT('Ctrl Pts',(0.492115383418018,-1.,-4.01411733503546));
#49315=CARTESIAN_POINT('Ctrl Pts',(0.492115383418018,1.,-4.01411733503546));
#49316=CARTESIAN_POINT('Ctrl Pts',(0.488457130424633,-1.,-4.0073800839099));
#49317=CARTESIAN_POINT('Ctrl Pts',(0.488457130424633,1.,-4.0073800839099));
#49318=CARTESIAN_POINT('Ctrl Pts',(0.484838042421834,-1.,-4.00063045119288));
#49319=CARTESIAN_POINT('Ctrl Pts',(0.484838042421834,1.,-4.00063045119288));
#49320=CARTESIAN_POINT('Ctrl Pts',(0.481258512209675,-1.,-3.99386775880679));
#49321=CARTESIAN_POINT('Ctrl Pts',(0.481258512209675,1.,-3.99386775880679));
#49322=CARTESIAN_POINT('Ctrl Pts',(0.477718999122027,-1.,-3.98709184306738));
#49323=CARTESIAN_POINT('Ctrl Pts',(0.477718999122027,1.,-3.98709184306738));
#49324=CARTESIAN_POINT('Ctrl Pts',(0.474220061019509,-1.,-3.98030338044409));
#49325=CARTESIAN_POINT('Ctrl Pts',(0.474220061019509,1.,-3.98030338044409));
#49326=CARTESIAN_POINT('Ctrl Pts',(0.470762379613439,-1.,-3.97350414289392));
#49327=CARTESIAN_POINT('Ctrl Pts',(0.470762379613439,1.,-3.97350414289392));
#49328=CARTESIAN_POINT('Ctrl Pts',(0.467346690880643,-1.,-3.9666962227393));
#49329=CARTESIAN_POINT('Ctrl Pts',(0.467346690880643,1.,-3.9666962227393));
#49330=CARTESIAN_POINT('Ctrl Pts',(0.463973722115733,-1.,-3.95988133243538));
#49331=CARTESIAN_POINT('Ctrl Pts',(0.463973722115733,1.,-3.95988133243538));
#49332=CARTESIAN_POINT('Ctrl Pts',(0.460644124429121,-1.,-3.95306005817364));
#49333=CARTESIAN_POINT('Ctrl Pts',(0.460644124429121,1.,-3.95306005817364));
#49334=CARTESIAN_POINT('Ctrl Pts',(0.457358410451682,-1.,-3.94623117206678));
#49335=CARTESIAN_POINT('Ctrl Pts',(0.457358410451682,1.,-3.94623117206678));
#49336=CARTESIAN_POINT('Ctrl Pts',(0.454116879027584,-1.,-3.93939080846298));
#49337=CARTESIAN_POINT('Ctrl Pts',(0.454116879027584,1.,-3.93939080846298));
#49338=CARTESIAN_POINT('Ctrl Pts',(0.450919768356348,-1.,-3.93253407403123));
#49339=CARTESIAN_POINT('Ctrl Pts',(0.450919768356348,1.,-3.93253407403123));
#49340=CARTESIAN_POINT('Ctrl Pts',(0.447767416837292,-1.,-3.92565674143416));
#49341=CARTESIAN_POINT('Ctrl Pts',(0.447767416837292,1.,-3.92565674143416));
#49342=CARTESIAN_POINT('Ctrl Pts',(0.44466043023059,-1.,-3.91875701610719));
#49343=CARTESIAN_POINT('Ctrl Pts',(0.44466043023059,1.,-3.91875701610719));
#49344=CARTESIAN_POINT('Ctrl Pts',(0.441599824524054,-1.,-3.91183704069153));
#49345=CARTESIAN_POINT('Ctrl Pts',(0.441599824524054,1.,-3.91183704069153));
#49346=CARTESIAN_POINT('Ctrl Pts',(0.438587235458249,-1.,-3.90490512938563));
#49347=CARTESIAN_POINT('Ctrl Pts',(0.438587235458249,1.,-3.90490512938563));
#49348=CARTESIAN_POINT('Ctrl Pts',(0.435624629433527,-1.,-3.89797256655462));
#49349=CARTESIAN_POINT('Ctrl Pts',(0.435624629433527,1.,-3.89797256655462));
#49350=CARTESIAN_POINT('Ctrl Pts',(0.432713929544458,-1.,-3.89104947940611));
#49351=CARTESIAN_POINT('Ctrl Pts',(0.432713929544458,1.,-3.89104947940611));
#49352=CARTESIAN_POINT('Ctrl Pts',(0.429856640579741,-1.,-3.88414070943341));
#49353=CARTESIAN_POINT('Ctrl Pts',(0.429856640579741,1.,-3.88414070943341));
#49354=CARTESIAN_POINT('Ctrl Pts',(0.427053541173457,-1.,-3.87724240306597));
#49355=CARTESIAN_POINT('Ctrl Pts',(0.427053541173457,1.,-3.87724240306597));
#49356=CARTESIAN_POINT('Ctrl Pts',(0.42430417319511,-1.,-3.87033643487851));
#49357=CARTESIAN_POINT('Ctrl Pts',(0.42430417319511,1.,-3.87033643487851));
#49358=CARTESIAN_POINT('Ctrl Pts',(0.421607423177534,-1.,-3.86339652542709));
#49359=CARTESIAN_POINT('Ctrl Pts',(0.421607423177534,1.,-3.86339652542709));
#49360=CARTESIAN_POINT('Ctrl Pts',(0.418962468086773,-1.,-3.85639825647996));
#49361=CARTESIAN_POINT('Ctrl Pts',(0.418962468086773,1.,-3.85639825647996));
#49362=CARTESIAN_POINT('Ctrl Pts',(0.416369678052906,-1.,-3.84932864157497));
#49363=CARTESIAN_POINT('Ctrl Pts',(0.416369678052906,1.,-3.84932864157497));
#49364=CARTESIAN_POINT('Ctrl Pts',(0.413831367016748,-1.,-3.84219403994762));
#49365=CARTESIAN_POINT('Ctrl Pts',(0.413831367016748,1.,-3.84219403994762));
#49366=CARTESIAN_POINT('Ctrl Pts',(0.411353038798518,-1.,-3.83503345578698));
#49367=CARTESIAN_POINT('Ctrl Pts',(0.411353038798518,1.,-3.83503345578698));
#49368=CARTESIAN_POINT('Ctrl Pts',(0.408942371447459,-1.,-3.82790724256471));
#49369=CARTESIAN_POINT('Ctrl Pts',(0.408942371447459,1.,-3.82790724256471));
#49370=CARTESIAN_POINT('Ctrl Pts',(0.406607038258985,-1.,-3.8208730391381));
#49371=CARTESIAN_POINT('Ctrl Pts',(0.406607038258985,1.,-3.8208730391381));
#49372=CARTESIAN_POINT('Ctrl Pts',(0.404352694628273,-1.,-3.81396374287793));
#49373=CARTESIAN_POINT('Ctrl Pts',(0.404352694628273,1.,-3.81396374287793));
#49374=CARTESIAN_POINT('Ctrl Pts',(0.402181320148435,-1.,-3.80716881962728));
#49375=CARTESIAN_POINT('Ctrl Pts',(0.402181320148435,1.,-3.80716881962728));
#49376=CARTESIAN_POINT('Ctrl Pts',(0.4000883465046,-1.,-3.80040370384546));
#49377=CARTESIAN_POINT('Ctrl Pts',(0.4000883465046,1.,-3.80040370384546));
#49378=CARTESIAN_POINT('Ctrl Pts',(0.398064818683969,-1.,-3.7935288716329));
#49379=CARTESIAN_POINT('Ctrl Pts',(0.398064818683969,1.,-3.7935288716329));
#49380=CARTESIAN_POINT('Ctrl Pts',(0.39610320533484,-1.,-3.78640521279313));
#49381=CARTESIAN_POINT('Ctrl Pts',(0.39610320533484,1.,-3.78640521279313));
#49382=CARTESIAN_POINT('Ctrl Pts',(0.394202481011499,-1.,-3.77894173114283));
#49383=CARTESIAN_POINT('Ctrl Pts',(0.394202481011499,1.,-3.77894173114283));
#49384=CARTESIAN_POINT('Ctrl Pts',(0.392372786223432,-1.,-3.77114011595967));
#49385=CARTESIAN_POINT('Ctrl Pts',(0.392372786223432,1.,-3.77114011595967));
#49386=CARTESIAN_POINT('Ctrl Pts',(0.390642072979559,-1.,-3.76315635033257));
#49387=CARTESIAN_POINT('Ctrl Pts',(0.390642072979559,1.,-3.76315635033257));
#49388=CARTESIAN_POINT('Ctrl Pts',(0.389054775898701,-1.,-3.75529302895152));
#49389=CARTESIAN_POINT('Ctrl Pts',(0.389054775898701,1.,-3.75529302895152));
#49390=CARTESIAN_POINT('Ctrl Pts',(0.387663020050836,-1.,-3.74792651696654));
#49391=CARTESIAN_POINT('Ctrl Pts',(0.387663020050836,1.,-3.74792651696654));
#49392=CARTESIAN_POINT('Ctrl Pts',(0.386519576222251,-1.,-3.74144965781276));
#49393=CARTESIAN_POINT('Ctrl Pts',(0.386519576222251,1.,-3.74144965781276));
#49394=CARTESIAN_POINT('Ctrl Pts',(0.385670806454565,-1.,-3.73621371845318));
#49395=CARTESIAN_POINT('Ctrl Pts',(0.385670806454565,1.,-3.73621371845318));
#49396=CARTESIAN_POINT('Ctrl Pts',(0.385147887988951,-1.,-3.73245705638843));
#49397=CARTESIAN_POINT('Ctrl Pts',(0.385147887988951,1.,-3.73245705638843));
#49398=CARTESIAN_POINT('Ctrl Pts',(0.385001870183213,-1.,-3.73072465900175));
#49399=CARTESIAN_POINT('Ctrl Pts',(0.385001870183213,1.,-3.73072465900175));
#49400=CARTESIAN_POINT('Ctrl Pts',(0.385047711603462,-1.,-3.73015851028356));
#49401=CARTESIAN_POINT('Ctrl Pts',(0.385047711603462,1.,-3.73015851028356));
#49402=CARTESIAN_POINT('Ctrl Pts',(0.385147278814642,-1.,-3.73010668803042));
#49403=CARTESIAN_POINT('Ctrl Pts',(0.385147278814642,1.,-3.73010668803042));
#49404=CARTESIAN_POINT('Ctrl Pts',(0.385214314776329,-1.,-3.73016218570874));
#49405=CARTESIAN_POINT('Ctrl Pts',(0.385214314776329,1.,-3.73016218570874));
#49406=CARTESIAN_POINT('',(0.581791163835815,1.,-4.15950947128175));
#49407=CARTESIAN_POINT('Ctrl Pts',(0.581791163835815,1.,-4.15950947128175));
#49408=CARTESIAN_POINT('Ctrl Pts',(0.580901211463535,1.,-4.1582129171283));
#49409=CARTESIAN_POINT('Ctrl Pts',(0.579124568914235,1.,-4.15561864788576));
#49410=CARTESIAN_POINT('Ctrl Pts',(0.576469391676688,1.,-4.151723761217));
#49411=CARTESIAN_POINT('Ctrl Pts',(0.572948736069522,1.,-4.14652361068081));
#49412=CARTESIAN_POINT('Ctrl Pts',(0.568580610189774,1.,-4.14001179830547));
#49413=CARTESIAN_POINT('Ctrl Pts',(0.564245279537148,1.,-4.13348835727104));
#49414=CARTESIAN_POINT('Ctrl Pts',(0.559942890594773,1.,-4.12695329951961));
#49415=CARTESIAN_POINT('Ctrl Pts',(0.555673636129977,1.,-4.12040666195664));
#49416=CARTESIAN_POINT('Ctrl Pts',(0.551437758497032,1.,-4.11384852024721));
#49417=CARTESIAN_POINT('Ctrl Pts',(0.547235539485636,1.,-4.10727897027977));
#49418=CARTESIAN_POINT('Ctrl Pts',(0.543067286877757,1.,-4.10069810243979));
#49419=CARTESIAN_POINT('Ctrl Pts',(0.538933321179755,1.,-4.09410597627));
#49420=CARTESIAN_POINT('Ctrl Pts',(0.534833963477273,1.,-4.08750259988885));
#49421=CARTESIAN_POINT('Ctrl Pts',(0.53076951872857,1.,-4.08088789536836));
#49422=CARTESIAN_POINT('Ctrl Pts',(0.526740277227498,1.,-4.07426172299847));
#49423=CARTESIAN_POINT('Ctrl Pts',(0.522746528603107,1.,-4.06762394471314));
#49424=CARTESIAN_POINT('Ctrl Pts',(0.518788572336923,1.,-4.06097448038013));
#49425=CARTESIAN_POINT('Ctrl Pts',(0.514866728193016,1.,-4.05431335771199));
#49426=CARTESIAN_POINT('Ctrl Pts',(0.51098134921897,1.,-4.04764078815447));
#49427=CARTESIAN_POINT('Ctrl Pts',(0.507132823288136,1.,-4.04095715148915));
#49428=CARTESIAN_POINT('Ctrl Pts',(0.503321556915346,1.,-4.03426284174272));
#49429=CARTESIAN_POINT('Ctrl Pts',(0.499547962340821,1.,-4.02755813980101));
#49430=CARTESIAN_POINT('Ctrl Pts',(0.495812444326251,1.,-4.02084308851832));
#49431=CARTESIAN_POINT('Ctrl Pts',(0.492115383418018,1.,-4.01411733503546));
#49432=CARTESIAN_POINT('Ctrl Pts',(0.488457130424633,1.,-4.0073800839099));
#49433=CARTESIAN_POINT('Ctrl Pts',(0.484838042421834,1.,-4.00063045119288));
#49434=CARTESIAN_POINT('Ctrl Pts',(0.481258512209675,1.,-3.99386775880679));
#49435=CARTESIAN_POINT('Ctrl Pts',(0.477718999122027,1.,-3.98709184306738));
#49436=CARTESIAN_POINT('Ctrl Pts',(0.474220061019509,1.,-3.98030338044409));
#49437=CARTESIAN_POINT('Ctrl Pts',(0.470762379613439,1.,-3.97350414289392));
#49438=CARTESIAN_POINT('Ctrl Pts',(0.467346690880643,1.,-3.9666962227393));
#49439=CARTESIAN_POINT('Ctrl Pts',(0.463973722115733,1.,-3.95988133243538));
#49440=CARTESIAN_POINT('Ctrl Pts',(0.460644124429121,1.,-3.95306005817364));
#49441=CARTESIAN_POINT('Ctrl Pts',(0.457358410451682,1.,-3.94623117206678));
#49442=CARTESIAN_POINT('Ctrl Pts',(0.454116879027584,1.,-3.93939080846298));
#49443=CARTESIAN_POINT('Ctrl Pts',(0.450919768356348,1.,-3.93253407403123));
#49444=CARTESIAN_POINT('Ctrl Pts',(0.447767416837292,1.,-3.92565674143416));
#49445=CARTESIAN_POINT('Ctrl Pts',(0.44466043023059,1.,-3.91875701610719));
#49446=CARTESIAN_POINT('Ctrl Pts',(0.441599824524054,1.,-3.91183704069153));
#49447=CARTESIAN_POINT('Ctrl Pts',(0.438587235458249,1.,-3.90490512938563));
#49448=CARTESIAN_POINT('Ctrl Pts',(0.435624629433527,1.,-3.89797256655462));
#49449=CARTESIAN_POINT('Ctrl Pts',(0.432713929544458,1.,-3.89104947940611));
#49450=CARTESIAN_POINT('Ctrl Pts',(0.429856640579741,1.,-3.88414070943341));
#49451=CARTESIAN_POINT('Ctrl Pts',(0.427053541173457,1.,-3.87724240306597));
#49452=CARTESIAN_POINT('Ctrl Pts',(0.42430417319511,1.,-3.87033643487851));
#49453=CARTESIAN_POINT('Ctrl Pts',(0.421607423177534,1.,-3.86339652542709));
#49454=CARTESIAN_POINT('Ctrl Pts',(0.418962468086773,1.,-3.85639825647996));
#49455=CARTESIAN_POINT('Ctrl Pts',(0.416369678052906,1.,-3.84932864157497));
#49456=CARTESIAN_POINT('Ctrl Pts',(0.413831367016748,1.,-3.84219403994762));
#49457=CARTESIAN_POINT('Ctrl Pts',(0.411353038798518,1.,-3.83503345578698));
#49458=CARTESIAN_POINT('Ctrl Pts',(0.408942371447459,1.,-3.82790724256471));
#49459=CARTESIAN_POINT('Ctrl Pts',(0.406607038258985,1.,-3.8208730391381));
#49460=CARTESIAN_POINT('Ctrl Pts',(0.404352694628273,1.,-3.81396374287793));
#49461=CARTESIAN_POINT('Ctrl Pts',(0.402181320148435,1.,-3.80716881962728));
#49462=CARTESIAN_POINT('Ctrl Pts',(0.4000883465046,1.,-3.80040370384546));
#49463=CARTESIAN_POINT('Ctrl Pts',(0.398064818683969,1.,-3.7935288716329));
#49464=CARTESIAN_POINT('Ctrl Pts',(0.39610320533484,1.,-3.78640521279313));
#49465=CARTESIAN_POINT('Ctrl Pts',(0.394202481011499,1.,-3.77894173114283));
#49466=CARTESIAN_POINT('Ctrl Pts',(0.392372786223432,1.,-3.77114011595967));
#49467=CARTESIAN_POINT('Ctrl Pts',(0.390642072979559,1.,-3.76315635033257));
#49468=CARTESIAN_POINT('Ctrl Pts',(0.389054775898701,1.,-3.75529302895152));
#49469=CARTESIAN_POINT('Ctrl Pts',(0.387663020050836,1.,-3.74792651696654));
#49470=CARTESIAN_POINT('Ctrl Pts',(0.386519576222251,1.,-3.74144965781276));
#49471=CARTESIAN_POINT('Ctrl Pts',(0.385670806454565,1.,-3.73621371845318));
#49472=CARTESIAN_POINT('Ctrl Pts',(0.385187124634206,1.,-3.73273893363406));
#49473=CARTESIAN_POINT('Ctrl Pts',(0.385031656499163,1.,-3.73106082862548));
#49474=CARTESIAN_POINT('Ctrl Pts',(0.385037797881504,1.,-3.73040527621055));
#49475=CARTESIAN_POINT('Ctrl Pts',(0.385087139000374,1.,-3.73021431755274));
#49476=CARTESIAN_POINT('Ctrl Pts',(0.385112848330761,1.,-3.73017266276651));
#49477=CARTESIAN_POINT('',(0.581791163835815,0.,-4.15950947128175));
#49478=CARTESIAN_POINT('Ctrl Pts',(0.786322922920599,-1.,-3.66663282329846));
#49479=CARTESIAN_POINT('Ctrl Pts',(0.786322922920599,1.,-3.66663282329846));
#49480=CARTESIAN_POINT('Ctrl Pts',(0.786369528183326,-1.,-3.66655932661986));
#49481=CARTESIAN_POINT('Ctrl Pts',(0.786369528183326,1.,-3.66655932661986));
#49482=CARTESIAN_POINT('Ctrl Pts',(0.786480236185696,-1.,-3.66657784455334));
#49483=CARTESIAN_POINT('Ctrl Pts',(0.786480236185696,1.,-3.66657784455334));
#49484=CARTESIAN_POINT('Ctrl Pts',(0.786698783542764,-1.,-3.66710211820482));
#49485=CARTESIAN_POINT('Ctrl Pts',(0.786698783542764,1.,-3.66710211820482));
#49486=CARTESIAN_POINT('Ctrl Pts',(0.787095252590501,-1.,-3.66879484801113));
#49487=CARTESIAN_POINT('Ctrl Pts',(0.787095252590501,1.,-3.66879484801113));
#49488=CARTESIAN_POINT('Ctrl Pts',(0.787758799995742,-1.,-3.67252923663655));
#49489=CARTESIAN_POINT('Ctrl Pts',(0.787758799995742,1.,-3.67252923663655));
#49490=CARTESIAN_POINT('Ctrl Pts',(0.788569566220285,-1.,-3.67777119516252));
#49491=CARTESIAN_POINT('Ctrl Pts',(0.788569566220285,1.,-3.67777119516252));
#49492=CARTESIAN_POINT('Ctrl Pts',(0.789483546064386,-1.,-3.68428439783905));
#49493=CARTESIAN_POINT('Ctrl Pts',(0.789483546064386,1.,-3.68428439783905));
#49494=CARTESIAN_POINT('Ctrl Pts',(0.790436284988787,-1.,-3.69172044327364));
#49495=CARTESIAN_POINT('Ctrl Pts',(0.790436284988787,1.,-3.69172044327364));
#49496=CARTESIAN_POINT('Ctrl Pts',(0.79135657569598,-1.,-3.69968940808721));
#49497=CARTESIAN_POINT('Ctrl Pts',(0.79135657569598,1.,-3.69968940808721));
#49498=CARTESIAN_POINT('Ctrl Pts',(0.792177688845817,-1.,-3.70781724021806));
#49499=CARTESIAN_POINT('Ctrl Pts',(0.792177688845817,1.,-3.70781724021806));
#49500=CARTESIAN_POINT('Ctrl Pts',(0.792848377370287,-1.,-3.71580242396124));
#49501=CARTESIAN_POINT('Ctrl Pts',(0.792848377370287,1.,-3.71580242396124));
#49502=CARTESIAN_POINT('Ctrl Pts',(0.793347023784204,-1.,-3.72348797293734));
#49503=CARTESIAN_POINT('Ctrl Pts',(0.793347023784204,1.,-3.72348797293734));
#49504=CARTESIAN_POINT('Ctrl Pts',(0.793682750269684,-1.,-3.73086914695805));
#49505=CARTESIAN_POINT('Ctrl Pts',(0.793682750269684,1.,-3.73086914695805));
#49506=CARTESIAN_POINT('Ctrl Pts',(0.793882700937016,-1.,-3.73803280541687));
#49507=CARTESIAN_POINT('Ctrl Pts',(0.793882700937016,1.,-3.73803280541687));
#49508=CARTESIAN_POINT('Ctrl Pts',(0.793982700459951,-1.,-3.74511357728861));
#49509=CARTESIAN_POINT('Ctrl Pts',(0.793982700459951,1.,-3.74511357728861));
#49510=CARTESIAN_POINT('Ctrl Pts',(0.794017347371377,-1.,-3.75224692493864));
#49511=CARTESIAN_POINT('Ctrl Pts',(0.794017347371377,1.,-3.75224692493864));
#49512=CARTESIAN_POINT('Ctrl Pts',(0.794008429134907,-1.,-3.75951468666257));
#49513=CARTESIAN_POINT('Ctrl Pts',(0.794008429134907,1.,-3.75951468666257));
#49514=CARTESIAN_POINT('Ctrl Pts',(0.793961083688991,-1.,-3.76692626931111));
#49515=CARTESIAN_POINT('Ctrl Pts',(0.793961083688991,1.,-3.76692626931111));
#49516=CARTESIAN_POINT('Ctrl Pts',(0.793870523787407,-1.,-3.77444863801212));
#49517=CARTESIAN_POINT('Ctrl Pts',(0.793870523787407,1.,-3.77444863801212));
#49518=CARTESIAN_POINT('Ctrl Pts',(0.7937262357813,-1.,-3.78202460377598));
#49519=CARTESIAN_POINT('Ctrl Pts',(0.7937262357813,1.,-3.78202460377598));
#49520=CARTESIAN_POINT('Ctrl Pts',(0.793516871680993,-1.,-3.78959439439235));
#49521=CARTESIAN_POINT('Ctrl Pts',(0.793516871680993,1.,-3.78959439439235));
#49522=CARTESIAN_POINT('Ctrl Pts',(0.793235612973273,-1.,-3.79711921389897));
#49523=CARTESIAN_POINT('Ctrl Pts',(0.793235612973273,1.,-3.79711921389897));
#49524=CARTESIAN_POINT('Ctrl Pts',(0.792882695234777,-1.,-3.80459229925637));
#49525=CARTESIAN_POINT('Ctrl Pts',(0.792882695234777,1.,-3.80459229925637));
#49526=CARTESIAN_POINT('Ctrl Pts',(0.792462483517634,-1.,-3.81202588694756));
#49527=CARTESIAN_POINT('Ctrl Pts',(0.792462483517634,1.,-3.81202588694756));
#49528=CARTESIAN_POINT('Ctrl Pts',(0.791981740718634,-1.,-3.81944345442249));
#49529=CARTESIAN_POINT('Ctrl Pts',(0.791981740718634,1.,-3.81944345442249));
#49530=CARTESIAN_POINT('Ctrl Pts',(0.791447528662369,-1.,-3.82687033899792));
#49531=CARTESIAN_POINT('Ctrl Pts',(0.791447528662369,1.,-3.82687033899792));
#49532=CARTESIAN_POINT('Ctrl Pts',(0.7908650127053,-1.,-3.83432392054786));
#49533=CARTESIAN_POINT('Ctrl Pts',(0.7908650127053,1.,-3.83432392054786));
#49534=CARTESIAN_POINT('Ctrl Pts',(0.790236124191242,-1.,-3.84180762342454));
#49535=CARTESIAN_POINT('Ctrl Pts',(0.790236124191242,1.,-3.84180762342454));
#49536=CARTESIAN_POINT('Ctrl Pts',(0.789560798155582,-1.,-3.84931637808894));
#49537=CARTESIAN_POINT('Ctrl Pts',(0.789560798155582,1.,-3.84931637808894));
#49538=CARTESIAN_POINT('Ctrl Pts',(0.788837734090671,-1.,-3.85683995872529));
#49539=CARTESIAN_POINT('Ctrl Pts',(0.788837734090671,1.,-3.85683995872529));
#49540=CARTESIAN_POINT('Ctrl Pts',(0.788065315093777,-1.,-3.86436702561345));
#49541=CARTESIAN_POINT('Ctrl Pts',(0.788065315093777,1.,-3.86436702561345));
#49542=CARTESIAN_POINT('Ctrl Pts',(0.787242527617999,-1.,-3.87188916600912));
#49543=CARTESIAN_POINT('Ctrl Pts',(0.787242527617999,1.,-3.87188916600912));
#49544=CARTESIAN_POINT('Ctrl Pts',(0.786369675812608,-1.,-3.8794040281819));
#49545=CARTESIAN_POINT('Ctrl Pts',(0.786369675812608,1.,-3.8794040281819));
#49546=CARTESIAN_POINT('Ctrl Pts',(0.78544789034073,-1.,-3.88691313167398));
#49547=CARTESIAN_POINT('Ctrl Pts',(0.78544789034073,1.,-3.88691313167398));
#49548=CARTESIAN_POINT('Ctrl Pts',(0.784478799358336,-1.,-3.89442039235103));
#49549=CARTESIAN_POINT('Ctrl Pts',(0.784478799358336,1.,-3.89442039235103));
#49550=CARTESIAN_POINT('Ctrl Pts',(0.783464141529081,-1.,-3.9019303904397));
#49551=CARTESIAN_POINT('Ctrl Pts',(0.783464141529081,1.,-3.9019303904397));
#49552=CARTESIAN_POINT('Ctrl Pts',(0.782405395622764,-1.,-3.90944671004542));
#49553=CARTESIAN_POINT('Ctrl Pts',(0.782405395622764,1.,-3.90944671004542));
#49554=CARTESIAN_POINT('Ctrl Pts',(0.781303428618366,-1.,-3.91697036054676));
#49555=CARTESIAN_POINT('Ctrl Pts',(0.781303428618366,1.,-3.91697036054676));
#49556=CARTESIAN_POINT('Ctrl Pts',(0.780158678615542,-1.,-3.92450058323823));
#49557=CARTESIAN_POINT('Ctrl Pts',(0.780158678615542,1.,-3.92450058323823));
#49558=CARTESIAN_POINT('Ctrl Pts',(0.77897130813482,-1.,-3.93203552473174));
#49559=CARTESIAN_POINT('Ctrl Pts',(0.77897130813482,1.,-3.93203552473174));
#49560=CARTESIAN_POINT('Ctrl Pts',(0.777741370568558,-1.,-3.93957296768103));
#49561=CARTESIAN_POINT('Ctrl Pts',(0.777741370568558,1.,-3.93957296768103));
#49562=CARTESIAN_POINT('Ctrl Pts',(0.776468966697921,-1.,-3.94711101619447));
#49563=CARTESIAN_POINT('Ctrl Pts',(0.776468966697921,1.,-3.94711101619447));
#49564=CARTESIAN_POINT('Ctrl Pts',(0.775154418039351,-1.,-3.9546488545231));
#49565=CARTESIAN_POINT('Ctrl Pts',(0.775154418039351,1.,-3.9546488545231));
#49566=CARTESIAN_POINT('Ctrl Pts',(0.773798212026565,-1.,-3.96218649639807));
#49567=CARTESIAN_POINT('Ctrl Pts',(0.773798212026565,1.,-3.96218649639807));
#49568=CARTESIAN_POINT('Ctrl Pts',(0.772400931772136,-1.,-3.96972446532772));
#49569=CARTESIAN_POINT('Ctrl Pts',(0.772400931772136,1.,-3.96972446532772));
#49570=CARTESIAN_POINT('Ctrl Pts',(0.77096319003047,-1.,-3.97726349165488));
#49571=CARTESIAN_POINT('Ctrl Pts',(0.77096319003047,1.,-3.97726349165488));
#49572=CARTESIAN_POINT('Ctrl Pts',(0.769485566245544,-1.,-3.98480422348451));
#49573=CARTESIAN_POINT('Ctrl Pts',(0.769485566245544,1.,-3.98480422348451));
#49574=CARTESIAN_POINT('Ctrl Pts',(0.767968531377914,-1.,-3.9923468788101));
#49575=CARTESIAN_POINT('Ctrl Pts',(0.767968531377914,1.,-3.9923468788101));
#49576=CARTESIAN_POINT('Ctrl Pts',(0.766412457136063,-1.,-3.99989129179622));
#49577=CARTESIAN_POINT('Ctrl Pts',(0.766412457136063,1.,-3.99989129179622));
#49578=CARTESIAN_POINT('Ctrl Pts',(0.764817648785197,-1.,-4.00743706791509));
#49579=CARTESIAN_POINT('Ctrl Pts',(0.764817648785197,1.,-4.00743706791509));
#49580=CARTESIAN_POINT('Ctrl Pts',(0.763184371182935,-1.,-4.01498370680496));
#49581=CARTESIAN_POINT('Ctrl Pts',(0.763184371182935,1.,-4.01498370680496));
#49582=CARTESIAN_POINT('Ctrl Pts',(0.761512875859804,-1.,-4.02253072741268));
#49583=CARTESIAN_POINT('Ctrl Pts',(0.761512875859804,1.,-4.02253072741268));
#49584=CARTESIAN_POINT('Ctrl Pts',(0.759803433243751,-1.,-4.03007781954412));
#49585=CARTESIAN_POINT('Ctrl Pts',(0.759803433243751,1.,-4.03007781954412));
#49586=CARTESIAN_POINT('Ctrl Pts',(0.758056338884944,-1.,-4.03762485803119));
#49587=CARTESIAN_POINT('Ctrl Pts',(0.758056338884944,1.,-4.03762485803119));
#49588=CARTESIAN_POINT('Ctrl Pts',(0.75627190236958,-1.,-4.04517182653997));
#49589=CARTESIAN_POINT('Ctrl Pts',(0.75627190236958,1.,-4.04517182653997));
#49590=CARTESIAN_POINT('Ctrl Pts',(0.754450441816078,-1.,-4.05271876687915));
#49591=CARTESIAN_POINT('Ctrl Pts',(0.754450441816078,1.,-4.05271876687915));
#49592=CARTESIAN_POINT('Ctrl Pts',(0.752592276483072,-1.,-4.06026572221515));
#49593=CARTESIAN_POINT('Ctrl Pts',(0.752592276483072,1.,-4.06026572221515));
#49594=CARTESIAN_POINT('Ctrl Pts',(0.750697720484036,-1.,-4.06781267242378));
#49595=CARTESIAN_POINT('Ctrl Pts',(0.750697720484036,1.,-4.06781267242378));
#49596=CARTESIAN_POINT('Ctrl Pts',(0.748767076680557,-1.,-4.07535951056152));
#49597=CARTESIAN_POINT('Ctrl Pts',(0.748767076680557,1.,-4.07535951056152));
#49598=CARTESIAN_POINT('Ctrl Pts',(0.746800631492315,-1.,-4.08290608095642));
#49599=CARTESIAN_POINT('Ctrl Pts',(0.746800631492315,1.,-4.08290608095642));
#49600=CARTESIAN_POINT('Ctrl Pts',(0.7447986497065,-1.,-4.09045220253573));
#49601=CARTESIAN_POINT('Ctrl Pts',(0.7447986497065,1.,-4.09045220253573));
#49602=CARTESIAN_POINT('Ctrl Pts',(0.742761369689841,-1.,-4.09799769702611));
#49603=CARTESIAN_POINT('Ctrl Pts',(0.742761369689841,1.,-4.09799769702611));
#49604=CARTESIAN_POINT('Ctrl Pts',(0.740688998553376,-1.,-4.10554241757547));
#49605=CARTESIAN_POINT('Ctrl Pts',(0.740688998553376,1.,-4.10554241757547));
#49606=CARTESIAN_POINT('Ctrl Pts',(0.738581708225843,-1.,-4.11308626951927));
#49607=CARTESIAN_POINT('Ctrl Pts',(0.738581708225843,1.,-4.11308626951927));
#49608=CARTESIAN_POINT('Ctrl Pts',(0.736439634331344,-1.,-4.120629196238));
#49609=CARTESIAN_POINT('Ctrl Pts',(0.736439634331344,1.,-4.120629196238));
#49610=CARTESIAN_POINT('Ctrl Pts',(0.734698226764092,-1.,-4.12666277570844));
#49611=CARTESIAN_POINT('Ctrl Pts',(0.734698226764092,1.,-4.12666277570844));
#49612=CARTESIAN_POINT('Ctrl Pts',(0.733376589323546,-1.,-4.13118752795207));
#49613=CARTESIAN_POINT('Ctrl Pts',(0.733376589323546,1.,-4.13118752795207));
#49614=CARTESIAN_POINT('Ctrl Pts',(0.732488575135159,-1.,-4.1342038373684));
#49615=CARTESIAN_POINT('Ctrl Pts',(0.732488575135159,1.,-4.1342038373684));
#49616=CARTESIAN_POINT('Ctrl Pts',(0.73204283740062,-1.,-4.13571194405636));
#49617=CARTESIAN_POINT('Ctrl Pts',(0.73204283740062,1.,-4.13571194405636));
#49618=CARTESIAN_POINT('',(0.786422660831986,1.,-3.66661143271685));
#49619=CARTESIAN_POINT('Ctrl Pts',(0.786422660831985,-1.,-3.66661143271685));
#49620=CARTESIAN_POINT('Ctrl Pts',(0.786422660831985,-0.666666666666667,
-3.66661143271685));
#49621=CARTESIAN_POINT('Ctrl Pts',(0.786422660831985,-0.333333333333333,
-3.66661143271685));
#49622=CARTESIAN_POINT('Ctrl Pts',(0.786422660831985,0.333333333333333,
-3.66661143271685));
#49623=CARTESIAN_POINT('Ctrl Pts',(0.786422660831985,0.666666666666667,
-3.66661143271685));
#49624=CARTESIAN_POINT('Ctrl Pts',(0.786422660831985,1.,-3.66661143271685));
#49625=CARTESIAN_POINT('',(0.73204283740062,1.,-4.13571194405636));
#49626=CARTESIAN_POINT('',(0.73204283740062,0.,-4.13571194405636));
#49627=CARTESIAN_POINT('Ctrl Pts',(0.786422660831986,1.,-3.66661143271685));
#49628=CARTESIAN_POINT('Ctrl Pts',(0.786459983895432,1.,-3.6666431041522));
#49629=CARTESIAN_POINT('Ctrl Pts',(0.786565919558984,1.,-3.66680946938293));
#49630=CARTESIAN_POINT('Ctrl Pts',(0.786774337198062,1.,-3.66743103898702));
#49631=CARTESIAN_POINT('Ctrl Pts',(0.787145041181546,1.,-3.66907505398677));
#49632=CARTESIAN_POINT('Ctrl Pts',(0.787758799995742,1.,-3.67252923663655));
#49633=CARTESIAN_POINT('Ctrl Pts',(0.788569566220285,1.,-3.67777119516252));
#49634=CARTESIAN_POINT('Ctrl Pts',(0.789483546064386,1.,-3.68428439783905));
#49635=CARTESIAN_POINT('Ctrl Pts',(0.790436284988787,1.,-3.69172044327364));
#49636=CARTESIAN_POINT('Ctrl Pts',(0.79135657569598,1.,-3.69968940808721));
#49637=CARTESIAN_POINT('Ctrl Pts',(0.792177688845817,1.,-3.70781724021806));
#49638=CARTESIAN_POINT('Ctrl Pts',(0.792848377370287,1.,-3.71580242396124));
#49639=CARTESIAN_POINT('Ctrl Pts',(0.793347023784204,1.,-3.72348797293734));
#49640=CARTESIAN_POINT('Ctrl Pts',(0.793682750269684,1.,-3.73086914695805));
#49641=CARTESIAN_POINT('Ctrl Pts',(0.793882700937016,1.,-3.73803280541687));
#49642=CARTESIAN_POINT('Ctrl Pts',(0.793982700459951,1.,-3.74511357728861));
#49643=CARTESIAN_POINT('Ctrl Pts',(0.794017347371377,1.,-3.75224692493864));
#49644=CARTESIAN_POINT('Ctrl Pts',(0.794008429134907,1.,-3.75951468666257));
#49645=CARTESIAN_POINT('Ctrl Pts',(0.793961083688991,1.,-3.76692626931111));
#49646=CARTESIAN_POINT('Ctrl Pts',(0.793870523787407,1.,-3.77444863801212));
#49647=CARTESIAN_POINT('Ctrl Pts',(0.7937262357813,1.,-3.78202460377598));
#49648=CARTESIAN_POINT('Ctrl Pts',(0.793516871680993,1.,-3.78959439439235));
#49649=CARTESIAN_POINT('Ctrl Pts',(0.793235612973273,1.,-3.79711921389897));
#49650=CARTESIAN_POINT('Ctrl Pts',(0.792882695234777,1.,-3.80459229925637));
#49651=CARTESIAN_POINT('Ctrl Pts',(0.792462483517634,1.,-3.81202588694756));
#49652=CARTESIAN_POINT('Ctrl Pts',(0.791981740718634,1.,-3.81944345442249));
#49653=CARTESIAN_POINT('Ctrl Pts',(0.791447528662369,1.,-3.82687033899792));
#49654=CARTESIAN_POINT('Ctrl Pts',(0.7908650127053,1.,-3.83432392054786));
#49655=CARTESIAN_POINT('Ctrl Pts',(0.790236124191242,1.,-3.84180762342454));
#49656=CARTESIAN_POINT('Ctrl Pts',(0.789560798155582,1.,-3.84931637808894));
#49657=CARTESIAN_POINT('Ctrl Pts',(0.788837734090671,1.,-3.85683995872529));
#49658=CARTESIAN_POINT('Ctrl Pts',(0.788065315093777,1.,-3.86436702561345));
#49659=CARTESIAN_POINT('Ctrl Pts',(0.787242527617999,1.,-3.87188916600912));
#49660=CARTESIAN_POINT('Ctrl Pts',(0.786369675812608,1.,-3.8794040281819));
#49661=CARTESIAN_POINT('Ctrl Pts',(0.78544789034073,1.,-3.88691313167398));
#49662=CARTESIAN_POINT('Ctrl Pts',(0.784478799358336,1.,-3.89442039235103));
#49663=CARTESIAN_POINT('Ctrl Pts',(0.783464141529081,1.,-3.9019303904397));
#49664=CARTESIAN_POINT('Ctrl Pts',(0.782405395622764,1.,-3.90944671004542));
#49665=CARTESIAN_POINT('Ctrl Pts',(0.781303428618366,1.,-3.91697036054676));
#49666=CARTESIAN_POINT('Ctrl Pts',(0.780158678615542,1.,-3.92450058323823));
#49667=CARTESIAN_POINT('Ctrl Pts',(0.77897130813482,1.,-3.93203552473174));
#49668=CARTESIAN_POINT('Ctrl Pts',(0.777741370568558,1.,-3.93957296768103));
#49669=CARTESIAN_POINT('Ctrl Pts',(0.776468966697921,1.,-3.94711101619447));
#49670=CARTESIAN_POINT('Ctrl Pts',(0.775154418039351,1.,-3.9546488545231));
#49671=CARTESIAN_POINT('Ctrl Pts',(0.773798212026565,1.,-3.96218649639807));
#49672=CARTESIAN_POINT('Ctrl Pts',(0.772400931772136,1.,-3.96972446532772));
#49673=CARTESIAN_POINT('Ctrl Pts',(0.77096319003047,1.,-3.97726349165488));
#49674=CARTESIAN_POINT('Ctrl Pts',(0.769485566245544,1.,-3.98480422348451));
#49675=CARTESIAN_POINT('Ctrl Pts',(0.767968531377914,1.,-3.9923468788101));
#49676=CARTESIAN_POINT('Ctrl Pts',(0.766412457136063,1.,-3.99989129179622));
#49677=CARTESIAN_POINT('Ctrl Pts',(0.764817648785197,1.,-4.00743706791509));
#49678=CARTESIAN_POINT('Ctrl Pts',(0.763184371182935,1.,-4.01498370680496));
#49679=CARTESIAN_POINT('Ctrl Pts',(0.761512875859804,1.,-4.02253072741268));
#49680=CARTESIAN_POINT('Ctrl Pts',(0.759803433243751,1.,-4.03007781954412));
#49681=CARTESIAN_POINT('Ctrl Pts',(0.758056338884944,1.,-4.03762485803119));
#49682=CARTESIAN_POINT('Ctrl Pts',(0.75627190236958,1.,-4.04517182653997));
#49683=CARTESIAN_POINT('Ctrl Pts',(0.754450441816078,1.,-4.05271876687915));
#49684=CARTESIAN_POINT('Ctrl Pts',(0.752592276483072,1.,-4.06026572221515));
#49685=CARTESIAN_POINT('Ctrl Pts',(0.750697720484036,1.,-4.06781267242378));
#49686=CARTESIAN_POINT('Ctrl Pts',(0.748767076680557,1.,-4.07535951056152));
#49687=CARTESIAN_POINT('Ctrl Pts',(0.746800631492315,1.,-4.08290608095642));
#49688=CARTESIAN_POINT('Ctrl Pts',(0.7447986497065,1.,-4.09045220253573));
#49689=CARTESIAN_POINT('Ctrl Pts',(0.742761369689841,1.,-4.09799769702611));
#49690=CARTESIAN_POINT('Ctrl Pts',(0.740688998553376,1.,-4.10554241757547));
#49691=CARTESIAN_POINT('Ctrl Pts',(0.738581708225843,1.,-4.11308626951927));
#49692=CARTESIAN_POINT('Ctrl Pts',(0.736439634331344,1.,-4.120629196238));
#49693=CARTESIAN_POINT('Ctrl Pts',(0.734698226764092,1.,-4.12666277570844));
#49694=CARTESIAN_POINT('Ctrl Pts',(0.733376589323546,1.,-4.13118752795207));
#49695=CARTESIAN_POINT('Ctrl Pts',(0.732488575135159,1.,-4.1342038373684));
#49696=CARTESIAN_POINT('Ctrl Pts',(0.73204283740062,1.,-4.13571194405636));
#49697=CARTESIAN_POINT('Origin',(0.73204283740062,0.,-4.13571194405636));
#49698=CARTESIAN_POINT('',(0.581791163835815,1.,-4.15950947128175));
#49699=CARTESIAN_POINT('Origin',(0.,0.,0.));
#49700=CARTESIAN_POINT('',(0.963899035117248,1.,-3.62400312501245));
#49701=CARTESIAN_POINT('Origin',(0.,1.,0.));
#49702=CARTESIAN_POINT('Ctrl Pts',(0.963899035117248,1.,-3.62400312501246));
#49703=CARTESIAN_POINT('Ctrl Pts',(0.963899035117248,0.666666666666667,
-3.62400312501246));
#49704=CARTESIAN_POINT('Ctrl Pts',(0.963899035117248,0.333333333333333,
-3.62400312501246));
#49705=CARTESIAN_POINT('Ctrl Pts',(0.963899035117248,-0.333333333333333,
-3.62400312501246));
#49706=CARTESIAN_POINT('Ctrl Pts',(0.963899035117249,-0.666666666666667,
-3.62400312501246));
#49707=CARTESIAN_POINT('Ctrl Pts',(0.963899035117249,-1.,-3.62400312501246));
#49708=CARTESIAN_POINT('Ctrl Pts',(1.22531898815164,-1.,-4.01728681790024));
#49709=CARTESIAN_POINT('Ctrl Pts',(1.22531898815164,1.,-4.01728681790024));
#49710=CARTESIAN_POINT('Ctrl Pts',(1.22423716681447,-1.,-4.0161454457032));
#49711=CARTESIAN_POINT('Ctrl Pts',(1.22423716681447,1.,-4.0161454457032));
#49712=CARTESIAN_POINT('Ctrl Pts',(1.22207656456199,-1.,-4.01386104434674));
#49713=CARTESIAN_POINT('Ctrl Pts',(1.22207656456199,1.,-4.01386104434674));
#49714=CARTESIAN_POINT('Ctrl Pts',(1.21884478244983,-1.,-4.01042947142681));
#49715=CARTESIAN_POINT('Ctrl Pts',(1.21884478244983,1.,-4.01042947142681));
#49716=CARTESIAN_POINT('Ctrl Pts',(1.21455398918813,-1.,-4.00584409524937));
#49717=CARTESIAN_POINT('Ctrl Pts',(1.21455398918813,1.,-4.00584409524937));
#49718=CARTESIAN_POINT('Ctrl Pts',(1.20922097030107,-1.,-4.00009577952534));
#49719=CARTESIAN_POINT('Ctrl Pts',(1.20922097030107,1.,-4.00009577952534));
#49720=CARTESIAN_POINT('Ctrl Pts',(1.2039185237544,-1.,-3.99433084800649));
#49721=CARTESIAN_POINT('Ctrl Pts',(1.2039185237544,1.,-3.99433084800649));
#49722=CARTESIAN_POINT('Ctrl Pts',(1.19864679609596,-1.,-3.98854928957287));
#49723=CARTESIAN_POINT('Ctrl Pts',(1.19864679609596,1.,-3.98854928957287));
#49724=CARTESIAN_POINT('Ctrl Pts',(1.19340598349307,-1.,-3.98275111052015));
#49725=CARTESIAN_POINT('Ctrl Pts',(1.19340598349307,1.,-3.98275111052015));
#49726=CARTESIAN_POINT('Ctrl Pts',(1.18819633715285,-1.,-3.97693634766926));
#49727=CARTESIAN_POINT('Ctrl Pts',(1.18819633715285,1.,-3.97693634766926));
#49728=CARTESIAN_POINT('Ctrl Pts',(1.18301815039596,-1.,-3.9711050516465));
#49729=CARTESIAN_POINT('Ctrl Pts',(1.18301815039596,1.,-3.9711050516465));
#49730=CARTESIAN_POINT('Ctrl Pts',(1.17787174135445,-1.,-3.96525726357682));
#49731=CARTESIAN_POINT('Ctrl Pts',(1.17787174135445,1.,-3.96525726357682));
#49732=CARTESIAN_POINT('Ctrl Pts',(1.17275743590327,-1.,-3.95939299213164));
#49733=CARTESIAN_POINT('Ctrl Pts',(1.17275743590327,1.,-3.95939299213164));
#49734=CARTESIAN_POINT('Ctrl Pts',(1.16767555244495,-1.,-3.95351219510062));
#49735=CARTESIAN_POINT('Ctrl Pts',(1.16767555244495,1.,-3.95351219510062));
#49736=CARTESIAN_POINT('Ctrl Pts',(1.16262637999261,-1.,-3.9476147478092));
#49737=CARTESIAN_POINT('Ctrl Pts',(1.16262637999261,1.,-3.9476147478092));
#49738=CARTESIAN_POINT('Ctrl Pts',(1.1576101834106,-1.,-3.94170046685542));
#49739=CARTESIAN_POINT('Ctrl Pts',(1.1576101834106,1.,-3.94170046685542));
#49740=CARTESIAN_POINT('Ctrl Pts',(1.1526272271639,-1.,-3.9357691705651));
#49741=CARTESIAN_POINT('Ctrl Pts',(1.1526272271639,1.,-3.9357691705651));
#49742=CARTESIAN_POINT('Ctrl Pts',(1.14767779451147,-1.,-3.92982073294334));
#49743=CARTESIAN_POINT('Ctrl Pts',(1.14767779451147,1.,-3.92982073294334));
#49744=CARTESIAN_POINT('Ctrl Pts',(1.14276220561575,-1.,-3.92385513133937));
#49745=CARTESIAN_POINT('Ctrl Pts',(1.14276220561575,1.,-3.92385513133937));
#49746=CARTESIAN_POINT('Ctrl Pts',(1.13788084225511,-1.,-3.91787251936688));
#49747=CARTESIAN_POINT('Ctrl Pts',(1.13788084225511,1.,-3.91787251936688));
#49748=CARTESIAN_POINT('Ctrl Pts',(1.13303414693849,-1.,-3.91187321145495));
#49749=CARTESIAN_POINT('Ctrl Pts',(1.13303414693849,1.,-3.91187321145495));
#49750=CARTESIAN_POINT('Ctrl Pts',(1.12822258281518,-1.,-3.90585753318622));
#49751=CARTESIAN_POINT('Ctrl Pts',(1.12822258281518,1.,-3.90585753318622));
#49752=CARTESIAN_POINT('Ctrl Pts',(1.12344660099029,-1.,-3.89982569749978));
#49753=CARTESIAN_POINT('Ctrl Pts',(1.12344660099029,1.,-3.89982569749978));
#49754=CARTESIAN_POINT('Ctrl Pts',(1.11870660794609,-1.,-3.89377768340362));
#49755=CARTESIAN_POINT('Ctrl Pts',(1.11870660794609,1.,-3.89377768340362));
#49756=CARTESIAN_POINT('Ctrl Pts',(1.11400292434447,-1.,-3.88771308285229));
#49757=CARTESIAN_POINT('Ctrl Pts',(1.11400292434447,1.,-3.88771308285229));
#49758=CARTESIAN_POINT('Ctrl Pts',(1.10933577224029,-1.,-3.88163105531791));
#49759=CARTESIAN_POINT('Ctrl Pts',(1.10933577224029,1.,-3.88163105531791));
#49760=CARTESIAN_POINT('Ctrl Pts',(1.10470536603303,-1.,-3.87553067187566));
#49761=CARTESIAN_POINT('Ctrl Pts',(1.10470536603303,1.,-3.87553067187566));
#49762=CARTESIAN_POINT('Ctrl Pts',(1.10011198761202,-1.,-3.86941120134872));
#49763=CARTESIAN_POINT('Ctrl Pts',(1.10011198761202,1.,-3.86941120134872));
#49764=CARTESIAN_POINT('Ctrl Pts',(1.09555606505012,-1.,-3.86327241021242));
#49765=CARTESIAN_POINT('Ctrl Pts',(1.09555606505012,1.,-3.86327241021242));
#49766=CARTESIAN_POINT('Ctrl Pts',(1.09103825516288,-1.,-3.85711487933911));
#49767=CARTESIAN_POINT('Ctrl Pts',(1.09103825516288,1.,-3.85711487933911));
#49768=CARTESIAN_POINT('Ctrl Pts',(1.08655950846377,-1.,-3.85094025222691));
#49769=CARTESIAN_POINT('Ctrl Pts',(1.08655950846377,1.,-3.85094025222691));
#49770=CARTESIAN_POINT('Ctrl Pts',(1.08212087917986,-1.,-3.84475048030615));
#49771=CARTESIAN_POINT('Ctrl Pts',(1.08212087917986,1.,-3.84475048030615));
#49772=CARTESIAN_POINT('Ctrl Pts',(1.07772335353856,-1.,-3.83854714117486));
#49773=CARTESIAN_POINT('Ctrl Pts',(1.07772335353856,1.,-3.83854714117486));
#49774=CARTESIAN_POINT('Ctrl Pts',(1.0733676663346,-1.,-3.83233071195145));
#49775=CARTESIAN_POINT('Ctrl Pts',(1.0733676663346,1.,-3.83233071195145));
#49776=CARTESIAN_POINT('Ctrl Pts',(1.0690541318036,-1.,-3.82609989967278));
#49777=CARTESIAN_POINT('Ctrl Pts',(1.0690541318036,1.,-3.82609989967278));
#49778=CARTESIAN_POINT('Ctrl Pts',(1.06478244038931,-1.,-3.81985083953012));
#49779=CARTESIAN_POINT('Ctrl Pts',(1.06478244038931,1.,-3.81985083953012));
#49780=CARTESIAN_POINT('Ctrl Pts',(1.06055206187298,-1.,-3.81357866117485));
#49781=CARTESIAN_POINT('Ctrl Pts',(1.06055206187298,1.,-3.81357866117485));
#49782=CARTESIAN_POINT('Ctrl Pts',(1.05636266918643,-1.,-3.80727913637784));
#49783=CARTESIAN_POINT('Ctrl Pts',(1.05636266918643,1.,-3.80727913637784));
#49784=CARTESIAN_POINT('Ctrl Pts',(1.05221457990015,-1.,-3.80095039790678));
#49785=CARTESIAN_POINT('Ctrl Pts',(1.05221457990015,1.,-3.80095039790678));
#49786=CARTESIAN_POINT('Ctrl Pts',(1.04810913267641,-1.,-3.79459440308793));
#49787=CARTESIAN_POINT('Ctrl Pts',(1.04810913267641,1.,-3.79459440308793));
#49788=CARTESIAN_POINT('Ctrl Pts',(1.04404924374426,-1.,-3.78821910787195));
#49789=CARTESIAN_POINT('Ctrl Pts',(1.04404924374426,1.,-3.78821910787195));
#49790=CARTESIAN_POINT('Ctrl Pts',(1.04003862055804,-1.,-3.78183535008192));
#49791=CARTESIAN_POINT('Ctrl Pts',(1.04003862055804,1.,-3.78183535008192));
#49792=CARTESIAN_POINT('Ctrl Pts',(1.03608074678013,-1.,-3.77545283140445));
#49793=CARTESIAN_POINT('Ctrl Pts',(1.03608074678013,1.,-3.77545283140445));
#49794=CARTESIAN_POINT('Ctrl Pts',(1.0321778660492,-1.,-3.76907609832522));
#49795=CARTESIAN_POINT('Ctrl Pts',(1.0321778660492,1.,-3.76907609832522));
#49796=CARTESIAN_POINT('Ctrl Pts',(1.02833014458181,-1.,-3.76270122291232));
#49797=CARTESIAN_POINT('Ctrl Pts',(1.02833014458181,1.,-3.76270122291232));
#49798=CARTESIAN_POINT('Ctrl Pts',(1.0245342944466,-1.,-3.75631037456194));
#49799=CARTESIAN_POINT('Ctrl Pts',(1.0245342944466,1.,-3.75631037456194));
#49800=CARTESIAN_POINT('Ctrl Pts',(1.02078510487428,-1.,-3.74987777155834));
#49801=CARTESIAN_POINT('Ctrl Pts',(1.02078510487428,1.,-3.74987777155834));
#49802=CARTESIAN_POINT('Ctrl Pts',(1.01707794311079,-1.,-3.74337942504959));
#49803=CARTESIAN_POINT('Ctrl Pts',(1.01707794311079,1.,-3.74337942504959));
#49804=CARTESIAN_POINT('Ctrl Pts',(1.01341114319903,-1.,-3.73680245055734));
#49805=CARTESIAN_POINT('Ctrl Pts',(1.01341114319903,1.,-3.73680245055734));
#49806=CARTESIAN_POINT('Ctrl Pts',(1.00978798539496,-1.,-3.73015276704426));
#49807=CARTESIAN_POINT('Ctrl Pts',(1.00978798539496,1.,-3.73015276704426));
#49808=CARTESIAN_POINT('Ctrl Pts',(1.0062200073571,-1.,-3.72346803750596));
#49809=CARTESIAN_POINT('Ctrl Pts',(1.0062200073571,1.,-3.72346803750596));
#49810=CARTESIAN_POINT('Ctrl Pts',(1.00272423396822,-1.,-3.71680667125119));
#49811=CARTESIAN_POINT('Ctrl Pts',(1.00272423396822,1.,-3.71680667125119));
#49812=CARTESIAN_POINT('Ctrl Pts',(0.99931726075653,-1.,-3.71022439713938));
#49813=CARTESIAN_POINT('Ctrl Pts',(0.99931726075653,1.,-3.71022439713938));
#49814=CARTESIAN_POINT('Ctrl Pts',(0.996009819772518,-1.,-3.70375282282138));
#49815=CARTESIAN_POINT('Ctrl Pts',(0.996009819772518,1.,-3.70375282282138));
#49816=CARTESIAN_POINT('Ctrl Pts',(0.99280221833201,-1.,-3.69738123415662));
#49817=CARTESIAN_POINT('Ctrl Pts',(0.99280221833201,1.,-3.69738123415662));
#49818=CARTESIAN_POINT('Ctrl Pts',(0.989676715398558,-1.,-3.69102682138847));
#49819=CARTESIAN_POINT('Ctrl Pts',(0.989676715398558,1.,-3.69102682138847));
#49820=CARTESIAN_POINT('Ctrl Pts',(0.986602639863837,-1.,-3.68455317926068));
#49821=CARTESIAN_POINT('Ctrl Pts',(0.986602639863837,1.,-3.68455317926068));
#49822=CARTESIAN_POINT('Ctrl Pts',(0.983550791470419,-1.,-3.67782408841715));
#49823=CARTESIAN_POINT('Ctrl Pts',(0.983550791470419,1.,-3.67782408841715));
#49824=CARTESIAN_POINT('Ctrl Pts',(0.980505922458267,-1.,-3.67074983340361));
#49825=CARTESIAN_POINT('Ctrl Pts',(0.980505922458267,1.,-3.67074983340361));
#49826=CARTESIAN_POINT('Ctrl Pts',(0.977478312751618,-1.,-3.66333049637475));
#49827=CARTESIAN_POINT('Ctrl Pts',(0.977478312751618,1.,-3.66333049637475));
#49828=CARTESIAN_POINT('Ctrl Pts',(0.974519971354848,-1.,-3.65571576735126));
#49829=CARTESIAN_POINT('Ctrl Pts',(0.974519971354848,1.,-3.65571576735126));
#49830=CARTESIAN_POINT('Ctrl Pts',(0.971722122061341,-1.,-3.64819756447455));
#49831=CARTESIAN_POINT('Ctrl Pts',(0.971722122061341,1.,-3.64819756447455));
#49832=CARTESIAN_POINT('Ctrl Pts',(0.969195124675865,-1.,-3.64113946505766));
#49833=CARTESIAN_POINT('Ctrl Pts',(0.969195124675865,1.,-3.64113946505766));
#49834=CARTESIAN_POINT('Ctrl Pts',(0.967052554541385,-1.,-3.63492122081143));
#49835=CARTESIAN_POINT('Ctrl Pts',(0.967052554541385,1.,-3.63492122081143));
#49836=CARTESIAN_POINT('Ctrl Pts',(0.965395153165293,-1.,-3.62988252139846));
#49837=CARTESIAN_POINT('Ctrl Pts',(0.965395153165293,1.,-3.62988252139846));
#49838=CARTESIAN_POINT('Ctrl Pts',(0.964291001273287,-1.,-3.62625391254797));
#49839=CARTESIAN_POINT('Ctrl Pts',(0.964291001273287,1.,-3.62625391254797));
#49840=CARTESIAN_POINT('Ctrl Pts',(0.963875774530619,-1.,-3.6245656860652));
#49841=CARTESIAN_POINT('Ctrl Pts',(0.963875774530619,1.,-3.6245656860652));
#49842=CARTESIAN_POINT('Ctrl Pts',(0.963832486395051,-1.,-3.62399933639915));
#49843=CARTESIAN_POINT('Ctrl Pts',(0.963832486395051,1.,-3.62399933639915));
#49844=CARTESIAN_POINT('Ctrl Pts',(0.963922720982193,-1.,-3.62393257642052));
#49845=CARTESIAN_POINT('Ctrl Pts',(0.963922720982193,1.,-3.62393257642052));
#49846=CARTESIAN_POINT('Ctrl Pts',(0.963997613369571,-1.,-3.62397690409552));
#49847=CARTESIAN_POINT('Ctrl Pts',(0.963997613369571,1.,-3.62397690409552));
#49848=CARTESIAN_POINT('',(1.22531898815164,1.,-4.01728681790024));
#49849=CARTESIAN_POINT('Ctrl Pts',(1.22531898815164,1.,-4.01728681790024));
#49850=CARTESIAN_POINT('Ctrl Pts',(1.22423716681447,1.,-4.0161454457032));
#49851=CARTESIAN_POINT('Ctrl Pts',(1.22207656456199,1.,-4.01386104434674));
#49852=CARTESIAN_POINT('Ctrl Pts',(1.21884478244983,1.,-4.01042947142681));
#49853=CARTESIAN_POINT('Ctrl Pts',(1.21455398918813,1.,-4.00584409524937));
#49854=CARTESIAN_POINT('Ctrl Pts',(1.20922097030107,1.,-4.00009577952534));
#49855=CARTESIAN_POINT('Ctrl Pts',(1.2039185237544,1.,-3.99433084800649));
#49856=CARTESIAN_POINT('Ctrl Pts',(1.19864679609596,1.,-3.98854928957287));
#49857=CARTESIAN_POINT('Ctrl Pts',(1.19340598349307,1.,-3.98275111052015));
#49858=CARTESIAN_POINT('Ctrl Pts',(1.18819633715285,1.,-3.97693634766926));
#49859=CARTESIAN_POINT('Ctrl Pts',(1.18301815039596,1.,-3.9711050516465));
#49860=CARTESIAN_POINT('Ctrl Pts',(1.17787174135445,1.,-3.96525726357682));
#49861=CARTESIAN_POINT('Ctrl Pts',(1.17275743590327,1.,-3.95939299213164));
#49862=CARTESIAN_POINT('Ctrl Pts',(1.16767555244495,1.,-3.95351219510062));
#49863=CARTESIAN_POINT('Ctrl Pts',(1.16262637999261,1.,-3.9476147478092));
#49864=CARTESIAN_POINT('Ctrl Pts',(1.1576101834106,1.,-3.94170046685542));
#49865=CARTESIAN_POINT('Ctrl Pts',(1.1526272271639,1.,-3.9357691705651));
#49866=CARTESIAN_POINT('Ctrl Pts',(1.14767779451147,1.,-3.92982073294334));
#49867=CARTESIAN_POINT('Ctrl Pts',(1.14276220561575,1.,-3.92385513133937));
#49868=CARTESIAN_POINT('Ctrl Pts',(1.13788084225511,1.,-3.91787251936688));
#49869=CARTESIAN_POINT('Ctrl Pts',(1.13303414693849,1.,-3.91187321145495));
#49870=CARTESIAN_POINT('Ctrl Pts',(1.12822258281518,1.,-3.90585753318622));
#49871=CARTESIAN_POINT('Ctrl Pts',(1.12344660099029,1.,-3.89982569749978));
#49872=CARTESIAN_POINT('Ctrl Pts',(1.11870660794609,1.,-3.89377768340362));
#49873=CARTESIAN_POINT('Ctrl Pts',(1.11400292434447,1.,-3.88771308285229));
#49874=CARTESIAN_POINT('Ctrl Pts',(1.10933577224029,1.,-3.88163105531791));
#49875=CARTESIAN_POINT('Ctrl Pts',(1.10470536603303,1.,-3.87553067187566));
#49876=CARTESIAN_POINT('Ctrl Pts',(1.10011198761202,1.,-3.86941120134872));
#49877=CARTESIAN_POINT('Ctrl Pts',(1.09555606505012,1.,-3.86327241021242));
#49878=CARTESIAN_POINT('Ctrl Pts',(1.09103825516288,1.,-3.85711487933911));
#49879=CARTESIAN_POINT('Ctrl Pts',(1.08655950846377,1.,-3.85094025222691));
#49880=CARTESIAN_POINT('Ctrl Pts',(1.08212087917986,1.,-3.84475048030615));
#49881=CARTESIAN_POINT('Ctrl Pts',(1.07772335353856,1.,-3.83854714117486));
#49882=CARTESIAN_POINT('Ctrl Pts',(1.0733676663346,1.,-3.83233071195145));
#49883=CARTESIAN_POINT('Ctrl Pts',(1.0690541318036,1.,-3.82609989967278));
#49884=CARTESIAN_POINT('Ctrl Pts',(1.06478244038931,1.,-3.81985083953012));
#49885=CARTESIAN_POINT('Ctrl Pts',(1.06055206187298,1.,-3.81357866117485));
#49886=CARTESIAN_POINT('Ctrl Pts',(1.05636266918643,1.,-3.80727913637784));
#49887=CARTESIAN_POINT('Ctrl Pts',(1.05221457990015,1.,-3.80095039790678));
#49888=CARTESIAN_POINT('Ctrl Pts',(1.04810913267641,1.,-3.79459440308793));
#49889=CARTESIAN_POINT('Ctrl Pts',(1.04404924374426,1.,-3.78821910787195));
#49890=CARTESIAN_POINT('Ctrl Pts',(1.04003862055804,1.,-3.78183535008192));
#49891=CARTESIAN_POINT('Ctrl Pts',(1.03608074678013,1.,-3.77545283140445));
#49892=CARTESIAN_POINT('Ctrl Pts',(1.0321778660492,1.,-3.76907609832522));
#49893=CARTESIAN_POINT('Ctrl Pts',(1.02833014458181,1.,-3.76270122291232));
#49894=CARTESIAN_POINT('Ctrl Pts',(1.0245342944466,1.,-3.75631037456194));
#49895=CARTESIAN_POINT('Ctrl Pts',(1.02078510487428,1.,-3.74987777155834));
#49896=CARTESIAN_POINT('Ctrl Pts',(1.01707794311079,1.,-3.74337942504959));
#49897=CARTESIAN_POINT('Ctrl Pts',(1.01341114319903,1.,-3.73680245055734));
#49898=CARTESIAN_POINT('Ctrl Pts',(1.00978798539496,1.,-3.73015276704426));
#49899=CARTESIAN_POINT('Ctrl Pts',(1.0062200073571,1.,-3.72346803750596));
#49900=CARTESIAN_POINT('Ctrl Pts',(1.00272423396822,1.,-3.71680667125119));
#49901=CARTESIAN_POINT('Ctrl Pts',(0.99931726075653,1.,-3.71022439713938));
#49902=CARTESIAN_POINT('Ctrl Pts',(0.996009819772518,1.,-3.70375282282138));
#49903=CARTESIAN_POINT('Ctrl Pts',(0.99280221833201,1.,-3.69738123415662));
#49904=CARTESIAN_POINT('Ctrl Pts',(0.989676715398558,1.,-3.69102682138847));
#49905=CARTESIAN_POINT('Ctrl Pts',(0.986602639863837,1.,-3.68455317926068));
#49906=CARTESIAN_POINT('Ctrl Pts',(0.983550791470419,1.,-3.67782408841715));
#49907=CARTESIAN_POINT('Ctrl Pts',(0.980505922458267,1.,-3.67074983340361));
#49908=CARTESIAN_POINT('Ctrl Pts',(0.977478312751618,1.,-3.66333049637475));
#49909=CARTESIAN_POINT('Ctrl Pts',(0.974519971354848,1.,-3.65571576735126));
#49910=CARTESIAN_POINT('Ctrl Pts',(0.971722122061341,1.,-3.64819756447455));
#49911=CARTESIAN_POINT('Ctrl Pts',(0.969195124675865,1.,-3.64113946505766));
#49912=CARTESIAN_POINT('Ctrl Pts',(0.967052554541385,1.,-3.63492122081143));
#49913=CARTESIAN_POINT('Ctrl Pts',(0.965395153165293,1.,-3.62988252139846));
#49914=CARTESIAN_POINT('Ctrl Pts',(0.964373850166457,1.,-3.62652618145335));
#49915=CARTESIAN_POINT('Ctrl Pts',(0.963957782642843,1.,-3.62489305727662));
#49916=CARTESIAN_POINT('Ctrl Pts',(0.963861297423241,1.,-3.62424461507588));
#49917=CARTESIAN_POINT('Ctrl Pts',(0.963880158555582,1.,-3.6240482887845));
#49918=CARTESIAN_POINT('Ctrl Pts',(0.963899035117249,1.,-3.62400312501246));
#49919=CARTESIAN_POINT('',(1.22531898815164,0.,-4.01728681790024));
#49920=CARTESIAN_POINT('Ctrl Pts',(1.35022972712301,-1.,-3.49848248301936));
#49921=CARTESIAN_POINT('Ctrl Pts',(1.35022972712301,1.,-3.49848248301936));
#49922=CARTESIAN_POINT('Ctrl Pts',(1.35026426118402,-1.,-3.4984026005375));
#49923=CARTESIAN_POINT('Ctrl Pts',(1.35026426118402,1.,-3.4984026005375));
#49924=CARTESIAN_POINT('Ctrl Pts',(1.35037650303019,-1.,-3.49840357193736));
#49925=CARTESIAN_POINT('Ctrl Pts',(1.35037650303019,1.,-3.49840357193736));
#49926=CARTESIAN_POINT('Ctrl Pts',(1.35067437417483,-1.,-3.49888720257132));
#49927=CARTESIAN_POINT('Ctrl Pts',(1.35067437417483,1.,-3.49888720257132));
#49928=CARTESIAN_POINT('Ctrl Pts',(1.3513307633124,-1.,-3.5004970706414));
#49929=CARTESIAN_POINT('Ctrl Pts',(1.3513307633124,1.,-3.5004970706414));
#49930=CARTESIAN_POINT('Ctrl Pts',(1.35257032843486,-1.,-3.50408168106261));
#49931=CARTESIAN_POINT('Ctrl Pts',(1.35257032843486,1.,-3.50408168106261));
#49932=CARTESIAN_POINT('Ctrl Pts',(1.35419113575956,-1.,-3.50913227059999));
#49933=CARTESIAN_POINT('Ctrl Pts',(1.35419113575956,1.,-3.50913227059999));
#49934=CARTESIAN_POINT('Ctrl Pts',(1.35611275237152,-1.,-3.51542230699556));
#49935=CARTESIAN_POINT('Ctrl Pts',(1.35611275237152,1.,-3.51542230699556));
#49936=CARTESIAN_POINT('Ctrl Pts',(1.35821701528836,-1.,-3.52261776116748));
#49937=CARTESIAN_POINT('Ctrl Pts',(1.35821701528836,1.,-3.52261776116748));
#49938=CARTESIAN_POINT('Ctrl Pts',(1.36037259643734,-1.,-3.530344649616));
#49939=CARTESIAN_POINT('Ctrl Pts',(1.36037259643734,1.,-3.530344649616));
#49940=CARTESIAN_POINT('Ctrl Pts',(1.36245507339307,-1.,-3.53824396424961));
#49941=CARTESIAN_POINT('Ctrl Pts',(1.36245507339307,1.,-3.53824396424961));
#49942=CARTESIAN_POINT('Ctrl Pts',(1.36436666257597,-1.,-3.54602591832973));
#49943=CARTESIAN_POINT('Ctrl Pts',(1.36436666257597,1.,-3.54602591832973));
#49944=CARTESIAN_POINT('Ctrl Pts',(1.3660614545677,-1.,-3.55353883995949));
#49945=CARTESIAN_POINT('Ctrl Pts',(1.3660614545677,1.,-3.55353883995949));
#49946=CARTESIAN_POINT('Ctrl Pts',(1.36754771771233,-1.,-3.56077662028649));
#49947=CARTESIAN_POINT('Ctrl Pts',(1.36754771771233,1.,-3.56077662028649));
#49948=CARTESIAN_POINT('Ctrl Pts',(1.36886584973389,-1.,-3.5678208030466));
#49949=CARTESIAN_POINT('Ctrl Pts',(1.36886584973389,1.,-3.5678208030466));
#49950=CARTESIAN_POINT('Ctrl Pts',(1.37007229485659,-1.,-3.57479875549486));
#49951=CARTESIAN_POINT('Ctrl Pts',(1.37007229485659,1.,-3.57479875549486));
#49952=CARTESIAN_POINT('Ctrl Pts',(1.37122241663062,-1.,-3.58183885982715));
#49953=CARTESIAN_POINT('Ctrl Pts',(1.37122241663062,1.,-3.58183885982715));
#49954=CARTESIAN_POINT('Ctrl Pts',(1.37235053660976,-1.,-3.58901853846365));
#49955=CARTESIAN_POINT('Ctrl Pts',(1.37235053660976,1.,-3.58901853846365));
#49956=CARTESIAN_POINT('Ctrl Pts',(1.37346320103157,-1.,-3.59634627869048));
#49957=CARTESIAN_POINT('Ctrl Pts',(1.37346320103157,1.,-3.59634627869048));
#49958=CARTESIAN_POINT('Ctrl Pts',(1.37455051379623,-1.,-3.60379020123988));
#49959=CARTESIAN_POINT('Ctrl Pts',(1.37455051379623,1.,-3.60379020123988));
#49960=CARTESIAN_POINT('Ctrl Pts',(1.37559314436634,-1.,-3.61129546591064));
#49961=CARTESIAN_POINT('Ctrl Pts',(1.37559314436634,1.,-3.61129546591064));
#49962=CARTESIAN_POINT('Ctrl Pts',(1.37657053403107,-1.,-3.61880481160421));
#49963=CARTESIAN_POINT('Ctrl Pts',(1.37657053403107,1.,-3.61880481160421));
#49964=CARTESIAN_POINT('Ctrl Pts',(1.37746987919881,-1.,-3.62628098665145));
#49965=CARTESIAN_POINT('Ctrl Pts',(1.37746987919881,1.,-3.62628098665145));
#49966=CARTESIAN_POINT('Ctrl Pts',(1.37829035457339,-1.,-3.63371727442486));
#49967=CARTESIAN_POINT('Ctrl Pts',(1.37829035457339,1.,-3.63371727442486));
#49968=CARTESIAN_POINT('Ctrl Pts',(1.37903818567359,-1.,-3.64112507791141));
#49969=CARTESIAN_POINT('Ctrl Pts',(1.37903818567359,1.,-3.64112507791141));
#49970=CARTESIAN_POINT('Ctrl Pts',(1.37972372481603,-1.,-3.64852652756456));
#49971=CARTESIAN_POINT('Ctrl Pts',(1.37972372481603,1.,-3.64852652756456));
#49972=CARTESIAN_POINT('Ctrl Pts',(1.38035791051212,-1.,-3.6559455440439));
#49973=CARTESIAN_POINT('Ctrl Pts',(1.38035791051212,1.,-3.6559455440439));
#49974=CARTESIAN_POINT('Ctrl Pts',(1.38094856333552,-1.,-3.66339848520857));
#49975=CARTESIAN_POINT('Ctrl Pts',(1.38094856333552,1.,-3.66339848520857));
#49976=CARTESIAN_POINT('Ctrl Pts',(1.38149812653868,-1.,-3.67088843112262));
#49977=CARTESIAN_POINT('Ctrl Pts',(1.38149812653868,1.,-3.67088843112262));
#49978=CARTESIAN_POINT('Ctrl Pts',(1.3820057429062,-1.,-3.67841038482414));
#49979=CARTESIAN_POINT('Ctrl Pts',(1.3820057429062,1.,-3.67841038482414));
#49980=CARTESIAN_POINT('Ctrl Pts',(1.38246852827182,-1.,-3.68595444983838));
#49981=CARTESIAN_POINT('Ctrl Pts',(1.38246852827182,1.,-3.68595444983838));
#49982=CARTESIAN_POINT('Ctrl Pts',(1.3828831117165,-1.,-3.69350967899526));
#49983=CARTESIAN_POINT('Ctrl Pts',(1.3828831117165,1.,-3.69350967899526));
#49984=CARTESIAN_POINT('Ctrl Pts',(1.38324717612865,-1.,-3.701067921679));
#49985=CARTESIAN_POINT('Ctrl Pts',(1.38324717612865,1.,-3.701067921679));
#49986=CARTESIAN_POINT('Ctrl Pts',(1.38356065402124,-1.,-3.70862680753347));
#49987=CARTESIAN_POINT('Ctrl Pts',(1.38356065402124,1.,-3.70862680753347));
#49988=CARTESIAN_POINT('Ctrl Pts',(1.38382489984586,-1.,-3.7161876605181));
#49989=CARTESIAN_POINT('Ctrl Pts',(1.38382489984586,1.,-3.7161876605181));
#49990=CARTESIAN_POINT('Ctrl Pts',(1.3840421342895,-1.,-3.72375409358803));
#49991=CARTESIAN_POINT('Ctrl Pts',(1.3840421342895,1.,-3.72375409358803));
#49992=CARTESIAN_POINT('Ctrl Pts',(1.38421479111531,-1.,-3.73133035859282));
#49993=CARTESIAN_POINT('Ctrl Pts',(1.38421479111531,1.,-3.73133035859282));
#49994=CARTESIAN_POINT('Ctrl Pts',(1.38434489156458,-1.,-3.73891976418104));
#49995=CARTESIAN_POINT('Ctrl Pts',(1.38434489156458,1.,-3.73891976418104));
#49996=CARTESIAN_POINT('Ctrl Pts',(1.38443344984394,-1.,-3.74652317167876));
#49997=CARTESIAN_POINT('Ctrl Pts',(1.38443344984394,1.,-3.74652317167876));
#49998=CARTESIAN_POINT('Ctrl Pts',(1.38448077997163,-1.,-3.7541397631875));
#49999=CARTESIAN_POINT('Ctrl Pts',(1.38448077997163,1.,-3.7541397631875));
#50000=CARTESIAN_POINT('Ctrl Pts',(1.3844867525335,-1.,-3.76176768271367));
#50001=CARTESIAN_POINT('Ctrl Pts',(1.3844867525335,1.,-3.76176768271367));
#50002=CARTESIAN_POINT('Ctrl Pts',(1.38445107339518,-1.,-3.76940473185779));
#50003=CARTESIAN_POINT('Ctrl Pts',(1.38445107339518,1.,-3.76940473185779));
#50004=CARTESIAN_POINT('Ctrl Pts',(1.38437354551428,-1.,-3.77704902230418));
#50005=CARTESIAN_POINT('Ctrl Pts',(1.38437354551428,1.,-3.77704902230418));
#50006=CARTESIAN_POINT('Ctrl Pts',(1.38425435883756,-1.,-3.78469969805082));
#50007=CARTESIAN_POINT('Ctrl Pts',(1.38425435883756,1.,-3.78469969805082));
#50008=CARTESIAN_POINT('Ctrl Pts',(1.38409399694566,-1.,-3.79235669640841));
#50009=CARTESIAN_POINT('Ctrl Pts',(1.38409399694566,1.,-3.79235669640841));
#50010=CARTESIAN_POINT('Ctrl Pts',(1.38389311766682,-1.,-3.80002044322111));
#50011=CARTESIAN_POINT('Ctrl Pts',(1.38389311766682,1.,-3.80002044322111));
#50012=CARTESIAN_POINT('Ctrl Pts',(1.3836524404622,-1.,-3.80769156398411));
#50013=CARTESIAN_POINT('Ctrl Pts',(1.3836524404622,1.,-3.80769156398411));
#50014=CARTESIAN_POINT('Ctrl Pts',(1.38337263902782,-1.,-3.81537060817811));
#50015=CARTESIAN_POINT('Ctrl Pts',(1.38337263902782,1.,-3.81537060817811));
#50016=CARTESIAN_POINT('Ctrl Pts',(1.38305421262763,-1.,-3.82305771743829));
#50017=CARTESIAN_POINT('Ctrl Pts',(1.38305421262763,1.,-3.82305771743829));
#50018=CARTESIAN_POINT('Ctrl Pts',(1.38269750245138,-1.,-3.8307526698229));
#50019=CARTESIAN_POINT('Ctrl Pts',(1.38269750245138,1.,-3.8307526698229));
#50020=CARTESIAN_POINT('Ctrl Pts',(1.38230274828821,-1.,-3.83845502790746));
#50021=CARTESIAN_POINT('Ctrl Pts',(1.38230274828821,1.,-3.83845502790746));
#50022=CARTESIAN_POINT('Ctrl Pts',(1.38187013346109,-1.,-3.84616425605764));
#50023=CARTESIAN_POINT('Ctrl Pts',(1.38187013346109,1.,-3.84616425605764));
#50024=CARTESIAN_POINT('Ctrl Pts',(1.38139983115049,-1.,-3.85387983979481));
#50025=CARTESIAN_POINT('Ctrl Pts',(1.38139983115049,1.,-3.85387983979481));
#50026=CARTESIAN_POINT('Ctrl Pts',(1.38089205992989,-1.,-3.86160143043959));
#50027=CARTESIAN_POINT('Ctrl Pts',(1.38089205992989,1.,-3.86160143043959));
#50028=CARTESIAN_POINT('Ctrl Pts',(1.38034709213014,-1.,-3.86932885813068));
#50029=CARTESIAN_POINT('Ctrl Pts',(1.38034709213014,1.,-3.86932885813068));
#50030=CARTESIAN_POINT('Ctrl Pts',(1.37976523097073,-1.,-3.87706205830532));
#50031=CARTESIAN_POINT('Ctrl Pts',(1.37976523097073,1.,-3.87706205830532));
#50032=CARTESIAN_POINT('Ctrl Pts',(1.37914679719383,-1.,-3.88480102249278));
#50033=CARTESIAN_POINT('Ctrl Pts',(1.37914679719383,1.,-3.88480102249278));
#50034=CARTESIAN_POINT('Ctrl Pts',(1.3784921128802,-1.,-3.89254574338496));
#50035=CARTESIAN_POINT('Ctrl Pts',(1.3784921128802,1.,-3.89254574338496));
#50036=CARTESIAN_POINT('Ctrl Pts',(1.37780148512792,-1.,-3.90029615196727));
#50037=CARTESIAN_POINT('Ctrl Pts',(1.37780148512792,1.,-3.90029615196727));
#50038=CARTESIAN_POINT('Ctrl Pts',(1.3770751963402,-1.,-3.90805209523486));
#50039=CARTESIAN_POINT('Ctrl Pts',(1.3770751963402,1.,-3.90805209523486));
#50040=CARTESIAN_POINT('Ctrl Pts',(1.37631350505797,-1.,-3.91581337462644));
#50041=CARTESIAN_POINT('Ctrl Pts',(1.37631350505797,1.,-3.91581337462644));
#50042=CARTESIAN_POINT('Ctrl Pts',(1.37551664448242,-1.,-3.92357976987672));
#50043=CARTESIAN_POINT('Ctrl Pts',(1.37551664448242,1.,-3.92357976987672));
#50044=CARTESIAN_POINT('Ctrl Pts',(1.37468482215751,-1.,-3.93135106761844));
#50045=CARTESIAN_POINT('Ctrl Pts',(1.37468482215751,1.,-3.93135106761844));
#50046=CARTESIAN_POINT('Ctrl Pts',(1.37381821967165,-1.,-3.93912709040818));
#50047=CARTESIAN_POINT('Ctrl Pts',(1.37381821967165,1.,-3.93912709040818));
#50048=CARTESIAN_POINT('Ctrl Pts',(1.37291699202807,-1.,-3.94690771785133));
#50049=CARTESIAN_POINT('Ctrl Pts',(1.37291699202807,1.,-3.94690771785133));
#50050=CARTESIAN_POINT('Ctrl Pts',(1.37198126432386,-1.,-3.95469287280914));
#50051=CARTESIAN_POINT('Ctrl Pts',(1.37198126432386,1.,-3.95469287280914));
#50052=CARTESIAN_POINT('Ctrl Pts',(1.3712051561502,-1.,-3.96092458506535));
#50053=CARTESIAN_POINT('Ctrl Pts',(1.3712051561502,1.,-3.96092458506535));
#50054=CARTESIAN_POINT('Ctrl Pts',(1.37060761745635,-1.,-3.96560037974645));
#50055=CARTESIAN_POINT('Ctrl Pts',(1.37060761745635,1.,-3.96560037974645));
#50056=CARTESIAN_POINT('Ctrl Pts',(1.37020239094614,-1.,-3.9687184694131));
#50057=CARTESIAN_POINT('Ctrl Pts',(1.37020239094614,1.,-3.9687184694131));
#50058=CARTESIAN_POINT('Ctrl Pts',(1.36999806084572,-1.,-3.97027773754922));
#50059=CARTESIAN_POINT('Ctrl Pts',(1.36999806084572,1.,-3.97027773754922));
#50060=CARTESIAN_POINT('',(1.35032489087101,1.,-3.4984457533445));
#50061=CARTESIAN_POINT('Ctrl Pts',(1.35032489087101,-1.,-3.4984457533445));
#50062=CARTESIAN_POINT('Ctrl Pts',(1.35032489087101,-0.666666666666667,
-3.4984457533445));
#50063=CARTESIAN_POINT('Ctrl Pts',(1.35032489087101,-0.333333333333333,
-3.4984457533445));
#50064=CARTESIAN_POINT('Ctrl Pts',(1.35032489087101,0.333333333333333,-3.4984457533445));
#50065=CARTESIAN_POINT('Ctrl Pts',(1.35032489087101,0.666666666666667,-3.4984457533445));
#50066=CARTESIAN_POINT('Ctrl Pts',(1.35032489087101,1.,-3.4984457533445));
#50067=CARTESIAN_POINT('',(1.36999806084572,1.,-3.97027773754922));
#50068=CARTESIAN_POINT('',(1.36999806084572,0.,-3.97027773754922));
#50069=CARTESIAN_POINT('Ctrl Pts',(1.35032489087101,1.,-3.49844575334451));
#50070=CARTESIAN_POINT('Ctrl Pts',(1.35036670892966,1.,-3.49847119623846));
#50071=CARTESIAN_POINT('Ctrl Pts',(1.35049736560527,1.,-3.49861894124827));
#50072=CARTESIAN_POINT('Ctrl Pts',(1.35080045218587,1.,-3.49920025459723));
#50073=CARTESIAN_POINT('Ctrl Pts',(1.35142377279517,1.,-3.50076603816491));
#50074=CARTESIAN_POINT('Ctrl Pts',(1.35257032843486,1.,-3.50408168106261));
#50075=CARTESIAN_POINT('Ctrl Pts',(1.35419113575956,1.,-3.50913227059999));
#50076=CARTESIAN_POINT('Ctrl Pts',(1.35611275237152,1.,-3.51542230699556));
#50077=CARTESIAN_POINT('Ctrl Pts',(1.35821701528836,1.,-3.52261776116748));
#50078=CARTESIAN_POINT('Ctrl Pts',(1.36037259643734,1.,-3.530344649616));
#50079=CARTESIAN_POINT('Ctrl Pts',(1.36245507339307,1.,-3.53824396424961));
#50080=CARTESIAN_POINT('Ctrl Pts',(1.36436666257597,1.,-3.54602591832973));
#50081=CARTESIAN_POINT('Ctrl Pts',(1.3660614545677,1.,-3.55353883995949));
#50082=CARTESIAN_POINT('Ctrl Pts',(1.36754771771233,1.,-3.56077662028649));
#50083=CARTESIAN_POINT('Ctrl Pts',(1.36886584973389,1.,-3.5678208030466));
#50084=CARTESIAN_POINT('Ctrl Pts',(1.37007229485659,1.,-3.57479875549486));
#50085=CARTESIAN_POINT('Ctrl Pts',(1.37122241663062,1.,-3.58183885982715));
#50086=CARTESIAN_POINT('Ctrl Pts',(1.37235053660976,1.,-3.58901853846365));
#50087=CARTESIAN_POINT('Ctrl Pts',(1.37346320103157,1.,-3.59634627869048));
#50088=CARTESIAN_POINT('Ctrl Pts',(1.37455051379623,1.,-3.60379020123988));
#50089=CARTESIAN_POINT('Ctrl Pts',(1.37559314436634,1.,-3.61129546591064));
#50090=CARTESIAN_POINT('Ctrl Pts',(1.37657053403107,1.,-3.61880481160421));
#50091=CARTESIAN_POINT('Ctrl Pts',(1.37746987919881,1.,-3.62628098665145));
#50092=CARTESIAN_POINT('Ctrl Pts',(1.37829035457339,1.,-3.63371727442486));
#50093=CARTESIAN_POINT('Ctrl Pts',(1.37903818567359,1.,-3.64112507791141));
#50094=CARTESIAN_POINT('Ctrl Pts',(1.37972372481603,1.,-3.64852652756456));
#50095=CARTESIAN_POINT('Ctrl Pts',(1.38035791051212,1.,-3.6559455440439));
#50096=CARTESIAN_POINT('Ctrl Pts',(1.38094856333552,1.,-3.66339848520857));
#50097=CARTESIAN_POINT('Ctrl Pts',(1.38149812653868,1.,-3.67088843112262));
#50098=CARTESIAN_POINT('Ctrl Pts',(1.3820057429062,1.,-3.67841038482414));
#50099=CARTESIAN_POINT('Ctrl Pts',(1.38246852827182,1.,-3.68595444983838));
#50100=CARTESIAN_POINT('Ctrl Pts',(1.3828831117165,1.,-3.69350967899526));
#50101=CARTESIAN_POINT('Ctrl Pts',(1.38324717612865,1.,-3.701067921679));
#50102=CARTESIAN_POINT('Ctrl Pts',(1.38356065402124,1.,-3.70862680753347));
#50103=CARTESIAN_POINT('Ctrl Pts',(1.38382489984586,1.,-3.7161876605181));
#50104=CARTESIAN_POINT('Ctrl Pts',(1.3840421342895,1.,-3.72375409358803));
#50105=CARTESIAN_POINT('Ctrl Pts',(1.38421479111531,1.,-3.73133035859282));
#50106=CARTESIAN_POINT('Ctrl Pts',(1.38434489156458,1.,-3.73891976418104));
#50107=CARTESIAN_POINT('Ctrl Pts',(1.38443344984394,1.,-3.74652317167876));
#50108=CARTESIAN_POINT('Ctrl Pts',(1.38448077997163,1.,-3.7541397631875));
#50109=CARTESIAN_POINT('Ctrl Pts',(1.3844867525335,1.,-3.76176768271367));
#50110=CARTESIAN_POINT('Ctrl Pts',(1.38445107339518,1.,-3.76940473185779));
#50111=CARTESIAN_POINT('Ctrl Pts',(1.38437354551428,1.,-3.77704902230418));
#50112=CARTESIAN_POINT('Ctrl Pts',(1.38425435883756,1.,-3.78469969805082));
#50113=CARTESIAN_POINT('Ctrl Pts',(1.38409399694566,1.,-3.79235669640841));
#50114=CARTESIAN_POINT('Ctrl Pts',(1.38389311766682,1.,-3.80002044322111));
#50115=CARTESIAN_POINT('Ctrl Pts',(1.3836524404622,1.,-3.80769156398411));
#50116=CARTESIAN_POINT('Ctrl Pts',(1.38337263902782,1.,-3.81537060817811));
#50117=CARTESIAN_POINT('Ctrl Pts',(1.38305421262763,1.,-3.82305771743829));
#50118=CARTESIAN_POINT('Ctrl Pts',(1.38269750245138,1.,-3.8307526698229));
#50119=CARTESIAN_POINT('Ctrl Pts',(1.38230274828821,1.,-3.83845502790746));
#50120=CARTESIAN_POINT('Ctrl Pts',(1.38187013346109,1.,-3.84616425605764));
#50121=CARTESIAN_POINT('Ctrl Pts',(1.38139983115049,1.,-3.85387983979481));
#50122=CARTESIAN_POINT('Ctrl Pts',(1.38089205992989,1.,-3.86160143043959));
#50123=CARTESIAN_POINT('Ctrl Pts',(1.38034709213014,1.,-3.86932885813068));
#50124=CARTESIAN_POINT('Ctrl Pts',(1.37976523097073,1.,-3.87706205830532));
#50125=CARTESIAN_POINT('Ctrl Pts',(1.37914679719383,1.,-3.88480102249278));
#50126=CARTESIAN_POINT('Ctrl Pts',(1.3784921128802,1.,-3.89254574338496));
#50127=CARTESIAN_POINT('Ctrl Pts',(1.37780148512792,1.,-3.90029615196727));
#50128=CARTESIAN_POINT('Ctrl Pts',(1.3770751963402,1.,-3.90805209523486));
#50129=CARTESIAN_POINT('Ctrl Pts',(1.37631350505797,1.,-3.91581337462644));
#50130=CARTESIAN_POINT('Ctrl Pts',(1.37551664448242,1.,-3.92357976987672));
#50131=CARTESIAN_POINT('Ctrl Pts',(1.37468482215751,1.,-3.93135106761844));
#50132=CARTESIAN_POINT('Ctrl Pts',(1.37381821967165,1.,-3.93912709040818));
#50133=CARTESIAN_POINT('Ctrl Pts',(1.37291699202807,1.,-3.94690771785133));
#50134=CARTESIAN_POINT('Ctrl Pts',(1.37198126432386,1.,-3.95469287280914));
#50135=CARTESIAN_POINT('Ctrl Pts',(1.3712051561502,1.,-3.96092458506535));
#50136=CARTESIAN_POINT('Ctrl Pts',(1.37060761745635,1.,-3.96560037974645));
#50137=CARTESIAN_POINT('Ctrl Pts',(1.37020239094614,1.,-3.9687184694131));
#50138=CARTESIAN_POINT('Ctrl Pts',(1.36999806084572,1.,-3.97027773754922));
#50139=CARTESIAN_POINT('Origin',(1.36999806084572,0.,-3.97027773754922));
#50140=CARTESIAN_POINT('',(1.22531898815164,1.,-4.01728681790024));
#50141=CARTESIAN_POINT('Origin',(0.,0.,0.));
#50142=CARTESIAN_POINT('',(1.51895082866166,1.,-3.42859860294378));
#50143=CARTESIAN_POINT('Origin',(0.,1.,0.));
#50144=CARTESIAN_POINT('Ctrl Pts',(1.51895082866166,1.,-3.42859860294378));
#50145=CARTESIAN_POINT('Ctrl Pts',(1.51895082866166,0.666666666666667,-3.42859860294378));
#50146=CARTESIAN_POINT('Ctrl Pts',(1.51895082866166,0.333333333333333,-3.42859860294378));
#50147=CARTESIAN_POINT('Ctrl Pts',(1.51895082866166,-0.333333333333333,
-3.42859860294378));
#50148=CARTESIAN_POINT('Ctrl Pts',(1.51895082866166,-0.666666666666667,
-3.42859860294378));
#50149=CARTESIAN_POINT('Ctrl Pts',(1.51895082866166,-1.,-3.42859860294378));
#50150=CARTESIAN_POINT('Ctrl Pts',(1.83867539237861,-1.,-3.77614523045147));
#50151=CARTESIAN_POINT('Ctrl Pts',(1.83867539237861,1.,-3.77614523045147));
#50152=CARTESIAN_POINT('Ctrl Pts',(1.83742834010821,-1.,-3.77518714458232));
#50153=CARTESIAN_POINT('Ctrl Pts',(1.83742834010821,1.,-3.77518714458232));
#50154=CARTESIAN_POINT('Ctrl Pts',(1.83493697935064,-1.,-3.77326886065484));
#50155=CARTESIAN_POINT('Ctrl Pts',(1.83493697935064,1.,-3.77326886065484));
#50156=CARTESIAN_POINT('Ctrl Pts',(1.83120816956515,-1.,-3.77038509819777));
#50157=CARTESIAN_POINT('Ctrl Pts',(1.83120816956515,1.,-3.77038509819777));
#50158=CARTESIAN_POINT('Ctrl Pts',(1.82625289221933,-1.,-3.76652740355856));
#50159=CARTESIAN_POINT('Ctrl Pts',(1.82625289221933,1.,-3.76652740355856));
#50160=CARTESIAN_POINT('Ctrl Pts',(1.82008629694924,-1.,-3.76168412709652));
#50161=CARTESIAN_POINT('Ctrl Pts',(1.82008629694924,1.,-3.76168412709652));
#50162=CARTESIAN_POINT('Ctrl Pts',(1.81394729834032,-1.,-3.75681965683995));
#50163=CARTESIAN_POINT('Ctrl Pts',(1.81394729834032,1.,-3.75681965683995));
#50164=CARTESIAN_POINT('Ctrl Pts',(1.80783603939662,-1.,-3.75193395888069));
#50165=CARTESIAN_POINT('Ctrl Pts',(1.80783603939662,1.,-3.75193395888069));
#50166=CARTESIAN_POINT('Ctrl Pts',(1.80175271485519,-1.,-3.74702700874954));
#50167=CARTESIAN_POINT('Ctrl Pts',(1.80175271485519,1.,-3.74702700874954));
#50168=CARTESIAN_POINT('Ctrl Pts',(1.79569757859041,-1.,-3.74209880351667));
#50169=CARTESIAN_POINT('Ctrl Pts',(1.79569757859041,1.,-3.74209880351667));
#50170=CARTESIAN_POINT('Ctrl Pts',(1.78967092823139,-1.,-3.73714934729962));
#50171=CARTESIAN_POINT('Ctrl Pts',(1.78967092823139,1.,-3.73714934729962));
#50172=CARTESIAN_POINT('Ctrl Pts',(1.78367308442682,-1.,-3.73217863095022));
#50173=CARTESIAN_POINT('Ctrl Pts',(1.78367308442682,1.,-3.73217863095022));
#50174=CARTESIAN_POINT('Ctrl Pts',(1.77770437039606,-1.,-3.72718661205504));
#50175=CARTESIAN_POINT('Ctrl Pts',(1.77770437039606,1.,-3.72718661205504));
#50176=CARTESIAN_POINT('Ctrl Pts',(1.77176509401846,-1.,-3.72217319911429));
#50177=CARTESIAN_POINT('Ctrl Pts',(1.77176509401846,1.,-3.72217319911429));
#50178=CARTESIAN_POINT('Ctrl Pts',(1.76585552124549,-1.,-3.71713822377676));
#50179=CARTESIAN_POINT('Ctrl Pts',(1.76585552124549,1.,-3.71713822377676));
#50180=CARTESIAN_POINT('Ctrl Pts',(1.75997588499021,-1.,-3.71208146346455));
#50181=CARTESIAN_POINT('Ctrl Pts',(1.75997588499021,1.,-3.71208146346455));
#50182=CARTESIAN_POINT('Ctrl Pts',(1.75412641804148,-1.,-3.70700269736876));
#50183=CARTESIAN_POINT('Ctrl Pts',(1.75412641804148,1.,-3.70700269736876));
#50184=CARTESIAN_POINT('Ctrl Pts',(1.74830738046092,-1.,-3.70190175673422));
#50185=CARTESIAN_POINT('Ctrl Pts',(1.74830738046092,1.,-3.70190175673422));
#50186=CARTESIAN_POINT('Ctrl Pts',(1.74251908492589,-1.,-3.6967785691046));
#50187=CARTESIAN_POINT('Ctrl Pts',(1.74251908492589,1.,-3.6967785691046));
#50188=CARTESIAN_POINT('Ctrl Pts',(1.73676193254493,-1.,-3.69163322647906));
#50189=CARTESIAN_POINT('Ctrl Pts',(1.73676193254493,1.,-3.69163322647906));
#50190=CARTESIAN_POINT('Ctrl Pts',(1.73103640956647,-1.,-3.68646597019188));
#50191=CARTESIAN_POINT('Ctrl Pts',(1.73103640956647,1.,-3.68646597019188));
#50192=CARTESIAN_POINT('Ctrl Pts',(1.72534302437003,-1.,-3.68127704936472));
#50193=CARTESIAN_POINT('Ctrl Pts',(1.72534302437003,1.,-3.68127704936472));
#50194=CARTESIAN_POINT('Ctrl Pts',(1.71968225581787,-1.,-3.67606660374665));
#50195=CARTESIAN_POINT('Ctrl Pts',(1.71968225581787,1.,-3.67606660374665));
#50196=CARTESIAN_POINT('Ctrl Pts',(1.71405450210392,-1.,-3.67083454901629));
#50197=CARTESIAN_POINT('Ctrl Pts',(1.71405450210392,1.,-3.67083454901629));
#50198=CARTESIAN_POINT('Ctrl Pts',(1.70846001610983,-1.,-3.6655804319893));
#50199=CARTESIAN_POINT('Ctrl Pts',(1.70846001610983,1.,-3.6655804319893));
#50200=CARTESIAN_POINT('Ctrl Pts',(1.70289888566904,-1.,-3.6603033877491));
#50201=CARTESIAN_POINT('Ctrl Pts',(1.70289888566904,1.,-3.6603033877491));
#50202=CARTESIAN_POINT('Ctrl Pts',(1.69737117722558,-1.,-3.65500246526798));
#50203=CARTESIAN_POINT('Ctrl Pts',(1.69737117722558,1.,-3.65500246526798));
#50204=CARTESIAN_POINT('Ctrl Pts',(1.691877054817,-1.,-3.64967689827393));
#50205=CARTESIAN_POINT('Ctrl Pts',(1.691877054817,1.,-3.64967689827393));
#50206=CARTESIAN_POINT('Ctrl Pts',(1.68641690471455,-1.,-3.64432638915199));
#50207=CARTESIAN_POINT('Ctrl Pts',(1.68641690471455,1.,-3.64432638915199));
#50208=CARTESIAN_POINT('Ctrl Pts',(1.68099146651577,-1.,-3.63895140887443));
#50209=CARTESIAN_POINT('Ctrl Pts',(1.68099146651577,1.,-3.63895140887443));
#50210=CARTESIAN_POINT('Ctrl Pts',(1.67560193613145,-1.,-3.63355343201211));
#50211=CARTESIAN_POINT('Ctrl Pts',(1.67560193613145,1.,-3.63355343201211));
#50212=CARTESIAN_POINT('Ctrl Pts',(1.67024966008037,-1.,-3.62813422105257));
#50213=CARTESIAN_POINT('Ctrl Pts',(1.67024966008037,1.,-3.62813422105257));
#50214=CARTESIAN_POINT('Ctrl Pts',(1.66493585923853,-1.,-3.62269517989104));
#50215=CARTESIAN_POINT('Ctrl Pts',(1.66493585923853,1.,-3.62269517989104));
#50216=CARTESIAN_POINT('Ctrl Pts',(1.65966133399186,-1.,-3.61723666482457));
#50217=CARTESIAN_POINT('Ctrl Pts',(1.65966133399186,1.,-3.61723666482457));
#50218=CARTESIAN_POINT('Ctrl Pts',(1.65442619244327,-1.,-3.61175734965129));
#50219=CARTESIAN_POINT('Ctrl Pts',(1.65442619244327,1.,-3.61175734965129));
#50220=CARTESIAN_POINT('Ctrl Pts',(1.64922952425833,-1.,-3.60625346556992));
#50221=CARTESIAN_POINT('Ctrl Pts',(1.64922952425833,1.,-3.60625346556992));
#50222=CARTESIAN_POINT('Ctrl Pts',(1.6440700438558,-1.,-3.6007202851384));
#50223=CARTESIAN_POINT('Ctrl Pts',(1.6440700438558,1.,-3.6007202851384));
#50224=CARTESIAN_POINT('Ctrl Pts',(1.63894676675349,-1.,-3.59515368334887));
#50225=CARTESIAN_POINT('Ctrl Pts',(1.63894676675349,1.,-3.59515368334887));
#50226=CARTESIAN_POINT('Ctrl Pts',(1.63385971451259,-1.,-3.58955176627876));
#50227=CARTESIAN_POINT('Ctrl Pts',(1.63385971451259,1.,-3.58955176627876));
#50228=CARTESIAN_POINT('Ctrl Pts',(1.62881051550748,-1.,-3.5839162577435));
#50229=CARTESIAN_POINT('Ctrl Pts',(1.62881051550748,1.,-3.5839162577435));
#50230=CARTESIAN_POINT('Ctrl Pts',(1.62380329464851,-1.,-3.57825455954405));
#50231=CARTESIAN_POINT('Ctrl Pts',(1.62380329464851,1.,-3.57825455954405));
#50232=CARTESIAN_POINT('Ctrl Pts',(1.61884340915412,-1.,-3.57257679609826));
#50233=CARTESIAN_POINT('Ctrl Pts',(1.61884340915412,1.,-3.57257679609826));
#50234=CARTESIAN_POINT('Ctrl Pts',(1.61393581747522,-1.,-3.56689200468404));
#50235=CARTESIAN_POINT('Ctrl Pts',(1.61393581747522,1.,-3.56689200468404));
#50236=CARTESIAN_POINT('Ctrl Pts',(1.60908344685459,-1.,-3.56120432482986));
#50237=CARTESIAN_POINT('Ctrl Pts',(1.60908344685459,1.,-3.56120432482986));
#50238=CARTESIAN_POINT('Ctrl Pts',(1.60428584699848,-1.,-3.55550985096117));
#50239=CARTESIAN_POINT('Ctrl Pts',(1.60428584699848,1.,-3.55550985096117));
#50240=CARTESIAN_POINT('Ctrl Pts',(1.59953698113444,-1.,-3.54979148634426));
#50241=CARTESIAN_POINT('Ctrl Pts',(1.59953698113444,1.,-3.54979148634426));
#50242=CARTESIAN_POINT('Ctrl Pts',(1.5948276694975,-1.,-3.544024581823));
#50243=CARTESIAN_POINT('Ctrl Pts',(1.5948276694975,1.,-3.544024581823));
#50244=CARTESIAN_POINT('Ctrl Pts',(1.59014958368725,-1.,-3.53818616861045));
#50245=CARTESIAN_POINT('Ctrl Pts',(1.59014958368725,1.,-3.53818616861045));
#50246=CARTESIAN_POINT('Ctrl Pts',(1.58549906268083,-1.,-3.53226378147068));
#50247=CARTESIAN_POINT('Ctrl Pts',(1.58549906268083,1.,-3.53226378147068));
#50248=CARTESIAN_POINT('Ctrl Pts',(1.58088027227856,-1.,-3.52626275334899));
#50249=CARTESIAN_POINT('Ctrl Pts',(1.58088027227856,1.,-3.52626275334899));
#50250=CARTESIAN_POINT('Ctrl Pts',(1.5763104998818,-1.,-3.52021847865961));
#50251=CARTESIAN_POINT('Ctrl Pts',(1.5763104998818,1.,-3.52021847865961));
#50252=CARTESIAN_POINT('Ctrl Pts',(1.57181569799774,-1.,-3.51418598431733));
#50253=CARTESIAN_POINT('Ctrl Pts',(1.57181569799774,1.,-3.51418598431733));
#50254=CARTESIAN_POINT('Ctrl Pts',(1.56742097575041,-1.,-3.50821771695427));
#50255=CARTESIAN_POINT('Ctrl Pts',(1.56742097575041,1.,-3.50821771695427));
#50256=CARTESIAN_POINT('Ctrl Pts',(1.56314187758689,-1.,-3.50234321621607));
#50257=CARTESIAN_POINT('Ctrl Pts',(1.56314187758689,1.,-3.50234321621607));
#50258=CARTESIAN_POINT('Ctrl Pts',(1.55897703097859,-1.,-3.49655185179623));
#50259=CARTESIAN_POINT('Ctrl Pts',(1.55897703097859,1.,-3.49655185179623));
#50260=CARTESIAN_POINT('Ctrl Pts',(1.5548959590107,-1.,-3.49076460877317));
#50261=CARTESIAN_POINT('Ctrl Pts',(1.5548959590107,1.,-3.49076460877317));
#50262=CARTESIAN_POINT('Ctrl Pts',(1.55084702970382,-1.,-3.48485155928414));
#50263=CARTESIAN_POINT('Ctrl Pts',(1.55084702970382,1.,-3.48485155928414));
#50264=CARTESIAN_POINT('Ctrl Pts',(1.54678009290206,-1.,-3.47868272898599));
#50265=CARTESIAN_POINT('Ctrl Pts',(1.54678009290206,1.,-3.47868272898599));
#50266=CARTESIAN_POINT('Ctrl Pts',(1.54266605398152,-1.,-3.47217189224576));
#50267=CARTESIAN_POINT('Ctrl Pts',(1.54266605398152,1.,-3.47217189224576));
#50268=CARTESIAN_POINT('Ctrl Pts',(1.53851507915533,-1.,-3.46531752207222));
#50269=CARTESIAN_POINT('Ctrl Pts',(1.53851507915533,1.,-3.46531752207222));
#50270=CARTESIAN_POINT('Ctrl Pts',(1.53440195378902,-1.,-3.45825932955273));
#50271=CARTESIAN_POINT('Ctrl Pts',(1.53440195378902,1.,-3.45825932955273));
#50272=CARTESIAN_POINT('Ctrl Pts',(1.530462444618,-1.,-3.45127136828667));
#50273=CARTESIAN_POINT('Ctrl Pts',(1.530462444618,1.,-3.45127136828667));
#50274=CARTESIAN_POINT('Ctrl Pts',(1.52686242875717,-1.,-3.44469547527));
#50275=CARTESIAN_POINT('Ctrl Pts',(1.52686242875717,1.,-3.44469547527));
#50276=CARTESIAN_POINT('Ctrl Pts',(1.52377348950429,-1.,-3.43888895974182));
#50277=CARTESIAN_POINT('Ctrl Pts',(1.52377348950429,1.,-3.43888895974182));
#50278=CARTESIAN_POINT('Ctrl Pts',(1.52134826724227,-1.,-3.43417156977749));
#50279=CARTESIAN_POINT('Ctrl Pts',(1.52134826724227,1.,-3.43417156977749));
#50280=CARTESIAN_POINT('Ctrl Pts',(1.51969006980792,-1.,-3.43076036253384));
#50281=CARTESIAN_POINT('Ctrl Pts',(1.51969006980792,1.,-3.43076036253384));
#50282=CARTESIAN_POINT('Ctrl Pts',(1.51901585838879,-1.,-3.42915787669388));
#50283=CARTESIAN_POINT('Ctrl Pts',(1.51901585838879,1.,-3.42915787669388));
#50284=CARTESIAN_POINT('Ctrl Pts',(1.51888450659497,-1.,-3.42860527148835));
#50285=CARTESIAN_POINT('Ctrl Pts',(1.51888450659497,1.,-3.42860527148835));
#50286=CARTESIAN_POINT('Ctrl Pts',(1.51896318668306,-1.,-3.42852521763648));
#50287=CARTESIAN_POINT('Ctrl Pts',(1.51896318668306,1.,-3.42852521763648));
#50288=CARTESIAN_POINT('Ctrl Pts',(1.519044091397,-1.,-3.42855728381368));
#50289=CARTESIAN_POINT('Ctrl Pts',(1.519044091397,1.,-3.42855728381368));
#50290=CARTESIAN_POINT('',(1.83867539237861,1.,-3.77614523045147));
#50291=CARTESIAN_POINT('Ctrl Pts',(1.83867539237861,1.,-3.77614523045147));
#50292=CARTESIAN_POINT('Ctrl Pts',(1.83742834010821,1.,-3.77518714458232));
#50293=CARTESIAN_POINT('Ctrl Pts',(1.83493697935064,1.,-3.77326886065484));
#50294=CARTESIAN_POINT('Ctrl Pts',(1.83120816956515,1.,-3.77038509819777));
#50295=CARTESIAN_POINT('Ctrl Pts',(1.82625289221933,1.,-3.76652740355856));
#50296=CARTESIAN_POINT('Ctrl Pts',(1.82008629694924,1.,-3.76168412709652));
#50297=CARTESIAN_POINT('Ctrl Pts',(1.81394729834032,1.,-3.75681965683995));
#50298=CARTESIAN_POINT('Ctrl Pts',(1.80783603939662,1.,-3.75193395888069));
#50299=CARTESIAN_POINT('Ctrl Pts',(1.80175271485519,1.,-3.74702700874954));
#50300=CARTESIAN_POINT('Ctrl Pts',(1.79569757859041,1.,-3.74209880351667));
#50301=CARTESIAN_POINT('Ctrl Pts',(1.78967092823139,1.,-3.73714934729962));
#50302=CARTESIAN_POINT('Ctrl Pts',(1.78367308442682,1.,-3.73217863095022));
#50303=CARTESIAN_POINT('Ctrl Pts',(1.77770437039606,1.,-3.72718661205504));
#50304=CARTESIAN_POINT('Ctrl Pts',(1.77176509401846,1.,-3.72217319911429));
#50305=CARTESIAN_POINT('Ctrl Pts',(1.76585552124549,1.,-3.71713822377676));
#50306=CARTESIAN_POINT('Ctrl Pts',(1.75997588499021,1.,-3.71208146346455));
#50307=CARTESIAN_POINT('Ctrl Pts',(1.75412641804148,1.,-3.70700269736876));
#50308=CARTESIAN_POINT('Ctrl Pts',(1.74830738046092,1.,-3.70190175673422));
#50309=CARTESIAN_POINT('Ctrl Pts',(1.74251908492589,1.,-3.6967785691046));
#50310=CARTESIAN_POINT('Ctrl Pts',(1.73676193254493,1.,-3.69163322647906));
#50311=CARTESIAN_POINT('Ctrl Pts',(1.73103640956647,1.,-3.68646597019188));
#50312=CARTESIAN_POINT('Ctrl Pts',(1.72534302437003,1.,-3.68127704936472));
#50313=CARTESIAN_POINT('Ctrl Pts',(1.71968225581787,1.,-3.67606660374665));
#50314=CARTESIAN_POINT('Ctrl Pts',(1.71405450210392,1.,-3.67083454901629));
#50315=CARTESIAN_POINT('Ctrl Pts',(1.70846001610983,1.,-3.6655804319893));
#50316=CARTESIAN_POINT('Ctrl Pts',(1.70289888566904,1.,-3.6603033877491));
#50317=CARTESIAN_POINT('Ctrl Pts',(1.69737117722558,1.,-3.65500246526798));
#50318=CARTESIAN_POINT('Ctrl Pts',(1.691877054817,1.,-3.64967689827393));
#50319=CARTESIAN_POINT('Ctrl Pts',(1.68641690471455,1.,-3.64432638915199));
#50320=CARTESIAN_POINT('Ctrl Pts',(1.68099146651577,1.,-3.63895140887443));
#50321=CARTESIAN_POINT('Ctrl Pts',(1.67560193613145,1.,-3.63355343201211));
#50322=CARTESIAN_POINT('Ctrl Pts',(1.67024966008037,1.,-3.62813422105257));
#50323=CARTESIAN_POINT('Ctrl Pts',(1.66493585923853,1.,-3.62269517989104));
#50324=CARTESIAN_POINT('Ctrl Pts',(1.65966133399186,1.,-3.61723666482457));
#50325=CARTESIAN_POINT('Ctrl Pts',(1.65442619244327,1.,-3.61175734965129));
#50326=CARTESIAN_POINT('Ctrl Pts',(1.64922952425833,1.,-3.60625346556992));
#50327=CARTESIAN_POINT('Ctrl Pts',(1.6440700438558,1.,-3.6007202851384));
#50328=CARTESIAN_POINT('Ctrl Pts',(1.63894676675349,1.,-3.59515368334887));
#50329=CARTESIAN_POINT('Ctrl Pts',(1.63385971451259,1.,-3.58955176627876));
#50330=CARTESIAN_POINT('Ctrl Pts',(1.62881051550748,1.,-3.5839162577435));
#50331=CARTESIAN_POINT('Ctrl Pts',(1.62380329464851,1.,-3.57825455954405));
#50332=CARTESIAN_POINT('Ctrl Pts',(1.61884340915412,1.,-3.57257679609826));
#50333=CARTESIAN_POINT('Ctrl Pts',(1.61393581747522,1.,-3.56689200468404));
#50334=CARTESIAN_POINT('Ctrl Pts',(1.60908344685459,1.,-3.56120432482986));
#50335=CARTESIAN_POINT('Ctrl Pts',(1.60428584699848,1.,-3.55550985096117));
#50336=CARTESIAN_POINT('Ctrl Pts',(1.59953698113444,1.,-3.54979148634426));
#50337=CARTESIAN_POINT('Ctrl Pts',(1.5948276694975,1.,-3.544024581823));
#50338=CARTESIAN_POINT('Ctrl Pts',(1.59014958368725,1.,-3.53818616861045));
#50339=CARTESIAN_POINT('Ctrl Pts',(1.58549906268083,1.,-3.53226378147068));
#50340=CARTESIAN_POINT('Ctrl Pts',(1.58088027227856,1.,-3.52626275334899));
#50341=CARTESIAN_POINT('Ctrl Pts',(1.5763104998818,1.,-3.52021847865961));
#50342=CARTESIAN_POINT('Ctrl Pts',(1.57181569799774,1.,-3.51418598431733));
#50343=CARTESIAN_POINT('Ctrl Pts',(1.56742097575041,1.,-3.50821771695427));
#50344=CARTESIAN_POINT('Ctrl Pts',(1.56314187758689,1.,-3.50234321621607));
#50345=CARTESIAN_POINT('Ctrl Pts',(1.55897703097859,1.,-3.49655185179623));
#50346=CARTESIAN_POINT('Ctrl Pts',(1.5548959590107,1.,-3.49076460877317));
#50347=CARTESIAN_POINT('Ctrl Pts',(1.55084702970382,1.,-3.48485155928414));
#50348=CARTESIAN_POINT('Ctrl Pts',(1.54678009290206,1.,-3.47868272898599));
#50349=CARTESIAN_POINT('Ctrl Pts',(1.54266605398152,1.,-3.47217189224576));
#50350=CARTESIAN_POINT('Ctrl Pts',(1.53851507915533,1.,-3.46531752207222));
#50351=CARTESIAN_POINT('Ctrl Pts',(1.53440195378902,1.,-3.45825932955273));
#50352=CARTESIAN_POINT('Ctrl Pts',(1.530462444618,1.,-3.45127136828667));
#50353=CARTESIAN_POINT('Ctrl Pts',(1.52686242875717,1.,-3.44469547527));
#50354=CARTESIAN_POINT('Ctrl Pts',(1.52377348950429,1.,-3.43888895974182));
#50355=CARTESIAN_POINT('Ctrl Pts',(1.52134826724227,1.,-3.43417156977749));
#50356=CARTESIAN_POINT('Ctrl Pts',(1.5198144909343,1.,-3.43101631893491));
#50357=CARTESIAN_POINT('Ctrl Pts',(1.51914806898539,1.,-3.42946838852728));
#50358=CARTESIAN_POINT('Ctrl Pts',(1.51895133295017,1.,-3.42884302333978));
#50359=CARTESIAN_POINT('Ctrl Pts',(1.51893924967231,1.,-3.42864616361967));
#50360=CARTESIAN_POINT('Ctrl Pts',(1.51895082866166,1.,-3.42859860294378));
#50361=CARTESIAN_POINT('',(1.83867539237861,0.,-3.77614523045147));
#50362=CARTESIAN_POINT('Ctrl Pts',(1.8808893942881,-1.,-3.24418789321065));
#50363=CARTESIAN_POINT('Ctrl Pts',(1.8808893942881,1.,-3.24418789321065));
#50364=CARTESIAN_POINT('Ctrl Pts',(1.8809110068042,-1.,-3.24410359189733));
#50365=CARTESIAN_POINT('Ctrl Pts',(1.8809110068042,1.,-3.24410359189733));
#50366=CARTESIAN_POINT('Ctrl Pts',(1.8810220187274,-1.,-3.24408699284449));
#50367=CARTESIAN_POINT('Ctrl Pts',(1.8810220187274,1.,-3.24408699284449));
#50368=CARTESIAN_POINT('Ctrl Pts',(1.88139187908347,-1.,-3.24451807186964));
#50369=CARTESIAN_POINT('Ctrl Pts',(1.88139187908347,1.,-3.24451807186964));
#50370=CARTESIAN_POINT('Ctrl Pts',(1.88229202583187,-1.,-3.24600543790876));
#50371=CARTESIAN_POINT('Ctrl Pts',(1.88229202583187,1.,-3.24600543790876));
#50372=CARTESIAN_POINT('Ctrl Pts',(1.88407708646435,-1.,-3.24935200512055));
#50373=CARTESIAN_POINT('Ctrl Pts',(1.88407708646435,1.,-3.24935200512055));
#50374=CARTESIAN_POINT('Ctrl Pts',(1.88646802523372,-1.,-3.25408686339298));
#50375=CARTESIAN_POINT('Ctrl Pts',(1.88646802523372,1.,-3.25408686339298));
#50376=CARTESIAN_POINT('Ctrl Pts',(1.88934996203508,-1.,-3.2599988519361));
#50377=CARTESIAN_POINT('Ctrl Pts',(1.88934996203508,1.,-3.2599988519361));
#50378=CARTESIAN_POINT('Ctrl Pts',(1.89255393500769,-1.,-3.2667765388833));
#50379=CARTESIAN_POINT('Ctrl Pts',(1.89255393500769,1.,-3.2667765388833));
#50380=CARTESIAN_POINT('Ctrl Pts',(1.89589172903662,-1.,-3.27407108932908));
#50381=CARTESIAN_POINT('Ctrl Pts',(1.89589172903662,1.,-3.27407108932908));
#50382=CARTESIAN_POINT('Ctrl Pts',(1.89918429230424,-1.,-3.28154737912287));
#50383=CARTESIAN_POINT('Ctrl Pts',(1.89918429230424,1.,-3.28154737912287));
#50384=CARTESIAN_POINT('Ctrl Pts',(1.9022897124757,-1.,-3.28893448600364));
#50385=CARTESIAN_POINT('Ctrl Pts',(1.9022897124757,1.,-3.28893448600364));
#50386=CARTESIAN_POINT('Ctrl Pts',(1.9051389186417,-1.,-3.29608978722258));
#50387=CARTESIAN_POINT('Ctrl Pts',(1.9051389186417,1.,-3.29608978722258));
#50388=CARTESIAN_POINT('Ctrl Pts',(1.90773912171424,-1.,-3.30300595568341));
#50389=CARTESIAN_POINT('Ctrl Pts',(1.90773912171424,1.,-3.30300595568341));
#50390=CARTESIAN_POINT('Ctrl Pts',(1.91014297830502,-1.,-3.30975721158694));
#50391=CARTESIAN_POINT('Ctrl Pts',(1.91014297830502,1.,-3.30975721158694));
#50392=CARTESIAN_POINT('Ctrl Pts',(1.91242616234459,-1.,-3.31646052426395));
#50393=CARTESIAN_POINT('Ctrl Pts',(1.91242616234459,1.,-3.31646052426395));
#50394=CARTESIAN_POINT('Ctrl Pts',(1.91466343916612,-1.,-3.32323403454507));
#50395=CARTESIAN_POINT('Ctrl Pts',(1.91466343916612,1.,-3.32323403454507));
#50396=CARTESIAN_POINT('Ctrl Pts',(1.91690081930297,-1.,-3.33014884257812));
#50397=CARTESIAN_POINT('Ctrl Pts',(1.91690081930297,1.,-3.33014884257812));
#50398=CARTESIAN_POINT('Ctrl Pts',(1.91914609610173,-1.,-3.33721230709948));
#50399=CARTESIAN_POINT('Ctrl Pts',(1.91914609610173,1.,-3.33721230709948));
#50400=CARTESIAN_POINT('Ctrl Pts',(1.92138450828378,-1.,-3.34439448941915));
#50401=CARTESIAN_POINT('Ctrl Pts',(1.92138450828378,1.,-3.34439448941915));
#50402=CARTESIAN_POINT('Ctrl Pts',(1.92358838440518,-1.,-3.35164424847207));
#50403=CARTESIAN_POINT('Ctrl Pts',(1.92358838440518,1.,-3.35164424847207));
#50404=CARTESIAN_POINT('Ctrl Pts',(1.92572846125763,-1.,-3.35890824422976));
#50405=CARTESIAN_POINT('Ctrl Pts',(1.92572846125763,1.,-3.35890824422976));
#50406=CARTESIAN_POINT('Ctrl Pts',(1.92778626543803,-1.,-3.36615168657597));
#50407=CARTESIAN_POINT('Ctrl Pts',(1.92778626543803,1.,-3.36615168657597));
#50408=CARTESIAN_POINT('Ctrl Pts',(1.92975993109897,-1.,-3.37336807068078));
#50409=CARTESIAN_POINT('Ctrl Pts',(1.92975993109897,1.,-3.37336807068078));
#50410=CARTESIAN_POINT('Ctrl Pts',(1.93165739093292,-1.,-3.38056768525577));
#50411=CARTESIAN_POINT('Ctrl Pts',(1.93165739093292,1.,-3.38056768525577));
#50412=CARTESIAN_POINT('Ctrl Pts',(1.93349233176794,-1.,-3.38777076883267));
#50413=CARTESIAN_POINT('Ctrl Pts',(1.93349233176794,1.,-3.38777076883267));
#50414=CARTESIAN_POINT('Ctrl Pts',(1.93527929945982,-1.,-3.39499923640789));
#50415=CARTESIAN_POINT('Ctrl Pts',(1.93527929945982,1.,-3.39499923640789));
#50416=CARTESIAN_POINT('Ctrl Pts',(1.93702857723089,-1.,-3.40226802104093));
#50417=CARTESIAN_POINT('Ctrl Pts',(1.93702857723089,1.,-3.40226802104093));
#50418=CARTESIAN_POINT('Ctrl Pts',(1.93874306008132,-1.,-3.40957978266623));
#50419=CARTESIAN_POINT('Ctrl Pts',(1.93874306008132,1.,-3.40957978266623));
#50420=CARTESIAN_POINT('Ctrl Pts',(1.94042111965237,-1.,-3.41692971994082));
#50421=CARTESIAN_POINT('Ctrl Pts',(1.94042111965237,1.,-3.41692971994082));
#50422=CARTESIAN_POINT('Ctrl Pts',(1.94205835913692,-1.,-3.42430850941497));
#50423=CARTESIAN_POINT('Ctrl Pts',(1.94205835913692,1.,-3.42430850941497));
#50424=CARTESIAN_POINT('Ctrl Pts',(1.94364973660285,-1.,-3.43170586602436));
#50425=CARTESIAN_POINT('Ctrl Pts',(1.94364973660285,1.,-3.43170586602436));
#50426=CARTESIAN_POINT('Ctrl Pts',(1.94519168842883,-1.,-3.43911410197693));
#50427=CARTESIAN_POINT('Ctrl Pts',(1.94519168842883,1.,-3.43911410197693));
#50428=CARTESIAN_POINT('Ctrl Pts',(1.94668377715332,-1.,-3.44653088665685));
#50429=CARTESIAN_POINT('Ctrl Pts',(1.94668377715332,1.,-3.44653088665685));
#50430=CARTESIAN_POINT('Ctrl Pts',(1.94812754766524,-1.,-3.45395731584051));
#50431=CARTESIAN_POINT('Ctrl Pts',(1.94812754766524,1.,-3.45395731584051));
#50432=CARTESIAN_POINT('Ctrl Pts',(1.94952575850196,-1.,-3.46139661060959));
#50433=CARTESIAN_POINT('Ctrl Pts',(1.94952575850196,1.,-3.46139661060959));
#50434=CARTESIAN_POINT('Ctrl Pts',(1.95088147859876,-1.,-3.4688525897419));
#50435=CARTESIAN_POINT('Ctrl Pts',(1.95088147859876,1.,-3.4688525897419));
#50436=CARTESIAN_POINT('Ctrl Pts',(1.95219722189878,-1.,-3.47632820495926));
#50437=CARTESIAN_POINT('Ctrl Pts',(1.95219722189878,1.,-3.47632820495926));
#50438=CARTESIAN_POINT('Ctrl Pts',(1.95347412486316,-1.,-3.48382414832649));
#50439=CARTESIAN_POINT('Ctrl Pts',(1.95347412486316,1.,-3.48382414832649));
#50440=CARTESIAN_POINT('Ctrl Pts',(1.95471236969653,-1.,-3.49133956289154));
#50441=CARTESIAN_POINT('Ctrl Pts',(1.95471236969653,1.,-3.49133956289154));
#50442=CARTESIAN_POINT('Ctrl Pts',(1.9559115382367,-1.,-3.49887263575602));
#50443=CARTESIAN_POINT('Ctrl Pts',(1.9559115382367,1.,-3.49887263575602));
#50444=CARTESIAN_POINT('Ctrl Pts',(1.95707099606513,-1.,-3.50642124159913));
#50445=CARTESIAN_POINT('Ctrl Pts',(1.95707099606513,1.,-3.50642124159913));
#50446=CARTESIAN_POINT('Ctrl Pts',(1.95819025316768,-1.,-3.51398354617773));
#50447=CARTESIAN_POINT('Ctrl Pts',(1.95819025316768,1.,-3.51398354617773));
#50448=CARTESIAN_POINT('Ctrl Pts',(1.95926936324436,-1.,-3.52155867431438));
#50449=CARTESIAN_POINT('Ctrl Pts',(1.95926936324436,1.,-3.52155867431438));
#50450=CARTESIAN_POINT('Ctrl Pts',(1.96030879411534,-1.,-3.52914648844289));
#50451=CARTESIAN_POINT('Ctrl Pts',(1.96030879411534,1.,-3.52914648844289));
#50452=CARTESIAN_POINT('Ctrl Pts',(1.96130926212661,-1.,-3.53674730625759));
#50453=CARTESIAN_POINT('Ctrl Pts',(1.96130926212661,1.,-3.53674730625759));
#50454=CARTESIAN_POINT('Ctrl Pts',(1.96227157573058,-1.,-3.54436163300425));
#50455=CARTESIAN_POINT('Ctrl Pts',(1.96227157573058,1.,-3.54436163300425));
#50456=CARTESIAN_POINT('Ctrl Pts',(1.96319648628667,-1.,-3.55198990600929));
#50457=CARTESIAN_POINT('Ctrl Pts',(1.96319648628667,1.,-3.55198990600929));
#50458=CARTESIAN_POINT('Ctrl Pts',(1.96408450906868,-1.,-3.55963218706201));
#50459=CARTESIAN_POINT('Ctrl Pts',(1.96408450906868,1.,-3.55963218706201));
#50460=CARTESIAN_POINT('Ctrl Pts',(1.96493594634643,-1.,-3.56728820357933));
#50461=CARTESIAN_POINT('Ctrl Pts',(1.96493594634643,1.,-3.56728820357933));
#50462=CARTESIAN_POINT('Ctrl Pts',(1.96575096652857,-1.,-3.57495748601088));
#50463=CARTESIAN_POINT('Ctrl Pts',(1.96575096652857,1.,-3.57495748601088));
#50464=CARTESIAN_POINT('Ctrl Pts',(1.9665296668894,-1.,-3.58263947663884));
#50465=CARTESIAN_POINT('Ctrl Pts',(1.9665296668894,1.,-3.58263947663884));
#50466=CARTESIAN_POINT('Ctrl Pts',(1.96727213799507,-1.,-3.5903336402273));
#50467=CARTESIAN_POINT('Ctrl Pts',(1.96727213799507,1.,-3.5903336402273));
#50468=CARTESIAN_POINT('Ctrl Pts',(1.96797854118257,-1.,-3.59803959819725));
#50469=CARTESIAN_POINT('Ctrl Pts',(1.96797854118257,1.,-3.59803959819725));
#50470=CARTESIAN_POINT('Ctrl Pts',(1.96864911885775,-1.,-3.60575714017676));
#50471=CARTESIAN_POINT('Ctrl Pts',(1.96864911885775,1.,-3.60575714017676));
#50472=CARTESIAN_POINT('Ctrl Pts',(1.96928416040712,-1.,-3.61348615496393));
#50473=CARTESIAN_POINT('Ctrl Pts',(1.96928416040712,1.,-3.61348615496393));
#50474=CARTESIAN_POINT('Ctrl Pts',(1.96988398129888,-1.,-3.62122658401722));
#50475=CARTESIAN_POINT('Ctrl Pts',(1.96988398129888,1.,-3.62122658401722));
#50476=CARTESIAN_POINT('Ctrl Pts',(1.97044889850518,-1.,-3.62897836973397));
#50477=CARTESIAN_POINT('Ctrl Pts',(1.97044889850518,1.,-3.62897836973397));
#50478=CARTESIAN_POINT('Ctrl Pts',(1.97097920454698,-1.,-3.63674139590853));
#50479=CARTESIAN_POINT('Ctrl Pts',(1.97097920454698,1.,-3.63674139590853));
#50480=CARTESIAN_POINT('Ctrl Pts',(1.97147515441539,-1.,-3.64451546724222));
#50481=CARTESIAN_POINT('Ctrl Pts',(1.97147515441539,1.,-3.64451546724222));
#50482=CARTESIAN_POINT('Ctrl Pts',(1.97193697240645,-1.,-3.65230034717364));
#50483=CARTESIAN_POINT('Ctrl Pts',(1.97193697240645,1.,-3.65230034717364));
#50484=CARTESIAN_POINT('Ctrl Pts',(1.97236485439317,-1.,-3.66009578166865));
#50485=CARTESIAN_POINT('Ctrl Pts',(1.97236485439317,1.,-3.66009578166865));
#50486=CARTESIAN_POINT('Ctrl Pts',(1.9727589719863,-1.,-3.66790152751984));
#50487=CARTESIAN_POINT('Ctrl Pts',(1.9727589719863,1.,-3.66790152751984));
#50488=CARTESIAN_POINT('Ctrl Pts',(1.97311947678035,-1.,-3.67571738106175));
#50489=CARTESIAN_POINT('Ctrl Pts',(1.97311947678035,1.,-3.67571738106175));
#50490=CARTESIAN_POINT('Ctrl Pts',(1.9734465030363,-1.,-3.68354319913416));
#50491=CARTESIAN_POINT('Ctrl Pts',(1.9734465030363,1.,-3.68354319913416));
#50492=CARTESIAN_POINT('Ctrl Pts',(1.97374016224397,-1.,-3.69137888597855));
#50493=CARTESIAN_POINT('Ctrl Pts',(1.97374016224397,1.,-3.69137888597855));
#50494=CARTESIAN_POINT('Ctrl Pts',(1.97394846382288,-1.,-3.69765528558292));
#50495=CARTESIAN_POINT('Ctrl Pts',(1.97394846382288,1.,-3.69765528558292));
#50496=CARTESIAN_POINT('Ctrl Pts',(1.97408973726149,-1.,-3.70236698911837));
#50497=CARTESIAN_POINT('Ctrl Pts',(1.97408973726149,1.,-3.70236698911837));
#50498=CARTESIAN_POINT('Ctrl Pts',(1.974177276451,-1.,-3.7055100813194));
#50499=CARTESIAN_POINT('Ctrl Pts',(1.974177276451,1.,-3.7055100813194));
#50500=CARTESIAN_POINT('Ctrl Pts',(1.97421938526992,-1.,-3.70708211654725));
#50501=CARTESIAN_POINT('Ctrl Pts',(1.97421938526992,1.,-3.70708211654725));
#50502=CARTESIAN_POINT('',(1.88097764062542,1.,-3.24413672884902));
#50503=CARTESIAN_POINT('Ctrl Pts',(1.88097764062541,-1.,-3.24413672884902));
#50504=CARTESIAN_POINT('Ctrl Pts',(1.88097764062541,-0.666666666666667,
-3.24413672884902));
#50505=CARTESIAN_POINT('Ctrl Pts',(1.88097764062541,-0.333333333333333,
-3.24413672884902));
#50506=CARTESIAN_POINT('Ctrl Pts',(1.88097764062541,0.333333333333333,-3.24413672884902));
#50507=CARTESIAN_POINT('Ctrl Pts',(1.88097764062541,0.666666666666667,-3.24413672884902));
#50508=CARTESIAN_POINT('Ctrl Pts',(1.88097764062541,1.,-3.24413672884902));
#50509=CARTESIAN_POINT('',(1.97421938526992,1.,-3.70708211654725));
#50510=CARTESIAN_POINT('',(1.97421938526992,0.,-3.70708211654725));
#50511=CARTESIAN_POINT('Ctrl Pts',(1.88097764062542,1.,-3.24413672884902));
#50512=CARTESIAN_POINT('Ctrl Pts',(1.88102292397987,1.,-3.24415531671311));
#50513=CARTESIAN_POINT('Ctrl Pts',(1.88117508446657,1.,-3.24428080352952));
#50514=CARTESIAN_POINT('Ctrl Pts',(1.88156537699118,1.,-3.24480754675942));
#50515=CARTESIAN_POINT('Ctrl Pts',(1.88242596600422,1.,-3.24625654410705));
#50516=CARTESIAN_POINT('Ctrl Pts',(1.88407708646435,1.,-3.24935200512055));
#50517=CARTESIAN_POINT('Ctrl Pts',(1.88646802523372,1.,-3.25408686339298));
#50518=CARTESIAN_POINT('Ctrl Pts',(1.88934996203508,1.,-3.2599988519361));
#50519=CARTESIAN_POINT('Ctrl Pts',(1.89255393500769,1.,-3.2667765388833));
#50520=CARTESIAN_POINT('Ctrl Pts',(1.89589172903662,1.,-3.27407108932908));
#50521=CARTESIAN_POINT('Ctrl Pts',(1.89918429230424,1.,-3.28154737912287));
#50522=CARTESIAN_POINT('Ctrl Pts',(1.9022897124757,1.,-3.28893448600364));
#50523=CARTESIAN_POINT('Ctrl Pts',(1.9051389186417,1.,-3.29608978722258));
#50524=CARTESIAN_POINT('Ctrl Pts',(1.90773912171424,1.,-3.30300595568341));
#50525=CARTESIAN_POINT('Ctrl Pts',(1.91014297830502,1.,-3.30975721158694));
#50526=CARTESIAN_POINT('Ctrl Pts',(1.91242616234459,1.,-3.31646052426395));
#50527=CARTESIAN_POINT('Ctrl Pts',(1.91466343916612,1.,-3.32323403454507));
#50528=CARTESIAN_POINT('Ctrl Pts',(1.91690081930297,1.,-3.33014884257812));
#50529=CARTESIAN_POINT('Ctrl Pts',(1.91914609610173,1.,-3.33721230709948));
#50530=CARTESIAN_POINT('Ctrl Pts',(1.92138450828378,1.,-3.34439448941915));
#50531=CARTESIAN_POINT('Ctrl Pts',(1.92358838440518,1.,-3.35164424847207));
#50532=CARTESIAN_POINT('Ctrl Pts',(1.92572846125763,1.,-3.35890824422976));
#50533=CARTESIAN_POINT('Ctrl Pts',(1.92778626543803,1.,-3.36615168657597));
#50534=CARTESIAN_POINT('Ctrl Pts',(1.92975993109897,1.,-3.37336807068078));
#50535=CARTESIAN_POINT('Ctrl Pts',(1.93165739093292,1.,-3.38056768525577));
#50536=CARTESIAN_POINT('Ctrl Pts',(1.93349233176794,1.,-3.38777076883267));
#50537=CARTESIAN_POINT('Ctrl Pts',(1.93527929945982,1.,-3.39499923640789));
#50538=CARTESIAN_POINT('Ctrl Pts',(1.93702857723089,1.,-3.40226802104093));
#50539=CARTESIAN_POINT('Ctrl Pts',(1.93874306008132,1.,-3.40957978266623));
#50540=CARTESIAN_POINT('Ctrl Pts',(1.94042111965237,1.,-3.41692971994082));
#50541=CARTESIAN_POINT('Ctrl Pts',(1.94205835913692,1.,-3.42430850941497));
#50542=CARTESIAN_POINT('Ctrl Pts',(1.94364973660285,1.,-3.43170586602436));
#50543=CARTESIAN_POINT('Ctrl Pts',(1.94519168842883,1.,-3.43911410197693));
#50544=CARTESIAN_POINT('Ctrl Pts',(1.94668377715332,1.,-3.44653088665685));
#50545=CARTESIAN_POINT('Ctrl Pts',(1.94812754766524,1.,-3.45395731584051));
#50546=CARTESIAN_POINT('Ctrl Pts',(1.94952575850196,1.,-3.46139661060959));
#50547=CARTESIAN_POINT('Ctrl Pts',(1.95088147859876,1.,-3.4688525897419));
#50548=CARTESIAN_POINT('Ctrl Pts',(1.95219722189878,1.,-3.47632820495926));
#50549=CARTESIAN_POINT('Ctrl Pts',(1.95347412486316,1.,-3.48382414832649));
#50550=CARTESIAN_POINT('Ctrl Pts',(1.95471236969653,1.,-3.49133956289154));
#50551=CARTESIAN_POINT('Ctrl Pts',(1.9559115382367,1.,-3.49887263575602));
#50552=CARTESIAN_POINT('Ctrl Pts',(1.95707099606513,1.,-3.50642124159913));
#50553=CARTESIAN_POINT('Ctrl Pts',(1.95819025316768,1.,-3.51398354617773));
#50554=CARTESIAN_POINT('Ctrl Pts',(1.95926936324436,1.,-3.52155867431438));
#50555=CARTESIAN_POINT('Ctrl Pts',(1.96030879411534,1.,-3.52914648844289));
#50556=CARTESIAN_POINT('Ctrl Pts',(1.96130926212661,1.,-3.53674730625759));
#50557=CARTESIAN_POINT('Ctrl Pts',(1.96227157573058,1.,-3.54436163300425));
#50558=CARTESIAN_POINT('Ctrl Pts',(1.96319648628667,1.,-3.55198990600929));
#50559=CARTESIAN_POINT('Ctrl Pts',(1.96408450906868,1.,-3.55963218706201));
#50560=CARTESIAN_POINT('Ctrl Pts',(1.96493594634643,1.,-3.56728820357933));
#50561=CARTESIAN_POINT('Ctrl Pts',(1.96575096652857,1.,-3.57495748601088));
#50562=CARTESIAN_POINT('Ctrl Pts',(1.9665296668894,1.,-3.58263947663884));
#50563=CARTESIAN_POINT('Ctrl Pts',(1.96727213799507,1.,-3.5903336402273));
#50564=CARTESIAN_POINT('Ctrl Pts',(1.96797854118257,1.,-3.59803959819725));
#50565=CARTESIAN_POINT('Ctrl Pts',(1.96864911885775,1.,-3.60575714017676));
#50566=CARTESIAN_POINT('Ctrl Pts',(1.96928416040712,1.,-3.61348615496393));
#50567=CARTESIAN_POINT('Ctrl Pts',(1.96988398129888,1.,-3.62122658401722));
#50568=CARTESIAN_POINT('Ctrl Pts',(1.97044889850518,1.,-3.62897836973397));
#50569=CARTESIAN_POINT('Ctrl Pts',(1.97097920454698,1.,-3.63674139590853));
#50570=CARTESIAN_POINT('Ctrl Pts',(1.97147515441539,1.,-3.64451546724222));
#50571=CARTESIAN_POINT('Ctrl Pts',(1.97193697240645,1.,-3.65230034717364));
#50572=CARTESIAN_POINT('Ctrl Pts',(1.97236485439317,1.,-3.66009578166865));
#50573=CARTESIAN_POINT('Ctrl Pts',(1.9727589719863,1.,-3.66790152751984));
#50574=CARTESIAN_POINT('Ctrl Pts',(1.97311947678035,1.,-3.67571738106175));
#50575=CARTESIAN_POINT('Ctrl Pts',(1.9734465030363,1.,-3.68354319913416));
#50576=CARTESIAN_POINT('Ctrl Pts',(1.97374016224397,1.,-3.69137888597855));
#50577=CARTESIAN_POINT('Ctrl Pts',(1.97394846382288,1.,-3.69765528558292));
#50578=CARTESIAN_POINT('Ctrl Pts',(1.97408973726149,1.,-3.70236698911837));
#50579=CARTESIAN_POINT('Ctrl Pts',(1.974177276451,1.,-3.7055100813194));
#50580=CARTESIAN_POINT('Ctrl Pts',(1.97421938526992,1.,-3.70708211654725));
#50581=CARTESIAN_POINT('Origin',(1.97421938526992,0.,-3.70708211654725));
#50582=CARTESIAN_POINT('',(1.83867539237861,1.,-3.77614523045147));
#50583=CARTESIAN_POINT('Origin',(0.,0.,0.));
#50584=CARTESIAN_POINT('',(2.03660101169564,1.,-3.14877060440425));
#50585=CARTESIAN_POINT('Origin',(0.,1.,0.));
#50586=CARTESIAN_POINT('Ctrl Pts',(2.03660101169564,1.,-3.14877060440425));
#50587=CARTESIAN_POINT('Ctrl Pts',(2.03660101169564,0.666666666666667,-3.14877060440425));
#50588=CARTESIAN_POINT('Ctrl Pts',(2.03660101169564,0.333333333333333,-3.14877060440425));
#50589=CARTESIAN_POINT('Ctrl Pts',(2.03660101169564,-0.333333333333333,
-3.14877060440425));
#50590=CARTESIAN_POINT('Ctrl Pts',(2.03660101169564,-0.666666666666667,
-3.14877060440425));
#50591=CARTESIAN_POINT('Ctrl Pts',(2.03660101169564,-1.,-3.14877060440425));
#50592=CARTESIAN_POINT('Ctrl Pts',(2.40675750623143,-1.,-3.44202241512147));
#50593=CARTESIAN_POINT('Ctrl Pts',(2.40675750623143,1.,-3.44202241512147));
#50594=CARTESIAN_POINT('Ctrl Pts',(2.40537592959345,-1.,-3.44127120683402));
#50595=CARTESIAN_POINT('Ctrl Pts',(2.40537592959345,1.,-3.44127120683402));
#50596=CARTESIAN_POINT('Ctrl Pts',(2.40261515590099,-1.,-3.43976627485223));
#50597=CARTESIAN_POINT('Ctrl Pts',(2.40261515590099,1.,-3.43976627485223));
#50598=CARTESIAN_POINT('Ctrl Pts',(2.39848113411428,-1.,-3.43750133066037));
#50599=CARTESIAN_POINT('Ctrl Pts',(2.39848113411428,1.,-3.43750133066037));
#50600=CARTESIAN_POINT('Ctrl Pts',(2.39298338805823,-1.,-3.43446630680436));
#50601=CARTESIAN_POINT('Ctrl Pts',(2.39298338805823,1.,-3.43446630680436));
#50602=CARTESIAN_POINT('Ctrl Pts',(2.38613505844641,-1.,-3.43064732714472));
#50603=CARTESIAN_POINT('Ctrl Pts',(2.38613505844641,1.,-3.43064732714472));
#50604=CARTESIAN_POINT('Ctrl Pts',(2.37931067029517,-1.,-3.42680309755241));
#50605=CARTESIAN_POINT('Ctrl Pts',(2.37931067029517,1.,-3.42680309755241));
#50606=CARTESIAN_POINT('Ctrl Pts',(2.37251035954351,-1.,-3.42293356216595));
#50607=CARTESIAN_POINT('Ctrl Pts',(2.37251035954351,1.,-3.42293356216595));
#50608=CARTESIAN_POINT('Ctrl Pts',(2.36573431470313,-1.,-3.41903866635384));
#50609=CARTESIAN_POINT('Ctrl Pts',(2.36573431470313,1.,-3.41903866635384));
#50610=CARTESIAN_POINT('Ctrl Pts',(2.35898278606449,-1.,-3.4151183675076));
#50611=CARTESIAN_POINT('Ctrl Pts',(2.35898278606449,1.,-3.4151183675076));
#50612=CARTESIAN_POINT('Ctrl Pts',(2.35225606823649,-1.,-3.41117262313464));
#50613=CARTESIAN_POINT('Ctrl Pts',(2.35225606823649,1.,-3.41117262313464));
#50614=CARTESIAN_POINT('Ctrl Pts',(2.34555447648901,-1.,-3.40720137403888));
#50615=CARTESIAN_POINT('Ctrl Pts',(2.34555447648901,1.,-3.40720137403888));
#50616=CARTESIAN_POINT('Ctrl Pts',(2.33887832342715,-1.,-3.40320452776646));
#50617=CARTESIAN_POINT('Ctrl Pts',(2.33887832342715,1.,-3.40320452776646));
#50618=CARTESIAN_POINT('Ctrl Pts',(2.33222789882601,-1.,-3.39918194578115));
#50619=CARTESIAN_POINT('Ctrl Pts',(2.33222789882601,1.,-3.39918194578115));
#50620=CARTESIAN_POINT('Ctrl Pts',(2.32560343902683,-1.,-3.39513342020045));
#50621=CARTESIAN_POINT('Ctrl Pts',(2.32560343902683,1.,-3.39513342020045));
#50622=CARTESIAN_POINT('Ctrl Pts',(2.31900513925627,-1.,-3.39105869475112));
#50623=CARTESIAN_POINT('Ctrl Pts',(2.31900513925627,1.,-3.39105869475112));
#50624=CARTESIAN_POINT('Ctrl Pts',(2.31243319489505,-1.,-3.38695751492659));
#50625=CARTESIAN_POINT('Ctrl Pts',(2.31243319489505,1.,-3.38695751492659));
#50626=CARTESIAN_POINT('Ctrl Pts',(2.30588783640389,-1.,-3.38282967336676));
#50627=CARTESIAN_POINT('Ctrl Pts',(2.30588783640389,1.,-3.38282967336676));
#50628=CARTESIAN_POINT('Ctrl Pts',(2.29936936127588,-1.,-3.37867504959382));
#50629=CARTESIAN_POINT('Ctrl Pts',(2.29936936127588,1.,-3.37867504959382));
#50630=CARTESIAN_POINT('Ctrl Pts',(2.2928781800731,-1.,-3.37449367172707));
#50631=CARTESIAN_POINT('Ctrl Pts',(2.2928781800731,1.,-3.37449367172707));
#50632=CARTESIAN_POINT('Ctrl Pts',(2.28641481081045,-1.,-3.37028570206357));
#50633=CARTESIAN_POINT('Ctrl Pts',(2.28641481081045,1.,-3.37028570206357));
#50634=CARTESIAN_POINT('Ctrl Pts',(2.27997979457968,-1.,-3.36605130712978));
#50635=CARTESIAN_POINT('Ctrl Pts',(2.27997979457968,1.,-3.36605130712978));
#50636=CARTESIAN_POINT('Ctrl Pts',(2.27357362620902,-1.,-3.36179055004369));
#50637=CARTESIAN_POINT('Ctrl Pts',(2.27357362620902,1.,-3.36179055004369));
#50638=CARTESIAN_POINT('Ctrl Pts',(2.26719668579921,-1.,-3.35750328523077));
#50639=CARTESIAN_POINT('Ctrl Pts',(2.26719668579921,1.,-3.35750328523077));
#50640=CARTESIAN_POINT('Ctrl Pts',(2.26084915222484,-1.,-3.35318902552676));
#50641=CARTESIAN_POINT('Ctrl Pts',(2.26084915222484,1.,-3.35318902552676));
#50642=CARTESIAN_POINT('Ctrl Pts',(2.25453097693524,-1.,-3.34884690292342));
#50643=CARTESIAN_POINT('Ctrl Pts',(2.25453097693524,1.,-3.34884690292342));
#50644=CARTESIAN_POINT('Ctrl Pts',(2.24824207678287,-1.,-3.34447596770768));
#50645=CARTESIAN_POINT('Ctrl Pts',(2.24824207678287,1.,-3.34447596770768));
#50646=CARTESIAN_POINT('Ctrl Pts',(2.24198249391437,-1.,-3.34007543738044));
#50647=CARTESIAN_POINT('Ctrl Pts',(2.24198249391437,1.,-3.34007543738044));
#50648=CARTESIAN_POINT('Ctrl Pts',(2.23575256328809,-1.,-3.33564495756478));
#50649=CARTESIAN_POINT('Ctrl Pts',(2.23575256328809,1.,-3.33564495756478));
#50650=CARTESIAN_POINT('Ctrl Pts',(2.22955308907221,-1.,-3.33118487773593));
#50651=CARTESIAN_POINT('Ctrl Pts',(2.22955308907221,1.,-3.33118487773593));
#50652=CARTESIAN_POINT('Ctrl Pts',(2.22338548312758,-1.,-3.32669646722871));
#50653=CARTESIAN_POINT('Ctrl Pts',(2.22338548312758,1.,-3.32669646722871));
#50654=CARTESIAN_POINT('Ctrl Pts',(2.21725135110889,-1.,-3.32218125618955));
#50655=CARTESIAN_POINT('Ctrl Pts',(2.21725135110889,1.,-3.32218125618955));
#50656=CARTESIAN_POINT('Ctrl Pts',(2.21115211847872,-1.,-3.31764044024231));
#50657=CARTESIAN_POINT('Ctrl Pts',(2.21115211847872,1.,-3.31764044024231));
#50658=CARTESIAN_POINT('Ctrl Pts',(2.20508863150608,-1.,-3.3130742460895));
#50659=CARTESIAN_POINT('Ctrl Pts',(2.20508863150608,1.,-3.3130742460895));
#50660=CARTESIAN_POINT('Ctrl Pts',(2.19906078949924,-1.,-3.30848134694597));
#50661=CARTESIAN_POINT('Ctrl Pts',(2.19906078949924,1.,-3.30848134694597));
#50662=CARTESIAN_POINT('Ctrl Pts',(2.19306710376112,-1.,-3.30385816281831));
#50663=CARTESIAN_POINT('Ctrl Pts',(2.19306710376112,1.,-3.30385816281831));
#50664=CARTESIAN_POINT('Ctrl Pts',(2.18710556500325,-1.,-3.29920022557635));
#50665=CARTESIAN_POINT('Ctrl Pts',(2.18710556500325,1.,-3.29920022557635));
#50666=CARTESIAN_POINT('Ctrl Pts',(2.18117455557062,-1.,-3.29450361500484));
#50667=CARTESIAN_POINT('Ctrl Pts',(2.18117455557062,1.,-3.29450361500484));
#50668=CARTESIAN_POINT('Ctrl Pts',(2.17527380048422,-1.,-3.28976645712566));
#50669=CARTESIAN_POINT('Ctrl Pts',(2.17527380048422,1.,-3.28976645712566));
#50670=CARTESIAN_POINT('Ctrl Pts',(2.16940517773459,-1.,-3.2849901997973));
#50671=CARTESIAN_POINT('Ctrl Pts',(2.16940517773459,1.,-3.2849901997973));
#50672=CARTESIAN_POINT('Ctrl Pts',(2.16357391934434,-1.,-3.28018150841414));
#50673=CARTESIAN_POINT('Ctrl Pts',(2.16357391934434,1.,-3.28018150841414));
#50674=CARTESIAN_POINT('Ctrl Pts',(2.15778690038359,-1.,-3.27534954469206));
#50675=CARTESIAN_POINT('Ctrl Pts',(2.15778690038359,1.,-3.27534954469206));
#50676=CARTESIAN_POINT('Ctrl Pts',(2.15205043199818,-1.,-3.27050245897244));
#50677=CARTESIAN_POINT('Ctrl Pts',(2.15205043199818,1.,-3.27050245897244));
#50678=CARTESIAN_POINT('Ctrl Pts',(2.14636805295663,-1.,-3.26564388189764));
#50679=CARTESIAN_POINT('Ctrl Pts',(2.14636805295663,1.,-3.26564388189764));
#50680=CARTESIAN_POINT('Ctrl Pts',(2.14073870754257,-1.,-3.26077002641868));
#50681=CARTESIAN_POINT('Ctrl Pts',(2.14073870754257,1.,-3.26077002641868));
#50682=CARTESIAN_POINT('Ctrl Pts',(2.13515375878786,-1.,-3.25586495065027));
#50683=CARTESIAN_POINT('Ctrl Pts',(2.13515375878786,1.,-3.25586495065027));
#50684=CARTESIAN_POINT('Ctrl Pts',(2.1296002839681,-1.,-3.25090574493994));
#50685=CARTESIAN_POINT('Ctrl Pts',(2.1296002839681,1.,-3.25090574493994));
#50686=CARTESIAN_POINT('Ctrl Pts',(2.12406646410943,-1.,-3.24587102613347));
#50687=CARTESIAN_POINT('Ctrl Pts',(2.12406646410943,1.,-3.24587102613347));
#50688=CARTESIAN_POINT('Ctrl Pts',(2.11854673326972,-1.,-3.24074905517282));
#50689=CARTESIAN_POINT('Ctrl Pts',(2.11854673326972,1.,-3.24074905517282));
#50690=CARTESIAN_POINT('Ctrl Pts',(2.11304604021784,-1.,-3.23554444767115));
#50691=CARTESIAN_POINT('Ctrl Pts',(2.11304604021784,1.,-3.23554444767115));
#50692=CARTESIAN_POINT('Ctrl Pts',(2.1075869964248,-1.,-3.23028945793334));
#50693=CARTESIAN_POINT('Ctrl Pts',(2.1075869964248,1.,-3.23028945793334));
#50694=CARTESIAN_POINT('Ctrl Pts',(2.10220384298533,-1.,-3.22503437553496));
#50695=CARTESIAN_POINT('Ctrl Pts',(2.10220384298533,1.,-3.22503437553496));
#50696=CARTESIAN_POINT('Ctrl Pts',(2.09692958434933,-1.,-3.21982707347067));
#50697=CARTESIAN_POINT('Ctrl Pts',(2.09692958434933,1.,-3.21982707347067));
#50698=CARTESIAN_POINT('Ctrl Pts',(2.0917841946046,-1.,-3.2146942960168));
#50699=CARTESIAN_POINT('Ctrl Pts',(2.0917841946046,1.,-3.2146942960168));
#50700=CARTESIAN_POINT('Ctrl Pts',(2.08676465517435,-1.,-3.20962575845433));
#50701=CARTESIAN_POINT('Ctrl Pts',(2.08676465517435,1.,-3.20962575845433));
#50702=CARTESIAN_POINT('Ctrl Pts',(2.08182850370816,-1.,-3.20454818630635));
#50703=CARTESIAN_POINT('Ctrl Pts',(2.08182850370816,1.,-3.20454818630635));
#50704=CARTESIAN_POINT('Ctrl Pts',(2.0769044187063,-1.,-3.19934132835879));
#50705=CARTESIAN_POINT('Ctrl Pts',(2.0769044187063,1.,-3.19934132835879));
#50706=CARTESIAN_POINT('Ctrl Pts',(2.07192253497765,-1.,-3.19388465568113));
#50707=CARTESIAN_POINT('Ctrl Pts',(2.07192253497765,1.,-3.19388465568113));
#50708=CARTESIAN_POINT('Ctrl Pts',(2.06684062744065,-1.,-3.18809755562297));
#50709=CARTESIAN_POINT('Ctrl Pts',(2.06684062744065,1.,-3.18809755562297));
#50710=CARTESIAN_POINT('Ctrl Pts',(2.06166849827143,-1.,-3.18197692964677));
#50711=CARTESIAN_POINT('Ctrl Pts',(2.06166849827143,1.,-3.18197692964677));
#50712=CARTESIAN_POINT('Ctrl Pts',(2.05650186773279,-1.,-3.17564906975592));
#50713=CARTESIAN_POINT('Ctrl Pts',(2.05650186773279,1.,-3.17564906975592));
#50714=CARTESIAN_POINT('Ctrl Pts',(2.05151770247452,-1.,-3.16936341689859));
#50715=CARTESIAN_POINT('Ctrl Pts',(2.05151770247452,1.,-3.16936341689859));
#50716=CARTESIAN_POINT('Ctrl Pts',(2.0469333124766,-1.,-3.16343165059235));
#50717=CARTESIAN_POINT('Ctrl Pts',(2.0469333124766,1.,-3.16343165059235));
#50718=CARTESIAN_POINT('Ctrl Pts',(2.04297406404132,-1.,-3.15817983946525));
#50719=CARTESIAN_POINT('Ctrl Pts',(2.04297406404132,1.,-3.15817983946525));
#50720=CARTESIAN_POINT('Ctrl Pts',(2.03984073791432,-1.,-3.1538999167466));
#50721=CARTESIAN_POINT('Ctrl Pts',(2.03984073791432,1.,-3.1538999167466));
#50722=CARTESIAN_POINT('Ctrl Pts',(2.03766932526171,-1.,-3.15079010635326));
#50723=CARTESIAN_POINT('Ctrl Pts',(2.03766932526171,1.,-3.15079010635326));
#50724=CARTESIAN_POINT('Ctrl Pts',(2.03675273048882,-1.,-3.14931281967585));
#50725=CARTESIAN_POINT('Ctrl Pts',(2.03675273048882,1.,-3.14931281967585));
#50726=CARTESIAN_POINT('Ctrl Pts',(2.03653654935384,-1.,-3.14878756590499));
#50727=CARTESIAN_POINT('Ctrl Pts',(2.03653654935384,1.,-3.14878756590499));
#50728=CARTESIAN_POINT('Ctrl Pts',(2.036601737578,-1.,-3.14869618937139));
#50729=CARTESIAN_POINT('Ctrl Pts',(2.036601737578,1.,-3.14869618937139));
#50730=CARTESIAN_POINT('Ctrl Pts',(2.03668666247593,-1.,-3.1487152044751));
#50731=CARTESIAN_POINT('Ctrl Pts',(2.03668666247593,1.,-3.1487152044751));
#50732=CARTESIAN_POINT('',(2.40675750623143,1.,-3.44202241512147));
#50733=CARTESIAN_POINT('Ctrl Pts',(2.40675750623143,1.,-3.44202241512147));
#50734=CARTESIAN_POINT('Ctrl Pts',(2.40537592959345,1.,-3.44127120683402));
#50735=CARTESIAN_POINT('Ctrl Pts',(2.40261515590099,1.,-3.43976627485223));
#50736=CARTESIAN_POINT('Ctrl Pts',(2.39848113411428,1.,-3.43750133066037));
#50737=CARTESIAN_POINT('Ctrl Pts',(2.39298338805823,1.,-3.43446630680436));
#50738=CARTESIAN_POINT('Ctrl Pts',(2.38613505844641,1.,-3.43064732714472));
#50739=CARTESIAN_POINT('Ctrl Pts',(2.37931067029517,1.,-3.42680309755241));
#50740=CARTESIAN_POINT('Ctrl Pts',(2.37251035954351,1.,-3.42293356216595));
#50741=CARTESIAN_POINT('Ctrl Pts',(2.36573431470313,1.,-3.41903866635384));
#50742=CARTESIAN_POINT('Ctrl Pts',(2.35898278606449,1.,-3.4151183675076));
#50743=CARTESIAN_POINT('Ctrl Pts',(2.35225606823649,1.,-3.41117262313464));
#50744=CARTESIAN_POINT('Ctrl Pts',(2.34555447648901,1.,-3.40720137403888));
#50745=CARTESIAN_POINT('Ctrl Pts',(2.33887832342715,1.,-3.40320452776646));
#50746=CARTESIAN_POINT('Ctrl Pts',(2.33222789882601,1.,-3.39918194578115));
#50747=CARTESIAN_POINT('Ctrl Pts',(2.32560343902683,1.,-3.39513342020045));
#50748=CARTESIAN_POINT('Ctrl Pts',(2.31900513925627,1.,-3.39105869475112));
#50749=CARTESIAN_POINT('Ctrl Pts',(2.31243319489505,1.,-3.38695751492659));
#50750=CARTESIAN_POINT('Ctrl Pts',(2.30588783640389,1.,-3.38282967336676));
#50751=CARTESIAN_POINT('Ctrl Pts',(2.29936936127588,1.,-3.37867504959382));
#50752=CARTESIAN_POINT('Ctrl Pts',(2.2928781800731,1.,-3.37449367172707));
#50753=CARTESIAN_POINT('Ctrl Pts',(2.28641481081045,1.,-3.37028570206357));
#50754=CARTESIAN_POINT('Ctrl Pts',(2.27997979457968,1.,-3.36605130712978));
#50755=CARTESIAN_POINT('Ctrl Pts',(2.27357362620902,1.,-3.36179055004369));
#50756=CARTESIAN_POINT('Ctrl Pts',(2.26719668579921,1.,-3.35750328523077));
#50757=CARTESIAN_POINT('Ctrl Pts',(2.26084915222484,1.,-3.35318902552676));
#50758=CARTESIAN_POINT('Ctrl Pts',(2.25453097693524,1.,-3.34884690292342));
#50759=CARTESIAN_POINT('Ctrl Pts',(2.24824207678287,1.,-3.34447596770768));
#50760=CARTESIAN_POINT('Ctrl Pts',(2.24198249391437,1.,-3.34007543738044));
#50761=CARTESIAN_POINT('Ctrl Pts',(2.23575256328809,1.,-3.33564495756478));
#50762=CARTESIAN_POINT('Ctrl Pts',(2.22955308907221,1.,-3.33118487773593));
#50763=CARTESIAN_POINT('Ctrl Pts',(2.22338548312758,1.,-3.32669646722871));
#50764=CARTESIAN_POINT('Ctrl Pts',(2.21725135110889,1.,-3.32218125618955));
#50765=CARTESIAN_POINT('Ctrl Pts',(2.21115211847872,1.,-3.31764044024231));
#50766=CARTESIAN_POINT('Ctrl Pts',(2.20508863150608,1.,-3.3130742460895));
#50767=CARTESIAN_POINT('Ctrl Pts',(2.19906078949924,1.,-3.30848134694597));
#50768=CARTESIAN_POINT('Ctrl Pts',(2.19306710376112,1.,-3.30385816281831));
#50769=CARTESIAN_POINT('Ctrl Pts',(2.18710556500325,1.,-3.29920022557635));
#50770=CARTESIAN_POINT('Ctrl Pts',(2.18117455557062,1.,-3.29450361500484));
#50771=CARTESIAN_POINT('Ctrl Pts',(2.17527380048422,1.,-3.28976645712566));
#50772=CARTESIAN_POINT('Ctrl Pts',(2.16940517773459,1.,-3.2849901997973));
#50773=CARTESIAN_POINT('Ctrl Pts',(2.16357391934434,1.,-3.28018150841414));
#50774=CARTESIAN_POINT('Ctrl Pts',(2.15778690038359,1.,-3.27534954469206));
#50775=CARTESIAN_POINT('Ctrl Pts',(2.15205043199818,1.,-3.27050245897244));
#50776=CARTESIAN_POINT('Ctrl Pts',(2.14636805295663,1.,-3.26564388189764));
#50777=CARTESIAN_POINT('Ctrl Pts',(2.14073870754257,1.,-3.26077002641868));
#50778=CARTESIAN_POINT('Ctrl Pts',(2.13515375878786,1.,-3.25586495065027));
#50779=CARTESIAN_POINT('Ctrl Pts',(2.1296002839681,1.,-3.25090574493994));
#50780=CARTESIAN_POINT('Ctrl Pts',(2.12406646410943,1.,-3.24587102613347));
#50781=CARTESIAN_POINT('Ctrl Pts',(2.11854673326972,1.,-3.24074905517282));
#50782=CARTESIAN_POINT('Ctrl Pts',(2.11304604021784,1.,-3.23554444767115));
#50783=CARTESIAN_POINT('Ctrl Pts',(2.1075869964248,1.,-3.23028945793334));
#50784=CARTESIAN_POINT('Ctrl Pts',(2.10220384298533,1.,-3.22503437553496));
#50785=CARTESIAN_POINT('Ctrl Pts',(2.09692958434933,1.,-3.21982707347067));
#50786=CARTESIAN_POINT('Ctrl Pts',(2.0917841946046,1.,-3.2146942960168));
#50787=CARTESIAN_POINT('Ctrl Pts',(2.08676465517435,1.,-3.20962575845433));
#50788=CARTESIAN_POINT('Ctrl Pts',(2.08182850370816,1.,-3.20454818630635));
#50789=CARTESIAN_POINT('Ctrl Pts',(2.0769044187063,1.,-3.19934132835879));
#50790=CARTESIAN_POINT('Ctrl Pts',(2.07192253497765,1.,-3.19388465568113));
#50791=CARTESIAN_POINT('Ctrl Pts',(2.06684062744065,1.,-3.18809755562297));
#50792=CARTESIAN_POINT('Ctrl Pts',(2.06166849827143,1.,-3.18197692964677));
#50793=CARTESIAN_POINT('Ctrl Pts',(2.05650186773279,1.,-3.17564906975592));
#50794=CARTESIAN_POINT('Ctrl Pts',(2.05151770247452,1.,-3.16936341689859));
#50795=CARTESIAN_POINT('Ctrl Pts',(2.0469333124766,1.,-3.16343165059235));
#50796=CARTESIAN_POINT('Ctrl Pts',(2.04297406404132,1.,-3.15817983946525));
#50797=CARTESIAN_POINT('Ctrl Pts',(2.03984073791432,1.,-3.1538999167466));
#50798=CARTESIAN_POINT('Ctrl Pts',(2.03783225496023,1.,-3.15102344775396));
#50799=CARTESIAN_POINT('Ctrl Pts',(2.03693188810614,1.,-3.14959882629936));
#50800=CARTESIAN_POINT('Ctrl Pts',(2.03663974554941,1.,-3.14901193669147));
#50801=CARTESIAN_POINT('Ctrl Pts',(2.03659701539175,1.,-3.1488193908823));
#50802=CARTESIAN_POINT('Ctrl Pts',(2.03660101169564,1.,-3.14877060440425));
#50803=CARTESIAN_POINT('',(2.40675750623143,0.,-3.44202241512147));
#50804=CARTESIAN_POINT('Ctrl Pts',(2.36523532225181,-1.,-2.91001063062876));
#50805=CARTESIAN_POINT('Ctrl Pts',(2.36523532225181,1.,-2.91001063062876));
#50806=CARTESIAN_POINT('Ctrl Pts',(2.36524348105112,-1.,-2.90992398626211));
#50807=CARTESIAN_POINT('Ctrl Pts',(2.36524348105112,1.,-2.90992398626211));
#50808=CARTESIAN_POINT('Ctrl Pts',(2.36535052956938,-1.,-2.90989022548032));
#50809=CARTESIAN_POINT('Ctrl Pts',(2.36535052956938,1.,-2.90989022548032));
#50810=CARTESIAN_POINT('Ctrl Pts',(2.36578327194741,-1.,-2.91025813830041));
#50811=CARTESIAN_POINT('Ctrl Pts',(2.36578327194741,1.,-2.91025813830041));
#50812=CARTESIAN_POINT('Ctrl Pts',(2.36690501170627,-1.,-2.9115863784204));
#50813=CARTESIAN_POINT('Ctrl Pts',(2.36690501170627,1.,-2.9115863784204));
#50814=CARTESIAN_POINT('Ctrl Pts',(2.36919161373173,-1.,-2.9146124988314));
#50815=CARTESIAN_POINT('Ctrl Pts',(2.36919161373173,1.,-2.9146124988314));
#50816=CARTESIAN_POINT('Ctrl Pts',(2.37229381109821,-1.,-2.91891503791411));
#50817=CARTESIAN_POINT('Ctrl Pts',(2.37229381109821,1.,-2.91891503791411));
#50818=CARTESIAN_POINT('Ctrl Pts',(2.3760651052403,-1.,-2.92430340582608));
#50819=CARTESIAN_POINT('Ctrl Pts',(2.3760651052403,1.,-2.92430340582608));
#50820=CARTESIAN_POINT('Ctrl Pts',(2.38028989582073,-1.,-2.93049643640206));
#50821=CARTESIAN_POINT('Ctrl Pts',(2.38028989582073,1.,-2.93049643640206));
#50822=CARTESIAN_POINT('Ctrl Pts',(2.38472771516311,-1.,-2.93717903280391));
#50823=CARTESIAN_POINT('Ctrl Pts',(2.38472771516311,1.,-2.93717903280391));
#50824=CARTESIAN_POINT('Ctrl Pts',(2.38914929090759,-1.,-2.94404820669076));
#50825=CARTESIAN_POINT('Ctrl Pts',(2.38914929090759,1.,-2.94404820669076));
#50826=CARTESIAN_POINT('Ctrl Pts',(2.39337207631667,-1.,-2.95085857128439));
#50827=CARTESIAN_POINT('Ctrl Pts',(2.39337207631667,1.,-2.95085857128439));
#50828=CARTESIAN_POINT('Ctrl Pts',(2.39730553974516,-1.,-2.95748006482942));
#50829=CARTESIAN_POINT('Ctrl Pts',(2.39730553974516,1.,-2.95748006482942));
#50830=CARTESIAN_POINT('Ctrl Pts',(2.4009556571164,-1.,-2.96390432240312));
#50831=CARTESIAN_POINT('Ctrl Pts',(2.4009556571164,1.,-2.96390432240312));
#50832=CARTESIAN_POINT('Ctrl Pts',(2.40438604734919,-1.,-2.9701964131236));
#50833=CARTESIAN_POINT('Ctrl Pts',(2.40438604734919,1.,-2.9701964131236));
#50834=CARTESIAN_POINT('Ctrl Pts',(2.40768975073713,-1.,-2.97646002822422));
#50835=CARTESIAN_POINT('Ctrl Pts',(2.40768975073713,1.,-2.97646002822422));
#50836=CARTESIAN_POINT('Ctrl Pts',(2.41095909342571,-1.,-2.98280015815107));
#50837=CARTESIAN_POINT('Ctrl Pts',(2.41095909342571,1.,-2.98280015815107));
#50838=CARTESIAN_POINT('Ctrl Pts',(2.41425064199586,-1.,-2.98927983005796));
#50839=CARTESIAN_POINT('Ctrl Pts',(2.41425064199586,1.,-2.98927983005796));
#50840=CARTESIAN_POINT('Ctrl Pts',(2.41757324500514,-1.,-2.99590509293503));
#50841=CARTESIAN_POINT('Ctrl Pts',(2.41757324500514,1.,-2.99590509293503));
#50842=CARTESIAN_POINT('Ctrl Pts',(2.42090763946779,-1.,-3.00264868585996));
#50843=CARTESIAN_POINT('Ctrl Pts',(2.42090763946779,1.,-3.00264868585996));
#50844=CARTESIAN_POINT('Ctrl Pts',(2.42421849439613,-1.,-3.00946442616659));
#50845=CARTESIAN_POINT('Ctrl Pts',(2.42421849439613,1.,-3.00946442616659));
#50846=CARTESIAN_POINT('Ctrl Pts',(2.42746856264168,-1.,-3.01630420830504));
#50847=CARTESIAN_POINT('Ctrl Pts',(2.42746856264168,1.,-3.01630420830504));
#50848=CARTESIAN_POINT('Ctrl Pts',(2.43063415586637,-1.,-3.02313656036004));
#50849=CARTESIAN_POINT('Ctrl Pts',(2.43063415586637,1.,-3.02313656036004));
#50850=CARTESIAN_POINT('Ctrl Pts',(2.43371241361488,-1.,-3.02995534946978));
#50851=CARTESIAN_POINT('Ctrl Pts',(2.43371241361488,1.,-3.02995534946978));
#50852=CARTESIAN_POINT('Ctrl Pts',(2.43671278042414,-1.,-3.03676949672822));
#50853=CARTESIAN_POINT('Ctrl Pts',(2.43671278042414,1.,-3.03676949672822));
#50854=CARTESIAN_POINT('Ctrl Pts',(2.43965194061857,-1.,-3.04359685040555));
#50855=CARTESIAN_POINT('Ctrl Pts',(2.43965194061857,1.,-3.04359685040555));
#50856=CARTESIAN_POINT('Ctrl Pts',(2.44254768923105,-1.,-3.05045678021504));
#50857=CARTESIAN_POINT('Ctrl Pts',(2.44254768923105,1.,-3.05045678021504));
#50858=CARTESIAN_POINT('Ctrl Pts',(2.44541251892556,-1.,-3.05736242671506));
#50859=CARTESIAN_POINT('Ctrl Pts',(2.44541251892556,1.,-3.05736242671506));
#50860=CARTESIAN_POINT('Ctrl Pts',(2.44824970516543,-1.,-3.06431596421405));
#50861=CARTESIAN_POINT('Ctrl Pts',(2.44824970516543,1.,-3.06431596421405));
#50862=CARTESIAN_POINT('Ctrl Pts',(2.45105688854422,-1.,-3.07131290521297));
#50863=CARTESIAN_POINT('Ctrl Pts',(2.45105688854422,1.,-3.07131290521297));
#50864=CARTESIAN_POINT('Ctrl Pts',(2.4538282678779,-1.,-3.07834472886139));
#50865=CARTESIAN_POINT('Ctrl Pts',(2.4538282678779,1.,-3.07834472886139));
#50866=CARTESIAN_POINT('Ctrl Pts',(2.45655725437039,-1.,-3.08540206545315));
#50867=CARTESIAN_POINT('Ctrl Pts',(2.45655725437039,1.,-3.08540206545315));
#50868=CARTESIAN_POINT('Ctrl Pts',(2.4592391256388,-1.,-3.09247787931887));
#50869=CARTESIAN_POINT('Ctrl Pts',(2.4592391256388,1.,-3.09247787931887));
#50870=CARTESIAN_POINT('Ctrl Pts',(2.46187308501884,-1.,-3.09956993697052));
#50871=CARTESIAN_POINT('Ctrl Pts',(2.46187308501884,1.,-3.09956993697052));
#50872=CARTESIAN_POINT('Ctrl Pts',(2.46446082979646,-1.,-3.1066790790198));
#50873=CARTESIAN_POINT('Ctrl Pts',(2.46446082979646,1.,-3.1066790790198));
#50874=CARTESIAN_POINT('Ctrl Pts',(2.46700558843506,-1.,-3.11380805536122));
#50875=CARTESIAN_POINT('Ctrl Pts',(2.46700558843506,1.,-3.11380805536122));
#50876=CARTESIAN_POINT('Ctrl Pts',(2.46951098947469,-1.,-3.12096015766983));
#50877=CARTESIAN_POINT('Ctrl Pts',(2.46951098947469,1.,-3.12096015766983));
#50878=CARTESIAN_POINT('Ctrl Pts',(2.47197997765871,-1.,-3.12813790805952));
#50879=CARTESIAN_POINT('Ctrl Pts',(2.47197997765871,1.,-3.12813790805952));
#50880=CARTESIAN_POINT('Ctrl Pts',(2.47441378371932,-1.,-3.13534181229295));
#50881=CARTESIAN_POINT('Ctrl Pts',(2.47441378371932,1.,-3.13534181229295));
#50882=CARTESIAN_POINT('Ctrl Pts',(2.47681245356109,-1.,-3.1425709954655));
#50883=CARTESIAN_POINT('Ctrl Pts',(2.47681245356109,1.,-3.1425709954655));
#50884=CARTESIAN_POINT('Ctrl Pts',(2.47917529057029,-1.,-3.14982373241352));
#50885=CARTESIAN_POINT('Ctrl Pts',(2.47917529057029,1.,-3.14982373241352));
#50886=CARTESIAN_POINT('Ctrl Pts',(2.48150133566571,-1.,-3.15709802322739));
#50887=CARTESIAN_POINT('Ctrl Pts',(2.48150133566571,1.,-3.15709802322739));
#50888=CARTESIAN_POINT('Ctrl Pts',(2.48378981792725,-1.,-3.16439213290161));
#50889=CARTESIAN_POINT('Ctrl Pts',(2.48378981792725,1.,-3.16439213290161));
#50890=CARTESIAN_POINT('Ctrl Pts',(2.48604065348587,-1.,-3.17170518863313));
#50891=CARTESIAN_POINT('Ctrl Pts',(2.48604065348587,1.,-3.17170518863313));
#50892=CARTESIAN_POINT('Ctrl Pts',(2.48825428288201,-1.,-3.17903698136622));
#50893=CARTESIAN_POINT('Ctrl Pts',(2.48825428288201,1.,-3.17903698136622));
#50894=CARTESIAN_POINT('Ctrl Pts',(2.49043146334059,-1.,-3.18638771282266));
#50895=CARTESIAN_POINT('Ctrl Pts',(2.49043146334059,1.,-3.18638771282266));
#50896=CARTESIAN_POINT('Ctrl Pts',(2.49257307239848,-1.,-3.19375775555798));
#50897=CARTESIAN_POINT('Ctrl Pts',(2.49257307239848,1.,-3.19375775555798));
#50898=CARTESIAN_POINT('Ctrl Pts',(2.49467992057755,-1.,-3.20114742397588));
#50899=CARTESIAN_POINT('Ctrl Pts',(2.49467992057755,1.,-3.20114742397588));
#50900=CARTESIAN_POINT('Ctrl Pts',(2.4967525264737,-1.,-3.20855669849836));
#50901=CARTESIAN_POINT('Ctrl Pts',(2.4967525264737,1.,-3.20855669849836));
#50902=CARTESIAN_POINT('Ctrl Pts',(2.4987911459939,-1.,-3.21598526261286));
#50903=CARTESIAN_POINT('Ctrl Pts',(2.4987911459939,1.,-3.21598526261286));
#50904=CARTESIAN_POINT('Ctrl Pts',(2.50079587201957,-1.,-3.22343262620503));
#50905=CARTESIAN_POINT('Ctrl Pts',(2.50079587201957,1.,-3.22343262620503));
#50906=CARTESIAN_POINT('Ctrl Pts',(2.50276671338111,-1.,-3.23089822320646));
#50907=CARTESIAN_POINT('Ctrl Pts',(2.50276671338111,1.,-3.23089822320646));
#50908=CARTESIAN_POINT('Ctrl Pts',(2.5047036758003,-1.,-3.23838151080319));
#50909=CARTESIAN_POINT('Ctrl Pts',(2.5047036758003,1.,-3.23838151080319));
#50910=CARTESIAN_POINT('Ctrl Pts',(2.506606859405,-1.,-3.24588208983849));
#50911=CARTESIAN_POINT('Ctrl Pts',(2.506606859405,1.,-3.24588208983849));
#50912=CARTESIAN_POINT('Ctrl Pts',(2.50847647070723,-1.,-3.25339971460982));
#50913=CARTESIAN_POINT('Ctrl Pts',(2.50847647070723,1.,-3.25339971460982));
#50914=CARTESIAN_POINT('Ctrl Pts',(2.51031277813486,-1.,-3.26093423001434));
#50915=CARTESIAN_POINT('Ctrl Pts',(2.51031277813486,1.,-3.26093423001434));
#50916=CARTESIAN_POINT('Ctrl Pts',(2.51211608411423,-1.,-3.26848552888116));
#50917=CARTESIAN_POINT('Ctrl Pts',(2.51211608411423,1.,-3.26848552888116));
#50918=CARTESIAN_POINT('Ctrl Pts',(2.513886692704,-1.,-3.27605350473142));
#50919=CARTESIAN_POINT('Ctrl Pts',(2.513886692704,1.,-3.27605350473142));
#50920=CARTESIAN_POINT('Ctrl Pts',(2.51562487464514,-1.,-3.28363799702982));
#50921=CARTESIAN_POINT('Ctrl Pts',(2.51562487464514,1.,-3.28363799702982));
#50922=CARTESIAN_POINT('Ctrl Pts',(2.51733085123797,-1.,-3.2912387729927));
#50923=CARTESIAN_POINT('Ctrl Pts',(2.51733085123797,1.,-3.2912387729927));
#50924=CARTESIAN_POINT('Ctrl Pts',(2.51900480701068,-1.,-3.29885556388353));
#50925=CARTESIAN_POINT('Ctrl Pts',(2.51900480701068,1.,-3.29885556388353));
#50926=CARTESIAN_POINT('Ctrl Pts',(2.52064689568511,-1.,-3.30648808815443));
#50927=CARTESIAN_POINT('Ctrl Pts',(2.52064689568511,1.,-3.30648808815443));
#50928=CARTESIAN_POINT('Ctrl Pts',(2.52225724871313,-1.,-3.31413607874645));
#50929=CARTESIAN_POINT('Ctrl Pts',(2.52225724871313,1.,-3.31413607874645));
#50930=CARTESIAN_POINT('Ctrl Pts',(2.5238359839626,-1.,-3.32179931078699));
#50931=CARTESIAN_POINT('Ctrl Pts',(2.5238359839626,1.,-3.32179931078699));
#50932=CARTESIAN_POINT('Ctrl Pts',(2.52538321164634,-1.,-3.32947762187533));
#50933=CARTESIAN_POINT('Ctrl Pts',(2.52538321164634,1.,-3.32947762187533));
#50934=CARTESIAN_POINT('Ctrl Pts',(2.52689902690158,-1.,-3.33717089999103));
#50935=CARTESIAN_POINT('Ctrl Pts',(2.52689902690158,1.,-3.33717089999103));
#50936=CARTESIAN_POINT('Ctrl Pts',(2.52808660915689,-1.,-3.34333744115511));
#50937=CARTESIAN_POINT('Ctrl Pts',(2.52808660915689,1.,-3.34333744115511));
#50938=CARTESIAN_POINT('Ctrl Pts',(2.52896321610703,-1.,-3.34796903576663));
#50939=CARTESIAN_POINT('Ctrl Pts',(2.52896321610703,1.,-3.34796903576663));
#50940=CARTESIAN_POINT('Ctrl Pts',(2.5295413654909,-1.,-3.35105973714072));
#50941=CARTESIAN_POINT('Ctrl Pts',(2.5295413654909,1.,-3.35105973714072));
#50942=CARTESIAN_POINT('Ctrl Pts',(2.52982887637028,-1.,-3.35260583073571));
#50943=CARTESIAN_POINT('Ctrl Pts',(2.52982887637028,1.,-3.35260583073571));
#50944=CARTESIAN_POINT('',(2.36531447826073,1.,-2.90994629141676));
#50945=CARTESIAN_POINT('Ctrl Pts',(2.36531447826073,-1.,-2.90994629141676));
#50946=CARTESIAN_POINT('Ctrl Pts',(2.36531447826073,-0.666666666666667,
-2.90994629141676));
#50947=CARTESIAN_POINT('Ctrl Pts',(2.36531447826073,-0.333333333333333,
-2.90994629141676));
#50948=CARTESIAN_POINT('Ctrl Pts',(2.36531447826073,0.333333333333333,-2.90994629141676));
#50949=CARTESIAN_POINT('Ctrl Pts',(2.36531447826074,0.666666666666667,-2.90994629141676));
#50950=CARTESIAN_POINT('Ctrl Pts',(2.36531447826074,1.,-2.90994629141676));
#50951=CARTESIAN_POINT('',(2.52982887637028,1.,-3.35260583073571));
#50952=CARTESIAN_POINT('',(2.52982887637028,0.,-3.35260583073571));
#50953=CARTESIAN_POINT('Ctrl Pts',(2.36531447826073,1.,-2.90994629141676));
#50954=CARTESIAN_POINT('Ctrl Pts',(2.36536211188453,1.,-2.90995756655606));
#50955=CARTESIAN_POINT('Ctrl Pts',(2.36553202948613,1.,-2.91005770527719));
#50956=CARTESIAN_POINT('Ctrl Pts',(2.36599991765749,1.,-2.91051690822156));
#50957=CARTESIAN_POINT('Ctrl Pts',(2.36707658451664,1.,-2.91181344022548));
#50958=CARTESIAN_POINT('Ctrl Pts',(2.36919161373173,1.,-2.9146124988314));
#50959=CARTESIAN_POINT('Ctrl Pts',(2.37229381109821,1.,-2.91891503791411));
#50960=CARTESIAN_POINT('Ctrl Pts',(2.3760651052403,1.,-2.92430340582608));
#50961=CARTESIAN_POINT('Ctrl Pts',(2.38028989582073,1.,-2.93049643640206));
#50962=CARTESIAN_POINT('Ctrl Pts',(2.38472771516311,1.,-2.93717903280391));
#50963=CARTESIAN_POINT('Ctrl Pts',(2.38914929090759,1.,-2.94404820669076));
#50964=CARTESIAN_POINT('Ctrl Pts',(2.39337207631667,1.,-2.95085857128439));
#50965=CARTESIAN_POINT('Ctrl Pts',(2.39730553974516,1.,-2.95748006482942));
#50966=CARTESIAN_POINT('Ctrl Pts',(2.4009556571164,1.,-2.96390432240312));
#50967=CARTESIAN_POINT('Ctrl Pts',(2.40438604734919,1.,-2.9701964131236));
#50968=CARTESIAN_POINT('Ctrl Pts',(2.40768975073713,1.,-2.97646002822422));
#50969=CARTESIAN_POINT('Ctrl Pts',(2.41095909342571,1.,-2.98280015815107));
#50970=CARTESIAN_POINT('Ctrl Pts',(2.41425064199586,1.,-2.98927983005796));
#50971=CARTESIAN_POINT('Ctrl Pts',(2.41757324500514,1.,-2.99590509293503));
#50972=CARTESIAN_POINT('Ctrl Pts',(2.42090763946779,1.,-3.00264868585996));
#50973=CARTESIAN_POINT('Ctrl Pts',(2.42421849439613,1.,-3.00946442616659));
#50974=CARTESIAN_POINT('Ctrl Pts',(2.42746856264168,1.,-3.01630420830504));
#50975=CARTESIAN_POINT('Ctrl Pts',(2.43063415586637,1.,-3.02313656036004));
#50976=CARTESIAN_POINT('Ctrl Pts',(2.43371241361488,1.,-3.02995534946978));
#50977=CARTESIAN_POINT('Ctrl Pts',(2.43671278042414,1.,-3.03676949672822));
#50978=CARTESIAN_POINT('Ctrl Pts',(2.43965194061857,1.,-3.04359685040555));
#50979=CARTESIAN_POINT('Ctrl Pts',(2.44254768923105,1.,-3.05045678021504));
#50980=CARTESIAN_POINT('Ctrl Pts',(2.44541251892556,1.,-3.05736242671506));
#50981=CARTESIAN_POINT('Ctrl Pts',(2.44824970516543,1.,-3.06431596421405));
#50982=CARTESIAN_POINT('Ctrl Pts',(2.45105688854422,1.,-3.07131290521297));
#50983=CARTESIAN_POINT('Ctrl Pts',(2.4538282678779,1.,-3.07834472886139));
#50984=CARTESIAN_POINT('Ctrl Pts',(2.45655725437039,1.,-3.08540206545315));
#50985=CARTESIAN_POINT('Ctrl Pts',(2.4592391256388,1.,-3.09247787931887));
#50986=CARTESIAN_POINT('Ctrl Pts',(2.46187308501884,1.,-3.09956993697052));
#50987=CARTESIAN_POINT('Ctrl Pts',(2.46446082979646,1.,-3.1066790790198));
#50988=CARTESIAN_POINT('Ctrl Pts',(2.46700558843506,1.,-3.11380805536122));
#50989=CARTESIAN_POINT('Ctrl Pts',(2.46951098947469,1.,-3.12096015766983));
#50990=CARTESIAN_POINT('Ctrl Pts',(2.47197997765871,1.,-3.12813790805952));
#50991=CARTESIAN_POINT('Ctrl Pts',(2.47441378371932,1.,-3.13534181229295));
#50992=CARTESIAN_POINT('Ctrl Pts',(2.47681245356109,1.,-3.1425709954655));
#50993=CARTESIAN_POINT('Ctrl Pts',(2.47917529057029,1.,-3.14982373241352));
#50994=CARTESIAN_POINT('Ctrl Pts',(2.48150133566571,1.,-3.15709802322739));
#50995=CARTESIAN_POINT('Ctrl Pts',(2.48378981792725,1.,-3.16439213290161));
#50996=CARTESIAN_POINT('Ctrl Pts',(2.48604065348587,1.,-3.17170518863313));
#50997=CARTESIAN_POINT('Ctrl Pts',(2.48825428288201,1.,-3.17903698136622));
#50998=CARTESIAN_POINT('Ctrl Pts',(2.49043146334059,1.,-3.18638771282266));
#50999=CARTESIAN_POINT('Ctrl Pts',(2.49257307239848,1.,-3.19375775555798));
#51000=CARTESIAN_POINT('Ctrl Pts',(2.49467992057755,1.,-3.20114742397588));
#51001=CARTESIAN_POINT('Ctrl Pts',(2.4967525264737,1.,-3.20855669849836));
#51002=CARTESIAN_POINT('Ctrl Pts',(2.4987911459939,1.,-3.21598526261286));
#51003=CARTESIAN_POINT('Ctrl Pts',(2.50079587201957,1.,-3.22343262620503));
#51004=CARTESIAN_POINT('Ctrl Pts',(2.50276671338111,1.,-3.23089822320646));
#51005=CARTESIAN_POINT('Ctrl Pts',(2.5047036758003,1.,-3.23838151080319));
#51006=CARTESIAN_POINT('Ctrl Pts',(2.506606859405,1.,-3.24588208983849));
#51007=CARTESIAN_POINT('Ctrl Pts',(2.50847647070723,1.,-3.25339971460982));
#51008=CARTESIAN_POINT('Ctrl Pts',(2.51031277813486,1.,-3.26093423001434));
#51009=CARTESIAN_POINT('Ctrl Pts',(2.51211608411423,1.,-3.26848552888116));
#51010=CARTESIAN_POINT('Ctrl Pts',(2.513886692704,1.,-3.27605350473142));
#51011=CARTESIAN_POINT('Ctrl Pts',(2.51562487464514,1.,-3.28363799702982));
#51012=CARTESIAN_POINT('Ctrl Pts',(2.51733085123797,1.,-3.2912387729927));
#51013=CARTESIAN_POINT('Ctrl Pts',(2.51900480701068,1.,-3.29885556388353));
#51014=CARTESIAN_POINT('Ctrl Pts',(2.52064689568511,1.,-3.30648808815443));
#51015=CARTESIAN_POINT('Ctrl Pts',(2.52225724871313,1.,-3.31413607874645));
#51016=CARTESIAN_POINT('Ctrl Pts',(2.5238359839626,1.,-3.32179931078699));
#51017=CARTESIAN_POINT('Ctrl Pts',(2.52538321164634,1.,-3.32947762187533));
#51018=CARTESIAN_POINT('Ctrl Pts',(2.52689902690158,1.,-3.33717089999103));
#51019=CARTESIAN_POINT('Ctrl Pts',(2.52808660915689,1.,-3.34333744115511));
#51020=CARTESIAN_POINT('Ctrl Pts',(2.52896321610703,1.,-3.34796903576663));
#51021=CARTESIAN_POINT('Ctrl Pts',(2.5295413654909,1.,-3.35105973714072));
#51022=CARTESIAN_POINT('Ctrl Pts',(2.52982887637028,1.,-3.35260583073571));
#51023=CARTESIAN_POINT('Origin',(2.52982887637028,0.,-3.35260583073571));
#51024=CARTESIAN_POINT('',(2.40675750623143,1.,-3.44202241512147));
#51025=CARTESIAN_POINT('Origin',(0.,0.,0.));
#51026=CARTESIAN_POINT('',(2.50410331873042,1.,-2.79140942341378));
#51027=CARTESIAN_POINT('Origin',(0.,1.,0.));
#51028=CARTESIAN_POINT('Ctrl Pts',(2.50410331873042,1.,-2.79140942341378));
#51029=CARTESIAN_POINT('Ctrl Pts',(2.50410331873042,0.666666666666667,-2.79140942341378));
#51030=CARTESIAN_POINT('Ctrl Pts',(2.50410331873042,0.333333333333333,-2.79140942341378));
#51031=CARTESIAN_POINT('Ctrl Pts',(2.50410331873042,-0.333333333333333,
-2.79140942341378));
#51032=CARTESIAN_POINT('Ctrl Pts',(2.50410331873042,-0.666666666666667,
-2.79140942341378));
#51033=CARTESIAN_POINT('Ctrl Pts',(2.50410331873042,-1.,-2.79140942341378));
#51034=CARTESIAN_POINT('Ctrl Pts',(2.91557726271063,-1.,-3.02314558451372));
#51035=CARTESIAN_POINT('Ctrl Pts',(2.91557726271063,1.,-3.02314558451372));
#51036=CARTESIAN_POINT('Ctrl Pts',(2.91409518070707,-1.,-3.02261975104912));
#51037=CARTESIAN_POINT('Ctrl Pts',(2.91409518070707,1.,-3.02261975104912));
#51038=CARTESIAN_POINT('Ctrl Pts',(2.91113297349052,-1.,-3.02156522743299));
#51039=CARTESIAN_POINT('Ctrl Pts',(2.91113297349052,1.,-3.02156522743299));
#51040=CARTESIAN_POINT('Ctrl Pts',(2.90669553303902,-1.,-3.01997487194926));
#51041=CARTESIAN_POINT('Ctrl Pts',(2.90669553303902,1.,-3.01997487194926));
#51042=CARTESIAN_POINT('Ctrl Pts',(2.90079069102661,-1.,-3.01783725123646));
#51043=CARTESIAN_POINT('Ctrl Pts',(2.90079069102661,1.,-3.01783725123646));
#51044=CARTESIAN_POINT('Ctrl Pts',(2.8934292556764,-1.,-3.01513660433291));
#51045=CARTESIAN_POINT('Ctrl Pts',(2.8934292556764,1.,-3.01513660433291));
#51046=CARTESIAN_POINT('Ctrl Pts',(2.88608751706796,-1.,-3.01240727309568));
#51047=CARTESIAN_POINT('Ctrl Pts',(2.88608751706796,1.,-3.01240727309568));
#51048=CARTESIAN_POINT('Ctrl Pts',(2.87876560072799,-1.,-3.0096491810855));
#51049=CARTESIAN_POINT('Ctrl Pts',(2.87876560072799,1.,-3.0096491810855));
#51050=CARTESIAN_POINT('Ctrl Pts',(2.87146368430104,-1.,-3.00686224485374));
#51051=CARTESIAN_POINT('Ctrl Pts',(2.87146368430104,1.,-3.00686224485374));
#51052=CARTESIAN_POINT('Ctrl Pts',(2.86418200833065,-1.,-3.00404638316245));
#51053=CARTESIAN_POINT('Ctrl Pts',(2.86418200833065,1.,-3.00404638316245));
#51054=CARTESIAN_POINT('Ctrl Pts',(2.85692085715129,-1.,-3.0012015079552));
#51055=CARTESIAN_POINT('Ctrl Pts',(2.85692085715129,1.,-3.0012015079552));
#51056=CARTESIAN_POINT('Ctrl Pts',(2.84968053289104,-1.,-2.99832751144566));
#51057=CARTESIAN_POINT('Ctrl Pts',(2.84968053289104,1.,-2.99832751144566));
#51058=CARTESIAN_POINT('Ctrl Pts',(2.84246132984334,-1.,-2.995424253416));
#51059=CARTESIAN_POINT('Ctrl Pts',(2.84246132984334,1.,-2.995424253416));
#51060=CARTESIAN_POINT('Ctrl Pts',(2.83526351254383,-1.,-2.99249155170479));
#51061=CARTESIAN_POINT('Ctrl Pts',(2.83526351254383,1.,-2.99249155170479));
#51062=CARTESIAN_POINT('Ctrl Pts',(2.82808728190402,-1.,-2.98952916401699));
#51063=CARTESIAN_POINT('Ctrl Pts',(2.82808728190402,1.,-2.98952916401699));
#51064=CARTESIAN_POINT('Ctrl Pts',(2.82093279065704,-1.,-2.98653680669434));
#51065=CARTESIAN_POINT('Ctrl Pts',(2.82093279065704,1.,-2.98653680669434));
#51066=CARTESIAN_POINT('Ctrl Pts',(2.81380019196454,-1.,-2.9835141977994));
#51067=CARTESIAN_POINT('Ctrl Pts',(2.81380019196454,1.,-2.9835141977994));
#51068=CARTESIAN_POINT('Ctrl Pts',(2.80668968101162,-1.,-2.98046109647299));
#51069=CARTESIAN_POINT('Ctrl Pts',(2.80668968101162,1.,-2.98046109647299));
#51070=CARTESIAN_POINT('Ctrl Pts',(2.79960153278186,-1.,-2.97737733718242));
#51071=CARTESIAN_POINT('Ctrl Pts',(2.79960153278186,1.,-2.97737733718242));
#51072=CARTESIAN_POINT('Ctrl Pts',(2.79253615718147,-1.,-2.97426288347475));
#51073=CARTESIAN_POINT('Ctrl Pts',(2.79253615718147,1.,-2.97426288347475));
#51074=CARTESIAN_POINT('Ctrl Pts',(2.78549409123657,-1.,-2.97111781461349));
#51075=CARTESIAN_POINT('Ctrl Pts',(2.78549409123657,1.,-2.97111781461349));
#51076=CARTESIAN_POINT('Ctrl Pts',(2.77847589542767,-1.,-2.9679422104295));
#51077=CARTESIAN_POINT('Ctrl Pts',(2.77847589542767,1.,-2.9679422104295));
#51078=CARTESIAN_POINT('Ctrl Pts',(2.77148206836464,-1.,-2.96473605585548));
#51079=CARTESIAN_POINT('Ctrl Pts',(2.77148206836464,1.,-2.96473605585548));
#51080=CARTESIAN_POINT('Ctrl Pts',(2.76451296269571,-1.,-2.96149914764832));
#51081=CARTESIAN_POINT('Ctrl Pts',(2.76451296269571,1.,-2.96149914764832));
#51082=CARTESIAN_POINT('Ctrl Pts',(2.75756867888393,-1.,-2.9582309766594));
#51083=CARTESIAN_POINT('Ctrl Pts',(2.75756867888393,1.,-2.9582309766594));
#51084=CARTESIAN_POINT('Ctrl Pts',(2.75064903318996,-1.,-2.95493069316211));
#51085=CARTESIAN_POINT('Ctrl Pts',(2.75064903318996,1.,-2.95493069316211));
#51086=CARTESIAN_POINT('Ctrl Pts',(2.7437537949221,-1.,-2.95159737214305));
#51087=CARTESIAN_POINT('Ctrl Pts',(2.7437537949221,1.,-2.95159737214305));
#51088=CARTESIAN_POINT('Ctrl Pts',(2.73688288329825,-1.,-2.94823023414381));
#51089=CARTESIAN_POINT('Ctrl Pts',(2.73688288329825,1.,-2.94823023414381));
#51090=CARTESIAN_POINT('Ctrl Pts',(2.73003657371613,-1.,-2.94482887675139));
#51091=CARTESIAN_POINT('Ctrl Pts',(2.73003657371613,1.,-2.94482887675139));
#51092=CARTESIAN_POINT('Ctrl Pts',(2.72321571511322,-1.,-2.94139351933882));
#51093=CARTESIAN_POINT('Ctrl Pts',(2.72321571511322,1.,-2.94139351933882));
#51094=CARTESIAN_POINT('Ctrl Pts',(2.71642190053575,-1.,-2.93792519474955));
#51095=CARTESIAN_POINT('Ctrl Pts',(2.71642190053575,1.,-2.93792519474955));
#51096=CARTESIAN_POINT('Ctrl Pts',(2.70965695523776,-1.,-2.93442516311168));
#51097=CARTESIAN_POINT('Ctrl Pts',(2.70965695523776,1.,-2.93442516311168));
#51098=CARTESIAN_POINT('Ctrl Pts',(2.70292247416881,-1.,-2.93089438233746));
#51099=CARTESIAN_POINT('Ctrl Pts',(2.70292247416881,1.,-2.93089438233746));
#51100=CARTESIAN_POINT('Ctrl Pts',(2.69621932864302,-1.,-2.92733294395268));
#51101=CARTESIAN_POINT('Ctrl Pts',(2.69621932864302,1.,-2.92733294395268));
#51102=CARTESIAN_POINT('Ctrl Pts',(2.68954721165342,-1.,-2.92373955325876));
#51103=CARTESIAN_POINT('Ctrl Pts',(2.68954721165342,1.,-2.92373955325876));
#51104=CARTESIAN_POINT('Ctrl Pts',(2.68290409279689,-1.,-2.92011090722152));
#51105=CARTESIAN_POINT('Ctrl Pts',(2.68290409279689,1.,-2.92011090722152));
#51106=CARTESIAN_POINT('Ctrl Pts',(2.67628728855309,-1.,-2.91644290704281));
#51107=CARTESIAN_POINT('Ctrl Pts',(2.67628728855309,1.,-2.91644290704281));
#51108=CARTESIAN_POINT('Ctrl Pts',(2.66969458792627,-1.,-2.91273193382876));
#51109=CARTESIAN_POINT('Ctrl Pts',(2.66969458792627,1.,-2.91273193382876));
#51110=CARTESIAN_POINT('Ctrl Pts',(2.66312542616808,-1.,-2.90897617968921));
#51111=CARTESIAN_POINT('Ctrl Pts',(2.66312542616808,1.,-2.90897617968921));
#51112=CARTESIAN_POINT('Ctrl Pts',(2.65658188464287,-1.,-2.90517678087467));
#51113=CARTESIAN_POINT('Ctrl Pts',(2.65658188464287,1.,-2.90517678087467));
#51114=CARTESIAN_POINT('Ctrl Pts',(2.65007017365576,-1.,-2.90133950224879));
#51115=CARTESIAN_POINT('Ctrl Pts',(2.65007017365576,1.,-2.90133950224879));
#51116=CARTESIAN_POINT('Ctrl Pts',(2.64359851684146,-1.,-2.89747231723361));
#51117=CARTESIAN_POINT('Ctrl Pts',(2.64359851684146,1.,-2.89747231723361));
#51118=CARTESIAN_POINT('Ctrl Pts',(2.63717442263944,-1.,-2.89358228854557));
#51119=CARTESIAN_POINT('Ctrl Pts',(2.63717442263944,1.,-2.89358228854557));
#51120=CARTESIAN_POINT('Ctrl Pts',(2.63080195420771,-1.,-2.88967244854243));
#51121=CARTESIAN_POINT('Ctrl Pts',(2.63080195420771,1.,-2.88967244854243));
#51122=CARTESIAN_POINT('Ctrl Pts',(2.62447947640253,-1.,-2.88573922195049));
#51123=CARTESIAN_POINT('Ctrl Pts',(2.62447947640253,1.,-2.88573922195049));
#51124=CARTESIAN_POINT('Ctrl Pts',(2.61819596473087,-1.,-2.88176821427502));
#51125=CARTESIAN_POINT('Ctrl Pts',(2.61819596473087,1.,-2.88176821427502));
#51126=CARTESIAN_POINT('Ctrl Pts',(2.61193507170928,-1.,-2.87773881947885));
#51127=CARTESIAN_POINT('Ctrl Pts',(2.61193507170928,1.,-2.87773881947885));
#51128=CARTESIAN_POINT('Ctrl Pts',(2.6056817788128,-1.,-2.87363176656475));
#51129=CARTESIAN_POINT('Ctrl Pts',(2.6056817788128,1.,-2.87363176656475));
#51130=CARTESIAN_POINT('Ctrl Pts',(2.59942875223202,-1.,-2.86943633170712));
#51131=CARTESIAN_POINT('Ctrl Pts',(2.59942875223202,1.,-2.86943633170712));
#51132=CARTESIAN_POINT('Ctrl Pts',(2.59318160184921,-1.,-2.86515629953528));
#51133=CARTESIAN_POINT('Ctrl Pts',(2.59318160184921,1.,-2.86515629953528));
#51134=CARTESIAN_POINT('Ctrl Pts',(2.5869677064356,-1.,-2.86081999003668));
#51135=CARTESIAN_POINT('Ctrl Pts',(2.5869677064356,1.,-2.86081999003668));
#51136=CARTESIAN_POINT('Ctrl Pts',(2.58082875254407,-1.,-2.85647171715147));
#51137=CARTESIAN_POINT('Ctrl Pts',(2.58082875254407,1.,-2.85647171715147));
#51138=CARTESIAN_POINT('Ctrl Pts',(2.57480482727128,-1.,-2.85215360144483));
#51139=CARTESIAN_POINT('Ctrl Pts',(2.57480482727128,1.,-2.85215360144483));
#51140=CARTESIAN_POINT('Ctrl Pts',(2.56891984251743,-1.,-2.84788893329091));
#51141=CARTESIAN_POINT('Ctrl Pts',(2.56891984251743,1.,-2.84788893329091));
#51142=CARTESIAN_POINT('Ctrl Pts',(2.56316920798489,-1.,-2.84366802680211));
#51143=CARTESIAN_POINT('Ctrl Pts',(2.56316920798489,1.,-2.84366802680211));
#51144=CARTESIAN_POINT('Ctrl Pts',(2.55749952145165,-1.,-2.83942515220699));
#51145=CARTESIAN_POINT('Ctrl Pts',(2.55749952145165,1.,-2.83942515220699));
#51146=CARTESIAN_POINT('Ctrl Pts',(2.55182152806964,-1.,-2.83505269592412));
#51147=CARTESIAN_POINT('Ctrl Pts',(2.55182152806964,1.,-2.83505269592412));
#51148=CARTESIAN_POINT('Ctrl Pts',(2.54604736792542,-1.,-2.83044254225794));
#51149=CARTESIAN_POINT('Ctrl Pts',(2.54604736792542,1.,-2.83044254225794));
#51150=CARTESIAN_POINT('Ctrl Pts',(2.54012272520141,-1.,-2.82552167649157));
#51151=CARTESIAN_POINT('Ctrl Pts',(2.54012272520141,1.,-2.82552167649157));
#51152=CARTESIAN_POINT('Ctrl Pts',(2.53405679667463,-1.,-2.82028550483744));
#51153=CARTESIAN_POINT('Ctrl Pts',(2.53405679667463,1.,-2.82028550483744));
#51154=CARTESIAN_POINT('Ctrl Pts',(2.52796388055457,-1.,-2.8148437904867));
#51155=CARTESIAN_POINT('Ctrl Pts',(2.52796388055457,1.,-2.8148437904867));
#51156=CARTESIAN_POINT('Ctrl Pts',(2.52205778589922,-1.,-2.80941521967234));
#51157=CARTESIAN_POINT('Ctrl Pts',(2.52205778589922,1.,-2.80941521967234));
#51158=CARTESIAN_POINT('Ctrl Pts',(2.51660190466067,-1.,-2.80427363984939));
#51159=CARTESIAN_POINT('Ctrl Pts',(2.51660190466067,1.,-2.80427363984939));
#51160=CARTESIAN_POINT('Ctrl Pts',(2.51186983687947,-1.,-2.79970585014308));
#51161=CARTESIAN_POINT('Ctrl Pts',(2.51186983687947,1.,-2.79970585014308));
#51162=CARTESIAN_POINT('Ctrl Pts',(2.50810555977564,-1.,-2.7959687805717));
#51163=CARTESIAN_POINT('Ctrl Pts',(2.50810555977564,1.,-2.7959687805717));
#51164=CARTESIAN_POINT('Ctrl Pts',(2.50547439929077,-1.,-2.79323694088143));
#51165=CARTESIAN_POINT('Ctrl Pts',(2.50547439929077,1.,-2.79323694088143));
#51166=CARTESIAN_POINT('Ctrl Pts',(2.50433799076945,-1.,-2.79192122906739));
#51167=CARTESIAN_POINT('Ctrl Pts',(2.50433799076945,1.,-2.79192122906739));
#51168=CARTESIAN_POINT('Ctrl Pts',(2.50404230339032,-1.,-2.79143626022225));
#51169=CARTESIAN_POINT('Ctrl Pts',(2.50404230339032,1.,-2.79143626022225));
#51170=CARTESIAN_POINT('Ctrl Pts',(2.50409239460011,-1.,-2.79133581100044));
#51171=CARTESIAN_POINT('Ctrl Pts',(2.50409239460011,1.,-2.79133581100044));
#51172=CARTESIAN_POINT('Ctrl Pts',(2.50417924854921,-1.,-2.79134130681569));
#51173=CARTESIAN_POINT('Ctrl Pts',(2.50417924854921,1.,-2.79134130681569));
#51174=CARTESIAN_POINT('',(2.91557726271063,1.,-3.02314558451372));
#51175=CARTESIAN_POINT('Ctrl Pts',(2.91557726271063,1.,-3.02314558451372));
#51176=CARTESIAN_POINT('Ctrl Pts',(2.91409518070707,1.,-3.02261975104912));
#51177=CARTESIAN_POINT('Ctrl Pts',(2.91113297349052,1.,-3.02156522743299));
#51178=CARTESIAN_POINT('Ctrl Pts',(2.90669553303902,1.,-3.01997487194926));
#51179=CARTESIAN_POINT('Ctrl Pts',(2.90079069102661,1.,-3.01783725123646));
#51180=CARTESIAN_POINT('Ctrl Pts',(2.8934292556764,1.,-3.01513660433291));
#51181=CARTESIAN_POINT('Ctrl Pts',(2.88608751706796,1.,-3.01240727309568));
#51182=CARTESIAN_POINT('Ctrl Pts',(2.87876560072799,1.,-3.0096491810855));
#51183=CARTESIAN_POINT('Ctrl Pts',(2.87146368430104,1.,-3.00686224485374));
#51184=CARTESIAN_POINT('Ctrl Pts',(2.86418200833065,1.,-3.00404638316245));
#51185=CARTESIAN_POINT('Ctrl Pts',(2.85692085715129,1.,-3.0012015079552));
#51186=CARTESIAN_POINT('Ctrl Pts',(2.84968053289104,1.,-2.99832751144566));
#51187=CARTESIAN_POINT('Ctrl Pts',(2.84246132984334,1.,-2.995424253416));
#51188=CARTESIAN_POINT('Ctrl Pts',(2.83526351254383,1.,-2.99249155170479));
#51189=CARTESIAN_POINT('Ctrl Pts',(2.82808728190402,1.,-2.98952916401699));
#51190=CARTESIAN_POINT('Ctrl Pts',(2.82093279065704,1.,-2.98653680669434));
#51191=CARTESIAN_POINT('Ctrl Pts',(2.81380019196454,1.,-2.9835141977994));
#51192=CARTESIAN_POINT('Ctrl Pts',(2.80668968101162,1.,-2.98046109647299));
#51193=CARTESIAN_POINT('Ctrl Pts',(2.79960153278186,1.,-2.97737733718242));
#51194=CARTESIAN_POINT('Ctrl Pts',(2.79253615718147,1.,-2.97426288347475));
#51195=CARTESIAN_POINT('Ctrl Pts',(2.78549409123657,1.,-2.97111781461349));
#51196=CARTESIAN_POINT('Ctrl Pts',(2.77847589542767,1.,-2.9679422104295));
#51197=CARTESIAN_POINT('Ctrl Pts',(2.77148206836464,1.,-2.96473605585548));
#51198=CARTESIAN_POINT('Ctrl Pts',(2.76451296269571,1.,-2.96149914764832));
#51199=CARTESIAN_POINT('Ctrl Pts',(2.75756867888393,1.,-2.9582309766594));
#51200=CARTESIAN_POINT('Ctrl Pts',(2.75064903318996,1.,-2.95493069316211));
#51201=CARTESIAN_POINT('Ctrl Pts',(2.7437537949221,1.,-2.95159737214305));
#51202=CARTESIAN_POINT('Ctrl Pts',(2.73688288329825,1.,-2.94823023414381));
#51203=CARTESIAN_POINT('Ctrl Pts',(2.73003657371613,1.,-2.94482887675139));
#51204=CARTESIAN_POINT('Ctrl Pts',(2.72321571511322,1.,-2.94139351933882));
#51205=CARTESIAN_POINT('Ctrl Pts',(2.71642190053575,1.,-2.93792519474955));
#51206=CARTESIAN_POINT('Ctrl Pts',(2.70965695523776,1.,-2.93442516311168));
#51207=CARTESIAN_POINT('Ctrl Pts',(2.70292247416881,1.,-2.93089438233746));
#51208=CARTESIAN_POINT('Ctrl Pts',(2.69621932864302,1.,-2.92733294395268));
#51209=CARTESIAN_POINT('Ctrl Pts',(2.68954721165342,1.,-2.92373955325876));
#51210=CARTESIAN_POINT('Ctrl Pts',(2.68290409279689,1.,-2.92011090722152));
#51211=CARTESIAN_POINT('Ctrl Pts',(2.67628728855309,1.,-2.91644290704281));
#51212=CARTESIAN_POINT('Ctrl Pts',(2.66969458792627,1.,-2.91273193382876));
#51213=CARTESIAN_POINT('Ctrl Pts',(2.66312542616808,1.,-2.90897617968921));
#51214=CARTESIAN_POINT('Ctrl Pts',(2.65658188464287,1.,-2.90517678087467));
#51215=CARTESIAN_POINT('Ctrl Pts',(2.65007017365576,1.,-2.90133950224879));
#51216=CARTESIAN_POINT('Ctrl Pts',(2.64359851684146,1.,-2.89747231723361));
#51217=CARTESIAN_POINT('Ctrl Pts',(2.63717442263944,1.,-2.89358228854557));
#51218=CARTESIAN_POINT('Ctrl Pts',(2.63080195420771,1.,-2.88967244854243));
#51219=CARTESIAN_POINT('Ctrl Pts',(2.62447947640253,1.,-2.88573922195049));
#51220=CARTESIAN_POINT('Ctrl Pts',(2.61819596473087,1.,-2.88176821427502));
#51221=CARTESIAN_POINT('Ctrl Pts',(2.61193507170928,1.,-2.87773881947885));
#51222=CARTESIAN_POINT('Ctrl Pts',(2.6056817788128,1.,-2.87363176656475));
#51223=CARTESIAN_POINT('Ctrl Pts',(2.59942875223202,1.,-2.86943633170712));
#51224=CARTESIAN_POINT('Ctrl Pts',(2.59318160184921,1.,-2.86515629953528));
#51225=CARTESIAN_POINT('Ctrl Pts',(2.5869677064356,1.,-2.86081999003668));
#51226=CARTESIAN_POINT('Ctrl Pts',(2.58082875254407,1.,-2.85647171715147));
#51227=CARTESIAN_POINT('Ctrl Pts',(2.57480482727128,1.,-2.85215360144483));
#51228=CARTESIAN_POINT('Ctrl Pts',(2.56891984251743,1.,-2.84788893329091));
#51229=CARTESIAN_POINT('Ctrl Pts',(2.56316920798489,1.,-2.84366802680211));
#51230=CARTESIAN_POINT('Ctrl Pts',(2.55749952145165,1.,-2.83942515220699));
#51231=CARTESIAN_POINT('Ctrl Pts',(2.55182152806964,1.,-2.83505269592412));
#51232=CARTESIAN_POINT('Ctrl Pts',(2.54604736792542,1.,-2.83044254225794));
#51233=CARTESIAN_POINT('Ctrl Pts',(2.54012272520141,1.,-2.82552167649157));
#51234=CARTESIAN_POINT('Ctrl Pts',(2.53405679667463,1.,-2.82028550483744));
#51235=CARTESIAN_POINT('Ctrl Pts',(2.52796388055457,1.,-2.8148437904867));
#51236=CARTESIAN_POINT('Ctrl Pts',(2.52205778589922,1.,-2.80941521967234));
#51237=CARTESIAN_POINT('Ctrl Pts',(2.51660190466067,1.,-2.80427363984939));
#51238=CARTESIAN_POINT('Ctrl Pts',(2.51186983687947,1.,-2.79970585014308));
#51239=CARTESIAN_POINT('Ctrl Pts',(2.50810555977564,1.,-2.7959687805717));
#51240=CARTESIAN_POINT('Ctrl Pts',(2.50567182569153,1.,-2.79344192164204));
#51241=CARTESIAN_POINT('Ctrl Pts',(2.50455968395235,1.,-2.79217568804874));
#51242=CARTESIAN_POINT('Ctrl Pts',(2.50417932839344,1.,-2.79164172519039));
#51243=CARTESIAN_POINT('Ctrl Pts',(2.50410700351427,1.,-2.79145823440899));
#51244=CARTESIAN_POINT('Ctrl Pts',(2.50410331873043,1.,-2.79140942341378));
#51245=CARTESIAN_POINT('',(2.91557726271063,0.,-3.02314558451372));
#51246=CARTESIAN_POINT('Ctrl Pts',(2.79134130681569,-1.,-2.50417924854921));
#51247=CARTESIAN_POINT('Ctrl Pts',(2.79134130681569,1.,-2.50417924854921));
#51248=CARTESIAN_POINT('Ctrl Pts',(2.7913358110015,-1.,-2.50409239460108));
#51249=CARTESIAN_POINT('Ctrl Pts',(2.7913358110015,1.,-2.50409239460108));
#51250=CARTESIAN_POINT('Ctrl Pts',(2.79143626022503,-1.,-2.50404230339286));
#51251=CARTESIAN_POINT('Ctrl Pts',(2.79143626022503,1.,-2.50404230339286));
#51252=CARTESIAN_POINT('Ctrl Pts',(2.79192122907148,-1.,-2.5043379907732));
#51253=CARTESIAN_POINT('Ctrl Pts',(2.79192122907148,1.,-2.5043379907732));
#51254=CARTESIAN_POINT('Ctrl Pts',(2.7932369408851,-1.,-2.50547439929414));
#51255=CARTESIAN_POINT('Ctrl Pts',(2.7932369408851,1.,-2.50547439929414));
#51256=CARTESIAN_POINT('Ctrl Pts',(2.79596878057287,-1.,-2.50810555977671));
#51257=CARTESIAN_POINT('Ctrl Pts',(2.79596878057287,1.,-2.50810555977671));
#51258=CARTESIAN_POINT('Ctrl Pts',(2.79970585014168,-1.,-2.51186983687818));
#51259=CARTESIAN_POINT('Ctrl Pts',(2.79970585014168,1.,-2.51186983687818));
#51260=CARTESIAN_POINT('Ctrl Pts',(2.80427363984653,-1.,-2.51660190465805));
#51261=CARTESIAN_POINT('Ctrl Pts',(2.80427363984653,1.,-2.51660190465805));
#51262=CARTESIAN_POINT('Ctrl Pts',(2.80941521966941,-1.,-2.52205778589653));
#51263=CARTESIAN_POINT('Ctrl Pts',(2.80941521966941,1.,-2.52205778589653));
#51264=CARTESIAN_POINT('Ctrl Pts',(2.81484379048475,-1.,-2.52796388055278));
#51265=CARTESIAN_POINT('Ctrl Pts',(2.81484379048475,1.,-2.52796388055278));
#51266=CARTESIAN_POINT('Ctrl Pts',(2.82028550483689,-1.,-2.53405679667412));
#51267=CARTESIAN_POINT('Ctrl Pts',(2.82028550483689,1.,-2.53405679667412));
#51268=CARTESIAN_POINT('Ctrl Pts',(2.8255216764922,-1.,-2.54012272520199));
#51269=CARTESIAN_POINT('Ctrl Pts',(2.8255216764922,1.,-2.54012272520199));
#51270=CARTESIAN_POINT('Ctrl Pts',(2.83044254225917,-1.,-2.54604736792655));
#51271=CARTESIAN_POINT('Ctrl Pts',(2.83044254225917,1.,-2.54604736792655));
#51272=CARTESIAN_POINT('Ctrl Pts',(2.83505269592536,-1.,-2.55182152807077));
#51273=CARTESIAN_POINT('Ctrl Pts',(2.83505269592536,1.,-2.55182152807077));
#51274=CARTESIAN_POINT('Ctrl Pts',(2.83942515220782,-1.,-2.55749952145241));
#51275=CARTESIAN_POINT('Ctrl Pts',(2.83942515220782,1.,-2.55749952145241));
#51276=CARTESIAN_POINT('Ctrl Pts',(2.84366802680237,-1.,-2.56316920798513));
#51277=CARTESIAN_POINT('Ctrl Pts',(2.84366802680237,1.,-2.56316920798513));
#51278=CARTESIAN_POINT('Ctrl Pts',(2.84788893329067,-1.,-2.56891984251721));
#51279=CARTESIAN_POINT('Ctrl Pts',(2.84788893329067,1.,-2.56891984251721));
#51280=CARTESIAN_POINT('Ctrl Pts',(2.85215360144431,-1.,-2.57480482727081));
#51281=CARTESIAN_POINT('Ctrl Pts',(2.85215360144431,1.,-2.57480482727081));
#51282=CARTESIAN_POINT('Ctrl Pts',(2.85647171715092,-1.,-2.58082875254357));
#51283=CARTESIAN_POINT('Ctrl Pts',(2.85647171715092,1.,-2.58082875254357));
#51284=CARTESIAN_POINT('Ctrl Pts',(2.86081999003629,-1.,-2.58696770643524));
#51285=CARTESIAN_POINT('Ctrl Pts',(2.86081999003629,1.,-2.58696770643524));
#51286=CARTESIAN_POINT('Ctrl Pts',(2.86515629953513,-1.,-2.59318160184908));
#51287=CARTESIAN_POINT('Ctrl Pts',(2.86515629953513,1.,-2.59318160184908));
#51288=CARTESIAN_POINT('Ctrl Pts',(2.86943633170722,-1.,-2.5994287522321));
#51289=CARTESIAN_POINT('Ctrl Pts',(2.86943633170722,1.,-2.5994287522321));
#51290=CARTESIAN_POINT('Ctrl Pts',(2.87363176656501,-1.,-2.60568177881303));
#51291=CARTESIAN_POINT('Ctrl Pts',(2.87363176656501,1.,-2.60568177881303));
#51292=CARTESIAN_POINT('Ctrl Pts',(2.87773881947915,-1.,-2.61193507170955));
#51293=CARTESIAN_POINT('Ctrl Pts',(2.87773881947915,1.,-2.61193507170955));
#51294=CARTESIAN_POINT('Ctrl Pts',(2.88176821427525,-1.,-2.61819596473108));
#51295=CARTESIAN_POINT('Ctrl Pts',(2.88176821427525,1.,-2.61819596473108));
#51296=CARTESIAN_POINT('Ctrl Pts',(2.88573922195059,-1.,-2.62447947640262));
#51297=CARTESIAN_POINT('Ctrl Pts',(2.88573922195059,1.,-2.62447947640262));
#51298=CARTESIAN_POINT('Ctrl Pts',(2.88967244854239,-1.,-2.63080195420767));
#51299=CARTESIAN_POINT('Ctrl Pts',(2.88967244854239,1.,-2.63080195420767));
#51300=CARTESIAN_POINT('Ctrl Pts',(2.89358228854544,-1.,-2.63717442263932));
#51301=CARTESIAN_POINT('Ctrl Pts',(2.89358228854544,1.,-2.63717442263932));
#51302=CARTESIAN_POINT('Ctrl Pts',(2.89747231723345,-1.,-2.64359851684131));
#51303=CARTESIAN_POINT('Ctrl Pts',(2.89747231723345,1.,-2.64359851684131));
#51304=CARTESIAN_POINT('Ctrl Pts',(2.90133950224867,-1.,-2.65007017365564));
#51305=CARTESIAN_POINT('Ctrl Pts',(2.90133950224867,1.,-2.65007017365564));
#51306=CARTESIAN_POINT('Ctrl Pts',(2.90517678087461,-1.,-2.65658188464282));
#51307=CARTESIAN_POINT('Ctrl Pts',(2.90517678087461,1.,-2.65658188464282));
#51308=CARTESIAN_POINT('Ctrl Pts',(2.90897617968923,-1.,-2.6631254261681));
#51309=CARTESIAN_POINT('Ctrl Pts',(2.90897617968923,1.,-2.6631254261681));
#51310=CARTESIAN_POINT('Ctrl Pts',(2.91273193382882,-1.,-2.66969458792631));
#51311=CARTESIAN_POINT('Ctrl Pts',(2.91273193382882,1.,-2.66969458792631));
#51312=CARTESIAN_POINT('Ctrl Pts',(2.91644290704285,-1.,-2.67628728855312));
#51313=CARTESIAN_POINT('Ctrl Pts',(2.91644290704285,1.,-2.67628728855312));
#51314=CARTESIAN_POINT('Ctrl Pts',(2.92011090722152,-1.,-2.68290409279688));
#51315=CARTESIAN_POINT('Ctrl Pts',(2.92011090722152,1.,-2.68290409279688));
#51316=CARTESIAN_POINT('Ctrl Pts',(2.92373955325875,-1.,-2.68954721165339));
#51317=CARTESIAN_POINT('Ctrl Pts',(2.92373955325875,1.,-2.68954721165339));
#51318=CARTESIAN_POINT('Ctrl Pts',(2.92733294395267,-1.,-2.69621932864301));
#51319=CARTESIAN_POINT('Ctrl Pts',(2.92733294395267,1.,-2.69621932864301));
#51320=CARTESIAN_POINT('Ctrl Pts',(2.93089438233749,-1.,-2.70292247416885));
#51321=CARTESIAN_POINT('Ctrl Pts',(2.93089438233749,1.,-2.70292247416885));
#51322=CARTESIAN_POINT('Ctrl Pts',(2.93442516311179,-1.,-2.70965695523787));
#51323=CARTESIAN_POINT('Ctrl Pts',(2.93442516311179,1.,-2.70965695523787));
#51324=CARTESIAN_POINT('Ctrl Pts',(2.93792519474972,-1.,-2.71642190053592));
#51325=CARTESIAN_POINT('Ctrl Pts',(2.93792519474972,1.,-2.71642190053592));
#51326=CARTESIAN_POINT('Ctrl Pts',(2.94139351933897,-1.,-2.72321571511337));
#51327=CARTESIAN_POINT('Ctrl Pts',(2.94139351933897,1.,-2.72321571511337));
#51328=CARTESIAN_POINT('Ctrl Pts',(2.94482887675143,-1.,-2.73003657371617));
#51329=CARTESIAN_POINT('Ctrl Pts',(2.94482887675143,1.,-2.73003657371617));
#51330=CARTESIAN_POINT('Ctrl Pts',(2.94823023414364,-1.,-2.73688288329808));
#51331=CARTESIAN_POINT('Ctrl Pts',(2.94823023414364,1.,-2.73688288329808));
#51332=CARTESIAN_POINT('Ctrl Pts',(2.95159737214266,-1.,-2.74375379492172));
#51333=CARTESIAN_POINT('Ctrl Pts',(2.95159737214266,1.,-2.74375379492172));
#51334=CARTESIAN_POINT('Ctrl Pts',(2.95493069316161,-1.,-2.75064903318947));
#51335=CARTESIAN_POINT('Ctrl Pts',(2.95493069316161,1.,-2.75064903318947));
#51336=CARTESIAN_POINT('Ctrl Pts',(2.95823097665896,-1.,-2.7575686788835));
#51337=CARTESIAN_POINT('Ctrl Pts',(2.95823097665896,1.,-2.7575686788835));
#51338=CARTESIAN_POINT('Ctrl Pts',(2.96149914764818,-1.,-2.76451296269557));
#51339=CARTESIAN_POINT('Ctrl Pts',(2.96149914764818,1.,-2.76451296269557));
#51340=CARTESIAN_POINT('Ctrl Pts',(2.96473605585583,-1.,-2.77148206836498));
#51341=CARTESIAN_POINT('Ctrl Pts',(2.96473605585583,1.,-2.77148206836498));
#51342=CARTESIAN_POINT('Ctrl Pts',(2.96794221043036,-1.,-2.7784758954285));
#51343=CARTESIAN_POINT('Ctrl Pts',(2.96794221043036,1.,-2.7784758954285));
#51344=CARTESIAN_POINT('Ctrl Pts',(2.97111781461465,-1.,-2.78549409123769));
#51345=CARTESIAN_POINT('Ctrl Pts',(2.97111781461465,1.,-2.78549409123769));
#51346=CARTESIAN_POINT('Ctrl Pts',(2.9742628834758,-1.,-2.79253615718248));
#51347=CARTESIAN_POINT('Ctrl Pts',(2.9742628834758,1.,-2.79253615718248));
#51348=CARTESIAN_POINT('Ctrl Pts',(2.97737733718287,-1.,-2.7996015327823));
#51349=CARTESIAN_POINT('Ctrl Pts',(2.97737733718287,1.,-2.7996015327823));
#51350=CARTESIAN_POINT('Ctrl Pts',(2.98046109647241,-1.,-2.80668968101106));
#51351=CARTESIAN_POINT('Ctrl Pts',(2.98046109647241,1.,-2.80668968101106));
#51352=CARTESIAN_POINT('Ctrl Pts',(2.98351419779767,-1.,-2.81380019196286));
#51353=CARTESIAN_POINT('Ctrl Pts',(2.98351419779767,1.,-2.81380019196286));
#51354=CARTESIAN_POINT('Ctrl Pts',(2.9865368066918,-1.,-2.82093279065457));
#51355=CARTESIAN_POINT('Ctrl Pts',(2.9865368066918,1.,-2.82093279065457));
#51356=CARTESIAN_POINT('Ctrl Pts',(2.98952916401446,-1.,-2.82808728190157));
#51357=CARTESIAN_POINT('Ctrl Pts',(2.98952916401446,1.,-2.82808728190157));
#51358=CARTESIAN_POINT('Ctrl Pts',(2.99249155170339,-1.,-2.83526351254248));
#51359=CARTESIAN_POINT('Ctrl Pts',(2.99249155170339,1.,-2.83526351254248));
#51360=CARTESIAN_POINT('Ctrl Pts',(2.99542425341685,-1.,-2.84246132984415));
#51361=CARTESIAN_POINT('Ctrl Pts',(2.99542425341685,1.,-2.84246132984415));
#51362=CARTESIAN_POINT('Ctrl Pts',(2.99832751144925,-1.,-2.84968053289451));
#51363=CARTESIAN_POINT('Ctrl Pts',(2.99832751144925,1.,-2.84968053289451));
#51364=CARTESIAN_POINT('Ctrl Pts',(3.00120150796095,-1.,-2.85692085715686));
#51365=CARTESIAN_POINT('Ctrl Pts',(3.00120150796095,1.,-2.85692085715686));
#51366=CARTESIAN_POINT('Ctrl Pts',(3.00404638316867,-1.,-2.86418200833667));
#51367=CARTESIAN_POINT('Ctrl Pts',(3.00404638316867,1.,-2.86418200833667));
#51368=CARTESIAN_POINT('Ctrl Pts',(3.00686224485784,-1.,-2.87146368430502));
#51369=CARTESIAN_POINT('Ctrl Pts',(3.00686224485784,1.,-2.87146368430502));
#51370=CARTESIAN_POINT('Ctrl Pts',(3.00964918108476,-1.,-2.87876560072727));
#51371=CARTESIAN_POINT('Ctrl Pts',(3.00964918108476,1.,-2.87876560072727));
#51372=CARTESIAN_POINT('Ctrl Pts',(3.01240727308829,-1.,-2.8860875170608));
#51373=CARTESIAN_POINT('Ctrl Pts',(3.01240727308829,1.,-2.8860875170608));
#51374=CARTESIAN_POINT('Ctrl Pts',(3.01513660431928,-1.,-2.89342925566321));
#51375=CARTESIAN_POINT('Ctrl Pts',(3.01513660431928,1.,-2.89342925566321));
#51376=CARTESIAN_POINT('Ctrl Pts',(3.01783725121981,-1.,-2.9007906910105));
#51377=CARTESIAN_POINT('Ctrl Pts',(3.01783725121981,1.,-2.9007906910105));
#51378=CARTESIAN_POINT('Ctrl Pts',(3.01997487193503,-1.,-2.90669553302526));
#51379=CARTESIAN_POINT('Ctrl Pts',(3.01997487193503,1.,-2.90669553302526));
#51380=CARTESIAN_POINT('Ctrl Pts',(3.02156522742431,-1.,-2.91113297348212));
#51381=CARTESIAN_POINT('Ctrl Pts',(3.02156522742431,1.,-2.91113297348212));
#51382=CARTESIAN_POINT('Ctrl Pts',(3.02261975104593,-1.,-2.91409518070399));
#51383=CARTESIAN_POINT('Ctrl Pts',(3.02261975104593,1.,-2.91409518070399));
#51384=CARTESIAN_POINT('Ctrl Pts',(3.02314558451372,-1.,-2.91557726271063));
#51385=CARTESIAN_POINT('Ctrl Pts',(3.02314558451372,1.,-2.91557726271063));
#51386=CARTESIAN_POINT('',(2.79140942341258,1.,-2.50410331873176));
#51387=CARTESIAN_POINT('Ctrl Pts',(2.79140942341258,-1.,-2.50410331873176));
#51388=CARTESIAN_POINT('Ctrl Pts',(2.79140942341258,-0.666666666666667,
-2.50410331873176));
#51389=CARTESIAN_POINT('Ctrl Pts',(2.79140942341258,-0.333333333333333,
-2.50410331873176));
#51390=CARTESIAN_POINT('Ctrl Pts',(2.79140942341258,0.333333333333333,-2.50410331873176));
#51391=CARTESIAN_POINT('Ctrl Pts',(2.79140942341258,0.666666666666667,-2.50410331873176));
#51392=CARTESIAN_POINT('Ctrl Pts',(2.79140942341258,1.,-2.50410331873176));
#51393=CARTESIAN_POINT('',(3.02314558451372,1.,-2.91557726271063));
#51394=CARTESIAN_POINT('',(3.02314558451372,0.,-2.91557726271063));
#51395=CARTESIAN_POINT('Ctrl Pts',(2.79140942341258,1.,-2.50410331873176));
#51396=CARTESIAN_POINT('Ctrl Pts',(2.79145823440781,1.,-2.50410700351493));
#51397=CARTESIAN_POINT('Ctrl Pts',(2.79164172518905,1.,-2.50417932839313));
#51398=CARTESIAN_POINT('Ctrl Pts',(2.79217568804755,1.,-2.50455968395146));
#51399=CARTESIAN_POINT('Ctrl Pts',(2.79344192164147,1.,-2.50567182569081));
#51400=CARTESIAN_POINT('Ctrl Pts',(2.79596878057287,1.,-2.50810555977671));
#51401=CARTESIAN_POINT('Ctrl Pts',(2.79970585014168,1.,-2.51186983687818));
#51402=CARTESIAN_POINT('Ctrl Pts',(2.80427363984653,1.,-2.51660190465805));
#51403=CARTESIAN_POINT('Ctrl Pts',(2.80941521966941,1.,-2.52205778589653));
#51404=CARTESIAN_POINT('Ctrl Pts',(2.81484379048475,1.,-2.52796388055278));
#51405=CARTESIAN_POINT('Ctrl Pts',(2.82028550483689,1.,-2.53405679667412));
#51406=CARTESIAN_POINT('Ctrl Pts',(2.8255216764922,1.,-2.54012272520199));
#51407=CARTESIAN_POINT('Ctrl Pts',(2.83044254225917,1.,-2.54604736792655));
#51408=CARTESIAN_POINT('Ctrl Pts',(2.83505269592536,1.,-2.55182152807077));
#51409=CARTESIAN_POINT('Ctrl Pts',(2.83942515220782,1.,-2.55749952145241));
#51410=CARTESIAN_POINT('Ctrl Pts',(2.84366802680237,1.,-2.56316920798513));
#51411=CARTESIAN_POINT('Ctrl Pts',(2.84788893329067,1.,-2.56891984251721));
#51412=CARTESIAN_POINT('Ctrl Pts',(2.85215360144431,1.,-2.57480482727081));
#51413=CARTESIAN_POINT('Ctrl Pts',(2.85647171715092,1.,-2.58082875254357));
#51414=CARTESIAN_POINT('Ctrl Pts',(2.86081999003629,1.,-2.58696770643524));
#51415=CARTESIAN_POINT('Ctrl Pts',(2.86515629953513,1.,-2.59318160184908));
#51416=CARTESIAN_POINT('Ctrl Pts',(2.86943633170722,1.,-2.5994287522321));
#51417=CARTESIAN_POINT('Ctrl Pts',(2.87363176656501,1.,-2.60568177881303));
#51418=CARTESIAN_POINT('Ctrl Pts',(2.87773881947915,1.,-2.61193507170955));
#51419=CARTESIAN_POINT('Ctrl Pts',(2.88176821427525,1.,-2.61819596473108));
#51420=CARTESIAN_POINT('Ctrl Pts',(2.88573922195059,1.,-2.62447947640262));
#51421=CARTESIAN_POINT('Ctrl Pts',(2.88967244854239,1.,-2.63080195420767));
#51422=CARTESIAN_POINT('Ctrl Pts',(2.89358228854544,1.,-2.63717442263932));
#51423=CARTESIAN_POINT('Ctrl Pts',(2.89747231723345,1.,-2.64359851684131));
#51424=CARTESIAN_POINT('Ctrl Pts',(2.90133950224867,1.,-2.65007017365564));
#51425=CARTESIAN_POINT('Ctrl Pts',(2.90517678087461,1.,-2.65658188464282));
#51426=CARTESIAN_POINT('Ctrl Pts',(2.90897617968923,1.,-2.6631254261681));
#51427=CARTESIAN_POINT('Ctrl Pts',(2.91273193382882,1.,-2.66969458792631));
#51428=CARTESIAN_POINT('Ctrl Pts',(2.91644290704285,1.,-2.67628728855312));
#51429=CARTESIAN_POINT('Ctrl Pts',(2.92011090722152,1.,-2.68290409279688));
#51430=CARTESIAN_POINT('Ctrl Pts',(2.92373955325875,1.,-2.68954721165339));
#51431=CARTESIAN_POINT('Ctrl Pts',(2.92733294395267,1.,-2.69621932864301));
#51432=CARTESIAN_POINT('Ctrl Pts',(2.93089438233749,1.,-2.70292247416885));
#51433=CARTESIAN_POINT('Ctrl Pts',(2.93442516311179,1.,-2.70965695523787));
#51434=CARTESIAN_POINT('Ctrl Pts',(2.93792519474972,1.,-2.71642190053592));
#51435=CARTESIAN_POINT('Ctrl Pts',(2.94139351933897,1.,-2.72321571511337));
#51436=CARTESIAN_POINT('Ctrl Pts',(2.94482887675143,1.,-2.73003657371617));
#51437=CARTESIAN_POINT('Ctrl Pts',(2.94823023414364,1.,-2.73688288329808));
#51438=CARTESIAN_POINT('Ctrl Pts',(2.95159737214266,1.,-2.74375379492172));
#51439=CARTESIAN_POINT('Ctrl Pts',(2.95493069316161,1.,-2.75064903318947));
#51440=CARTESIAN_POINT('Ctrl Pts',(2.95823097665896,1.,-2.7575686788835));
#51441=CARTESIAN_POINT('Ctrl Pts',(2.96149914764818,1.,-2.76451296269557));
#51442=CARTESIAN_POINT('Ctrl Pts',(2.96473605585583,1.,-2.77148206836498));
#51443=CARTESIAN_POINT('Ctrl Pts',(2.96794221043036,1.,-2.7784758954285));
#51444=CARTESIAN_POINT('Ctrl Pts',(2.97111781461465,1.,-2.78549409123769));
#51445=CARTESIAN_POINT('Ctrl Pts',(2.9742628834758,1.,-2.79253615718248));
#51446=CARTESIAN_POINT('Ctrl Pts',(2.97737733718287,1.,-2.7996015327823));
#51447=CARTESIAN_POINT('Ctrl Pts',(2.98046109647241,1.,-2.80668968101106));
#51448=CARTESIAN_POINT('Ctrl Pts',(2.98351419779767,1.,-2.81380019196286));
#51449=CARTESIAN_POINT('Ctrl Pts',(2.9865368066918,1.,-2.82093279065457));
#51450=CARTESIAN_POINT('Ctrl Pts',(2.98952916401446,1.,-2.82808728190157));
#51451=CARTESIAN_POINT('Ctrl Pts',(2.99249155170339,1.,-2.83526351254248));
#51452=CARTESIAN_POINT('Ctrl Pts',(2.99542425341685,1.,-2.84246132984415));
#51453=CARTESIAN_POINT('Ctrl Pts',(2.99832751144925,1.,-2.84968053289451));
#51454=CARTESIAN_POINT('Ctrl Pts',(3.00120150796095,1.,-2.85692085715686));
#51455=CARTESIAN_POINT('Ctrl Pts',(3.00404638316867,1.,-2.86418200833667));
#51456=CARTESIAN_POINT('Ctrl Pts',(3.00686224485784,1.,-2.87146368430502));
#51457=CARTESIAN_POINT('Ctrl Pts',(3.00964918108476,1.,-2.87876560072727));
#51458=CARTESIAN_POINT('Ctrl Pts',(3.01240727308829,1.,-2.8860875170608));
#51459=CARTESIAN_POINT('Ctrl Pts',(3.01513660431928,1.,-2.89342925566321));
#51460=CARTESIAN_POINT('Ctrl Pts',(3.01783725121981,1.,-2.9007906910105));
#51461=CARTESIAN_POINT('Ctrl Pts',(3.01997487193503,1.,-2.90669553302526));
#51462=CARTESIAN_POINT('Ctrl Pts',(3.02156522742431,1.,-2.91113297348212));
#51463=CARTESIAN_POINT('Ctrl Pts',(3.02261975104593,1.,-2.91409518070399));
#51464=CARTESIAN_POINT('Ctrl Pts',(3.02314558451372,1.,-2.91557726271063));
#51465=CARTESIAN_POINT('Origin',(3.02314558451372,0.,-2.91557726271063));
#51466=CARTESIAN_POINT('',(2.91557726271063,1.,-3.02314558451372));
#51467=CARTESIAN_POINT('Origin',(0.,0.,0.));
#51468=CARTESIAN_POINT('',(2.90994629141562,1.,-2.36531447826213));
#51469=CARTESIAN_POINT('Origin',(0.,1.,0.));
#51470=CARTESIAN_POINT('Ctrl Pts',(2.90994629141562,1.,-2.36531447826213));
#51471=CARTESIAN_POINT('Ctrl Pts',(2.90994629141562,0.666666666666667,-2.36531447826213));
#51472=CARTESIAN_POINT('Ctrl Pts',(2.90994629141562,0.333333333333333,-2.36531447826213));
#51473=CARTESIAN_POINT('Ctrl Pts',(2.90994629141562,-0.333333333333333,
-2.36531447826213));
#51474=CARTESIAN_POINT('Ctrl Pts',(2.90994629141562,-0.666666666666667,
-2.36531447826213));
#51475=CARTESIAN_POINT('Ctrl Pts',(2.90994629141562,-1.,-2.36531447826213));
#51476=CARTESIAN_POINT('Ctrl Pts',(3.35260583073571,-1.,-2.52982887637028));
#51477=CARTESIAN_POINT('Ctrl Pts',(3.35260583073571,1.,-2.52982887637028));
#51478=CARTESIAN_POINT('Ctrl Pts',(3.35105973714426,-1.,-2.52954136549357));
#51479=CARTESIAN_POINT('Ctrl Pts',(3.35105973714426,1.,-2.52954136549357));
#51480=CARTESIAN_POINT('Ctrl Pts',(3.34796903577628,-1.,-2.5289632161143));
#51481=CARTESIAN_POINT('Ctrl Pts',(3.34796903577628,1.,-2.5289632161143));
#51482=CARTESIAN_POINT('Ctrl Pts',(3.34333744117093,-1.,-2.52808660916879));
#51483=CARTESIAN_POINT('Ctrl Pts',(3.34333744117093,1.,-2.52808660916879));
#51484=CARTESIAN_POINT('Ctrl Pts',(3.33717090000955,-1.,-2.52689902691551));
#51485=CARTESIAN_POINT('Ctrl Pts',(3.33717090000955,1.,-2.52689902691551));
#51486=CARTESIAN_POINT('Ctrl Pts',(3.32947762189049,-1.,-2.52538321165774));
#51487=CARTESIAN_POINT('Ctrl Pts',(3.32947762189049,1.,-2.52538321165774));
#51488=CARTESIAN_POINT('Ctrl Pts',(3.32179931079521,-1.,-2.52383598396878));
#51489=CARTESIAN_POINT('Ctrl Pts',(3.32179931079521,1.,-2.52383598396878));
#51490=CARTESIAN_POINT('Ctrl Pts',(3.31413607874727,-1.,-2.52225724871375));
#51491=CARTESIAN_POINT('Ctrl Pts',(3.31413607874727,1.,-2.52225724871375));
#51492=CARTESIAN_POINT('Ctrl Pts',(3.30648808814986,-1.,-2.52064689568167));
#51493=CARTESIAN_POINT('Ctrl Pts',(3.30648808814986,1.,-2.52064689568167));
#51494=CARTESIAN_POINT('Ctrl Pts',(3.29885556387661,-1.,-2.51900480700548));
#51495=CARTESIAN_POINT('Ctrl Pts',(3.29885556387661,1.,-2.51900480700548));
#51496=CARTESIAN_POINT('Ctrl Pts',(3.2912387729863,-1.,-2.51733085123316));
#51497=CARTESIAN_POINT('Ctrl Pts',(3.2912387729863,1.,-2.51733085123316));
#51498=CARTESIAN_POINT('Ctrl Pts',(3.28363799702583,-1.,-2.51562487464215));
#51499=CARTESIAN_POINT('Ctrl Pts',(3.28363799702583,1.,-2.51562487464215));
#51500=CARTESIAN_POINT('Ctrl Pts',(3.27605350473048,-1.,-2.51388669270329));
#51501=CARTESIAN_POINT('Ctrl Pts',(3.27605350473048,1.,-2.51388669270329));
#51502=CARTESIAN_POINT('Ctrl Pts',(3.26848552888271,-1.,-2.51211608411539));
#51503=CARTESIAN_POINT('Ctrl Pts',(3.26848552888271,1.,-2.51211608411539));
#51504=CARTESIAN_POINT('Ctrl Pts',(3.26093423001716,-1.,-2.51031277813697));
#51505=CARTESIAN_POINT('Ctrl Pts',(3.26093423001716,1.,-2.51031277813697));
#51506=CARTESIAN_POINT('Ctrl Pts',(3.25339971461265,-1.,-2.50847647070936));
#51507=CARTESIAN_POINT('Ctrl Pts',(3.25339971461265,1.,-2.50847647070936));
#51508=CARTESIAN_POINT('Ctrl Pts',(3.24588208984042,-1.,-2.50660685940645));
#51509=CARTESIAN_POINT('Ctrl Pts',(3.24588208984042,1.,-2.50660685940645));
#51510=CARTESIAN_POINT('Ctrl Pts',(3.23838151080383,-1.,-2.50470367580078));
#51511=CARTESIAN_POINT('Ctrl Pts',(3.23838151080383,1.,-2.50470367580078));
#51512=CARTESIAN_POINT('Ctrl Pts',(3.23089822320596,-1.,-2.50276671338074));
#51513=CARTESIAN_POINT('Ctrl Pts',(3.23089822320596,1.,-2.50276671338074));
#51514=CARTESIAN_POINT('Ctrl Pts',(3.22343262620387,-1.,-2.5007958720187));
#51515=CARTESIAN_POINT('Ctrl Pts',(3.22343262620387,1.,-2.5007958720187));
#51516=CARTESIAN_POINT('Ctrl Pts',(3.21598526261157,-1.,-2.49879114599293));
#51517=CARTESIAN_POINT('Ctrl Pts',(3.21598526261157,1.,-2.49879114599293));
#51518=CARTESIAN_POINT('Ctrl Pts',(3.2085566984974,-1.,-2.49675252647298));
#51519=CARTESIAN_POINT('Ctrl Pts',(3.2085566984974,1.,-2.49675252647298));
#51520=CARTESIAN_POINT('Ctrl Pts',(3.20114742397549,-1.,-2.49467992057726));
#51521=CARTESIAN_POINT('Ctrl Pts',(3.20114742397549,1.,-2.49467992057726));
#51522=CARTESIAN_POINT('Ctrl Pts',(3.19375775555814,-1.,-2.4925730723986));
#51523=CARTESIAN_POINT('Ctrl Pts',(3.19375775555814,1.,-2.4925730723986));
#51524=CARTESIAN_POINT('Ctrl Pts',(3.18638771282315,-1.,-2.49043146334095));
#51525=CARTESIAN_POINT('Ctrl Pts',(3.18638771282315,1.,-2.49043146334095));
#51526=CARTESIAN_POINT('Ctrl Pts',(3.17903698136678,-1.,-2.48825428288243));
#51527=CARTESIAN_POINT('Ctrl Pts',(3.17903698136678,1.,-2.48825428288243));
#51528=CARTESIAN_POINT('Ctrl Pts',(3.17170518863357,-1.,-2.48604065348619));
#51529=CARTESIAN_POINT('Ctrl Pts',(3.17170518863357,1.,-2.48604065348619));
#51530=CARTESIAN_POINT('Ctrl Pts',(3.16439213290181,-1.,-2.48378981792739));
#51531=CARTESIAN_POINT('Ctrl Pts',(3.16439213290181,1.,-2.48378981792739));
#51532=CARTESIAN_POINT('Ctrl Pts',(3.15709802322735,-1.,-2.48150133566568));
#51533=CARTESIAN_POINT('Ctrl Pts',(3.15709802322735,1.,-2.48150133566568));
#51534=CARTESIAN_POINT('Ctrl Pts',(3.14982373241335,-1.,-2.47917529057016));
#51535=CARTESIAN_POINT('Ctrl Pts',(3.14982373241335,1.,-2.47917529057016));
#51536=CARTESIAN_POINT('Ctrl Pts',(3.14257099546531,-1.,-2.47681245356095));
#51537=CARTESIAN_POINT('Ctrl Pts',(3.14257099546531,1.,-2.47681245356095));
#51538=CARTESIAN_POINT('Ctrl Pts',(3.13534181229282,-1.,-2.47441378371923));
#51539=CARTESIAN_POINT('Ctrl Pts',(3.13534181229282,1.,-2.47441378371923));
#51540=CARTESIAN_POINT('Ctrl Pts',(3.12813790805948,-1.,-2.47197997765868));
#51541=CARTESIAN_POINT('Ctrl Pts',(3.12813790805948,1.,-2.47197997765868));
#51542=CARTESIAN_POINT('Ctrl Pts',(3.12096015766984,-1.,-2.4695109894747));
#51543=CARTESIAN_POINT('Ctrl Pts',(3.12096015766984,1.,-2.4695109894747));
#51544=CARTESIAN_POINT('Ctrl Pts',(3.11380805536124,-1.,-2.46700558843507));
#51545=CARTESIAN_POINT('Ctrl Pts',(3.11380805536124,1.,-2.46700558843507));
#51546=CARTESIAN_POINT('Ctrl Pts',(3.10667907901981,-1.,-2.46446082979645));
#51547=CARTESIAN_POINT('Ctrl Pts',(3.10667907901981,1.,-2.46446082979645));
#51548=CARTESIAN_POINT('Ctrl Pts',(3.09956993697048,-1.,-2.4618730850188));
#51549=CARTESIAN_POINT('Ctrl Pts',(3.09956993697048,1.,-2.4618730850188));
#51550=CARTESIAN_POINT('Ctrl Pts',(3.09247787931881,-1.,-2.45923912563875));
#51551=CARTESIAN_POINT('Ctrl Pts',(3.09247787931881,1.,-2.45923912563875));
#51552=CARTESIAN_POINT('Ctrl Pts',(3.08540206545313,-1.,-2.45655725437037));
#51553=CARTESIAN_POINT('Ctrl Pts',(3.08540206545313,1.,-2.45655725437037));
#51554=CARTESIAN_POINT('Ctrl Pts',(3.07834472886145,-1.,-2.45382826787795));
#51555=CARTESIAN_POINT('Ctrl Pts',(3.07834472886145,1.,-2.45382826787795));
#51556=CARTESIAN_POINT('Ctrl Pts',(3.0713129052131,-1.,-2.45105688854432));
#51557=CARTESIAN_POINT('Ctrl Pts',(3.0713129052131,1.,-2.45105688854432));
#51558=CARTESIAN_POINT('Ctrl Pts',(3.06431596421422,-1.,-2.44824970516558));
#51559=CARTESIAN_POINT('Ctrl Pts',(3.06431596421422,1.,-2.44824970516558));
#51560=CARTESIAN_POINT('Ctrl Pts',(3.05736242671521,-1.,-2.44541251892568));
#51561=CARTESIAN_POINT('Ctrl Pts',(3.05736242671521,1.,-2.44541251892568));
#51562=CARTESIAN_POINT('Ctrl Pts',(3.05045678021509,-1.,-2.44254768923109));
#51563=CARTESIAN_POINT('Ctrl Pts',(3.05045678021509,1.,-2.44254768923109));
#51564=CARTESIAN_POINT('Ctrl Pts',(3.04359685040545,-1.,-2.43965194061849));
#51565=CARTESIAN_POINT('Ctrl Pts',(3.04359685040545,1.,-2.43965194061849));
#51566=CARTESIAN_POINT('Ctrl Pts',(3.03676949672797,-1.,-2.43671278042394));
#51567=CARTESIAN_POINT('Ctrl Pts',(3.03676949672797,1.,-2.43671278042394));
#51568=CARTESIAN_POINT('Ctrl Pts',(3.02995534946946,-1.,-2.43371241361462));
#51569=CARTESIAN_POINT('Ctrl Pts',(3.02995534946946,1.,-2.43371241361462));
#51570=CARTESIAN_POINT('Ctrl Pts',(3.02313656035977,-1.,-2.43063415586615));
#51571=CARTESIAN_POINT('Ctrl Pts',(3.02313656035977,1.,-2.43063415586615));
#51572=CARTESIAN_POINT('Ctrl Pts',(3.01630420830493,-1.,-2.4274685626416));
#51573=CARTESIAN_POINT('Ctrl Pts',(3.01630420830493,1.,-2.4274685626416));
#51574=CARTESIAN_POINT('Ctrl Pts',(3.00946442616674,-1.,-2.42421849439625));
#51575=CARTESIAN_POINT('Ctrl Pts',(3.00946442616674,1.,-2.42421849439625));
#51576=CARTESIAN_POINT('Ctrl Pts',(3.00264868586038,-1.,-2.42090763946812));
#51577=CARTESIAN_POINT('Ctrl Pts',(3.00264868586038,1.,-2.42090763946812));
#51578=CARTESIAN_POINT('Ctrl Pts',(2.99590509293561,-1.,-2.4175732450056));
#51579=CARTESIAN_POINT('Ctrl Pts',(2.99590509293561,1.,-2.4175732450056));
#51580=CARTESIAN_POINT('Ctrl Pts',(2.98927983005851,-1.,-2.4142506419963));
#51581=CARTESIAN_POINT('Ctrl Pts',(2.98927983005851,1.,-2.4142506419963));
#51582=CARTESIAN_POINT('Ctrl Pts',(2.98280015815132,-1.,-2.41095909342591));
#51583=CARTESIAN_POINT('Ctrl Pts',(2.98280015815132,1.,-2.41095909342591));
#51584=CARTESIAN_POINT('Ctrl Pts',(2.97646002822395,-1.,-2.40768975073691));
#51585=CARTESIAN_POINT('Ctrl Pts',(2.97646002822395,1.,-2.40768975073691));
#51586=CARTESIAN_POINT('Ctrl Pts',(2.97019641312272,-1.,-2.40438604734848));
#51587=CARTESIAN_POINT('Ctrl Pts',(2.97019641312272,1.,-2.40438604734848));
#51588=CARTESIAN_POINT('Ctrl Pts',(2.9639043224018,-1.,-2.40095565711535));
#51589=CARTESIAN_POINT('Ctrl Pts',(2.9639043224018,1.,-2.40095565711535));
#51590=CARTESIAN_POINT('Ctrl Pts',(2.95748006482811,-1.,-2.39730553974412));
#51591=CARTESIAN_POINT('Ctrl Pts',(2.95748006482811,1.,-2.39730553974412));
#51592=CARTESIAN_POINT('Ctrl Pts',(2.95085857128372,-1.,-2.39337207631613));
#51593=CARTESIAN_POINT('Ctrl Pts',(2.95085857128372,1.,-2.39337207631613));
#51594=CARTESIAN_POINT('Ctrl Pts',(2.94404820669135,-1.,-2.38914929090806));
#51595=CARTESIAN_POINT('Ctrl Pts',(2.94404820669135,1.,-2.38914929090806));
#51596=CARTESIAN_POINT('Ctrl Pts',(2.93717903280599,-1.,-2.38472771516476));
#51597=CARTESIAN_POINT('Ctrl Pts',(2.93717903280599,1.,-2.38472771516476));
#51598=CARTESIAN_POINT('Ctrl Pts',(2.93049643640517,-1.,-2.3802898958232));
#51599=CARTESIAN_POINT('Ctrl Pts',(2.93049643640517,1.,-2.3802898958232));
#51600=CARTESIAN_POINT('Ctrl Pts',(2.92430340582912,-1.,-2.37606510524271));
#51601=CARTESIAN_POINT('Ctrl Pts',(2.92430340582912,1.,-2.37606510524271));
#51602=CARTESIAN_POINT('Ctrl Pts',(2.9189150379156,-1.,-2.37229381109939));
#51603=CARTESIAN_POINT('Ctrl Pts',(2.9189150379156,1.,-2.37229381109939));
#51604=CARTESIAN_POINT('Ctrl Pts',(2.91461249883016,-1.,-2.36919161373074));
#51605=CARTESIAN_POINT('Ctrl Pts',(2.91461249883016,1.,-2.36919161373074));
#51606=CARTESIAN_POINT('Ctrl Pts',(2.9115863784165,-1.,-2.36690501170317));
#51607=CARTESIAN_POINT('Ctrl Pts',(2.9115863784165,1.,-2.36690501170317));
#51608=CARTESIAN_POINT('Ctrl Pts',(2.91025813829606,-1.,-2.36578327194396));
#51609=CARTESIAN_POINT('Ctrl Pts',(2.91025813829606,1.,-2.36578327194396));
#51610=CARTESIAN_POINT('Ctrl Pts',(2.90989022547738,-1.,-2.36535052956704));
#51611=CARTESIAN_POINT('Ctrl Pts',(2.90989022547738,1.,-2.36535052956704));
#51612=CARTESIAN_POINT('Ctrl Pts',(2.90992398626098,-1.,-2.36524348105023));
#51613=CARTESIAN_POINT('Ctrl Pts',(2.90992398626098,1.,-2.36524348105023));
#51614=CARTESIAN_POINT('Ctrl Pts',(2.91001063062876,-1.,-2.36523532225181));
#51615=CARTESIAN_POINT('Ctrl Pts',(2.91001063062876,1.,-2.36523532225181));
#51616=CARTESIAN_POINT('',(3.35260583073571,1.,-2.52982887637028));
#51617=CARTESIAN_POINT('Ctrl Pts',(3.35260583073571,1.,-2.52982887637028));
#51618=CARTESIAN_POINT('Ctrl Pts',(3.35105973714426,1.,-2.52954136549357));
#51619=CARTESIAN_POINT('Ctrl Pts',(3.34796903577628,1.,-2.5289632161143));
#51620=CARTESIAN_POINT('Ctrl Pts',(3.34333744117093,1.,-2.52808660916879));
#51621=CARTESIAN_POINT('Ctrl Pts',(3.33717090000955,1.,-2.52689902691551));
#51622=CARTESIAN_POINT('Ctrl Pts',(3.32947762189049,1.,-2.52538321165774));
#51623=CARTESIAN_POINT('Ctrl Pts',(3.32179931079521,1.,-2.52383598396878));
#51624=CARTESIAN_POINT('Ctrl Pts',(3.31413607874727,1.,-2.52225724871375));
#51625=CARTESIAN_POINT('Ctrl Pts',(3.30648808814986,1.,-2.52064689568167));
#51626=CARTESIAN_POINT('Ctrl Pts',(3.29885556387661,1.,-2.51900480700548));
#51627=CARTESIAN_POINT('Ctrl Pts',(3.2912387729863,1.,-2.51733085123316));
#51628=CARTESIAN_POINT('Ctrl Pts',(3.28363799702583,1.,-2.51562487464215));
#51629=CARTESIAN_POINT('Ctrl Pts',(3.27605350473048,1.,-2.51388669270329));
#51630=CARTESIAN_POINT('Ctrl Pts',(3.26848552888271,1.,-2.51211608411539));
#51631=CARTESIAN_POINT('Ctrl Pts',(3.26093423001716,1.,-2.51031277813697));
#51632=CARTESIAN_POINT('Ctrl Pts',(3.25339971461265,1.,-2.50847647070936));
#51633=CARTESIAN_POINT('Ctrl Pts',(3.24588208984042,1.,-2.50660685940645));
#51634=CARTESIAN_POINT('Ctrl Pts',(3.23838151080383,1.,-2.50470367580078));
#51635=CARTESIAN_POINT('Ctrl Pts',(3.23089822320596,1.,-2.50276671338074));
#51636=CARTESIAN_POINT('Ctrl Pts',(3.22343262620387,1.,-2.5007958720187));
#51637=CARTESIAN_POINT('Ctrl Pts',(3.21598526261157,1.,-2.49879114599293));
#51638=CARTESIAN_POINT('Ctrl Pts',(3.2085566984974,1.,-2.49675252647298));
#51639=CARTESIAN_POINT('Ctrl Pts',(3.20114742397549,1.,-2.49467992057726));
#51640=CARTESIAN_POINT('Ctrl Pts',(3.19375775555814,1.,-2.4925730723986));
#51641=CARTESIAN_POINT('Ctrl Pts',(3.18638771282315,1.,-2.49043146334095));
#51642=CARTESIAN_POINT('Ctrl Pts',(3.17903698136678,1.,-2.48825428288243));
#51643=CARTESIAN_POINT('Ctrl Pts',(3.17170518863357,1.,-2.48604065348619));
#51644=CARTESIAN_POINT('Ctrl Pts',(3.16439213290181,1.,-2.48378981792739));
#51645=CARTESIAN_POINT('Ctrl Pts',(3.15709802322735,1.,-2.48150133566568));
#51646=CARTESIAN_POINT('Ctrl Pts',(3.14982373241335,1.,-2.47917529057016));
#51647=CARTESIAN_POINT('Ctrl Pts',(3.14257099546531,1.,-2.47681245356095));
#51648=CARTESIAN_POINT('Ctrl Pts',(3.13534181229282,1.,-2.47441378371923));
#51649=CARTESIAN_POINT('Ctrl Pts',(3.12813790805948,1.,-2.47197997765868));
#51650=CARTESIAN_POINT('Ctrl Pts',(3.12096015766984,1.,-2.4695109894747));
#51651=CARTESIAN_POINT('Ctrl Pts',(3.11380805536124,1.,-2.46700558843507));
#51652=CARTESIAN_POINT('Ctrl Pts',(3.10667907901981,1.,-2.46446082979645));
#51653=CARTESIAN_POINT('Ctrl Pts',(3.09956993697048,1.,-2.4618730850188));
#51654=CARTESIAN_POINT('Ctrl Pts',(3.09247787931881,1.,-2.45923912563875));
#51655=CARTESIAN_POINT('Ctrl Pts',(3.08540206545313,1.,-2.45655725437037));
#51656=CARTESIAN_POINT('Ctrl Pts',(3.07834472886145,1.,-2.45382826787795));
#51657=CARTESIAN_POINT('Ctrl Pts',(3.0713129052131,1.,-2.45105688854432));
#51658=CARTESIAN_POINT('Ctrl Pts',(3.06431596421422,1.,-2.44824970516558));
#51659=CARTESIAN_POINT('Ctrl Pts',(3.05736242671521,1.,-2.44541251892568));
#51660=CARTESIAN_POINT('Ctrl Pts',(3.05045678021509,1.,-2.44254768923109));
#51661=CARTESIAN_POINT('Ctrl Pts',(3.04359685040545,1.,-2.43965194061849));
#51662=CARTESIAN_POINT('Ctrl Pts',(3.03676949672797,1.,-2.43671278042394));
#51663=CARTESIAN_POINT('Ctrl Pts',(3.02995534946946,1.,-2.43371241361462));
#51664=CARTESIAN_POINT('Ctrl Pts',(3.02313656035977,1.,-2.43063415586615));
#51665=CARTESIAN_POINT('Ctrl Pts',(3.01630420830493,1.,-2.4274685626416));
#51666=CARTESIAN_POINT('Ctrl Pts',(3.00946442616674,1.,-2.42421849439625));
#51667=CARTESIAN_POINT('Ctrl Pts',(3.00264868586038,1.,-2.42090763946812));
#51668=CARTESIAN_POINT('Ctrl Pts',(2.99590509293561,1.,-2.4175732450056));
#51669=CARTESIAN_POINT('Ctrl Pts',(2.98927983005851,1.,-2.4142506419963));
#51670=CARTESIAN_POINT('Ctrl Pts',(2.98280015815132,1.,-2.41095909342591));
#51671=CARTESIAN_POINT('Ctrl Pts',(2.97646002822395,1.,-2.40768975073691));
#51672=CARTESIAN_POINT('Ctrl Pts',(2.97019641312272,1.,-2.40438604734848));
#51673=CARTESIAN_POINT('Ctrl Pts',(2.9639043224018,1.,-2.40095565711535));
#51674=CARTESIAN_POINT('Ctrl Pts',(2.95748006482811,1.,-2.39730553974412));
#51675=CARTESIAN_POINT('Ctrl Pts',(2.95085857128372,1.,-2.39337207631613));
#51676=CARTESIAN_POINT('Ctrl Pts',(2.94404820669135,1.,-2.38914929090806));
#51677=CARTESIAN_POINT('Ctrl Pts',(2.93717903280599,1.,-2.38472771516476));
#51678=CARTESIAN_POINT('Ctrl Pts',(2.93049643640517,1.,-2.3802898958232));
#51679=CARTESIAN_POINT('Ctrl Pts',(2.92430340582912,1.,-2.37606510524271));
#51680=CARTESIAN_POINT('Ctrl Pts',(2.9189150379156,1.,-2.37229381109939));
#51681=CARTESIAN_POINT('Ctrl Pts',(2.91461249883016,1.,-2.36919161373074));
#51682=CARTESIAN_POINT('Ctrl Pts',(2.91181344022628,1.,-2.36707658451709));
#51683=CARTESIAN_POINT('Ctrl Pts',(2.91051690822262,1.,-2.36599991765853));
#51684=CARTESIAN_POINT('Ctrl Pts',(2.9100577052777,1.,-2.36553202948741));
#51685=CARTESIAN_POINT('Ctrl Pts',(2.90995756655558,1.,-2.3653621118858));
#51686=CARTESIAN_POINT('Ctrl Pts',(2.90994629141562,1.,-2.36531447826213));
#51687=CARTESIAN_POINT('',(3.35260583073571,0.,-2.52982887637028));
#51688=CARTESIAN_POINT('Ctrl Pts',(3.1487152044751,-1.,-2.03668666247593));
#51689=CARTESIAN_POINT('Ctrl Pts',(3.1487152044751,1.,-2.03668666247593));
#51690=CARTESIAN_POINT('Ctrl Pts',(3.14869618937258,-1.,-2.03660173757879));
#51691=CARTESIAN_POINT('Ctrl Pts',(3.14869618937258,1.,-2.03660173757879));
#51692=CARTESIAN_POINT('Ctrl Pts',(3.14878756590812,-1.,-2.03653654935592));
#51693=CARTESIAN_POINT('Ctrl Pts',(3.14878756590812,1.,-2.03653654935592));
#51694=CARTESIAN_POINT('Ctrl Pts',(3.14931281968048,-1.,-2.03675273049189));
#51695=CARTESIAN_POINT('Ctrl Pts',(3.14931281968048,1.,-2.03675273049189));
#51696=CARTESIAN_POINT('Ctrl Pts',(3.15079010635742,-1.,-2.03766932526445));
#51697=CARTESIAN_POINT('Ctrl Pts',(3.15079010635742,1.,-2.03766932526445));
#51698=CARTESIAN_POINT('Ctrl Pts',(3.15389991674792,-1.,-2.03984073791519));
#51699=CARTESIAN_POINT('Ctrl Pts',(3.15389991674792,1.,-2.03984073791519));
#51700=CARTESIAN_POINT('Ctrl Pts',(3.15817983946367,-1.,-2.04297406404027));
#51701=CARTESIAN_POINT('Ctrl Pts',(3.15817983946367,1.,-2.04297406404027));
#51702=CARTESIAN_POINT('Ctrl Pts',(3.16343165058912,-1.,-2.04693331247446));
#51703=CARTESIAN_POINT('Ctrl Pts',(3.16343165058912,1.,-2.04693331247446));
#51704=CARTESIAN_POINT('Ctrl Pts',(3.16936341689527,-1.,-2.05151770247233));
#51705=CARTESIAN_POINT('Ctrl Pts',(3.16936341689527,1.,-2.05151770247233));
#51706=CARTESIAN_POINT('Ctrl Pts',(3.17564906975371,-1.,-2.05650186773132));
#51707=CARTESIAN_POINT('Ctrl Pts',(3.17564906975371,1.,-2.05650186773132));
#51708=CARTESIAN_POINT('Ctrl Pts',(3.18197692964614,-1.,-2.06166849827101));
#51709=CARTESIAN_POINT('Ctrl Pts',(3.18197692964614,1.,-2.06166849827101));
#51710=CARTESIAN_POINT('Ctrl Pts',(3.18809755562368,-1.,-2.06684062744112));
#51711=CARTESIAN_POINT('Ctrl Pts',(3.18809755562368,1.,-2.06684062744112));
#51712=CARTESIAN_POINT('Ctrl Pts',(3.19388465568252,-1.,-2.07192253497857));
#51713=CARTESIAN_POINT('Ctrl Pts',(3.19388465568252,1.,-2.07192253497857));
#51714=CARTESIAN_POINT('Ctrl Pts',(3.19934132836019,-1.,-2.07690441870722));
#51715=CARTESIAN_POINT('Ctrl Pts',(3.19934132836019,1.,-2.07690441870722));
#51716=CARTESIAN_POINT('Ctrl Pts',(3.2045481863073,-1.,-2.08182850370878));
#51717=CARTESIAN_POINT('Ctrl Pts',(3.2045481863073,1.,-2.08182850370878));
#51718=CARTESIAN_POINT('Ctrl Pts',(3.20962575845463,-1.,-2.08676465517455));
#51719=CARTESIAN_POINT('Ctrl Pts',(3.20962575845463,1.,-2.08676465517455));
#51720=CARTESIAN_POINT('Ctrl Pts',(3.21469429601654,-1.,-2.09178419460443));
#51721=CARTESIAN_POINT('Ctrl Pts',(3.21469429601654,1.,-2.09178419460443));
#51722=CARTESIAN_POINT('Ctrl Pts',(3.21982707347009,-1.,-2.09692958434895));
#51723=CARTESIAN_POINT('Ctrl Pts',(3.21982707347009,1.,-2.09692958434895));
#51724=CARTESIAN_POINT('Ctrl Pts',(3.22503437553434,-1.,-2.10220384298492));
#51725=CARTESIAN_POINT('Ctrl Pts',(3.22503437553434,1.,-2.10220384298492));
#51726=CARTESIAN_POINT('Ctrl Pts',(3.23028945793289,-1.,-2.10758699642451));
#51727=CARTESIAN_POINT('Ctrl Pts',(3.23028945793289,1.,-2.10758699642451));
#51728=CARTESIAN_POINT('Ctrl Pts',(3.23554444767099,-1.,-2.11304604021773));
#51729=CARTESIAN_POINT('Ctrl Pts',(3.23554444767099,1.,-2.11304604021773));
#51730=CARTESIAN_POINT('Ctrl Pts',(3.24074905517293,-1.,-2.11854673326979));
#51731=CARTESIAN_POINT('Ctrl Pts',(3.24074905517293,1.,-2.11854673326979));
#51732=CARTESIAN_POINT('Ctrl Pts',(3.24587102613376,-1.,-2.12406646410962));
#51733=CARTESIAN_POINT('Ctrl Pts',(3.24587102613376,1.,-2.12406646410962));
#51734=CARTESIAN_POINT('Ctrl Pts',(3.25090574494028,-1.,-2.12960028396832));
#51735=CARTESIAN_POINT('Ctrl Pts',(3.25090574494028,1.,-2.12960028396832));
#51736=CARTESIAN_POINT('Ctrl Pts',(3.25586495065054,-1.,-2.13515375878803));
#51737=CARTESIAN_POINT('Ctrl Pts',(3.25586495065054,1.,-2.13515375878803));
#51738=CARTESIAN_POINT('Ctrl Pts',(3.26077002641879,-1.,-2.14073870754264));
#51739=CARTESIAN_POINT('Ctrl Pts',(3.26077002641879,1.,-2.14073870754264));
#51740=CARTESIAN_POINT('Ctrl Pts',(3.26564388189759,-1.,-2.1463680529566));
#51741=CARTESIAN_POINT('Ctrl Pts',(3.26564388189759,1.,-2.1463680529566));
#51742=CARTESIAN_POINT('Ctrl Pts',(3.27050245897228,-1.,-2.15205043199808));
#51743=CARTESIAN_POINT('Ctrl Pts',(3.27050245897228,1.,-2.15205043199808));
#51744=CARTESIAN_POINT('Ctrl Pts',(3.27534954469187,-1.,-2.15778690038347));
#51745=CARTESIAN_POINT('Ctrl Pts',(3.27534954469187,1.,-2.15778690038347));
#51746=CARTESIAN_POINT('Ctrl Pts',(3.280181508414,-1.,-2.16357391934425));
#51747=CARTESIAN_POINT('Ctrl Pts',(3.280181508414,1.,-2.16357391934425));
#51748=CARTESIAN_POINT('Ctrl Pts',(3.28499019979724,-1.,-2.16940517773455));
#51749=CARTESIAN_POINT('Ctrl Pts',(3.28499019979724,1.,-2.16940517773455));
#51750=CARTESIAN_POINT('Ctrl Pts',(3.28976645712568,-1.,-2.17527380048423));
#51751=CARTESIAN_POINT('Ctrl Pts',(3.28976645712568,1.,-2.17527380048423));
#51752=CARTESIAN_POINT('Ctrl Pts',(3.2945036150049,-1.,-2.18117455557065));
#51753=CARTESIAN_POINT('Ctrl Pts',(3.2945036150049,1.,-2.18117455557065));
#51754=CARTESIAN_POINT('Ctrl Pts',(3.29920022557639,-1.,-2.18710556500327));
#51755=CARTESIAN_POINT('Ctrl Pts',(3.29920022557639,1.,-2.18710556500327));
#51756=CARTESIAN_POINT('Ctrl Pts',(3.30385816281831,-1.,-2.19306710376111));
#51757=CARTESIAN_POINT('Ctrl Pts',(3.30385816281831,1.,-2.19306710376111));
#51758=CARTESIAN_POINT('Ctrl Pts',(3.30848134694595,-1.,-2.19906078949923));
#51759=CARTESIAN_POINT('Ctrl Pts',(3.30848134694595,1.,-2.19906078949923));
#51760=CARTESIAN_POINT('Ctrl Pts',(3.31307424608949,-1.,-2.20508863150607));
#51761=CARTESIAN_POINT('Ctrl Pts',(3.31307424608949,1.,-2.20508863150607));
#51762=CARTESIAN_POINT('Ctrl Pts',(3.31764044024235,-1.,-2.21115211847875));
#51763=CARTESIAN_POINT('Ctrl Pts',(3.31764044024235,1.,-2.21115211847875));
#51764=CARTESIAN_POINT('Ctrl Pts',(3.32218125618968,-1.,-2.21725135110898));
#51765=CARTESIAN_POINT('Ctrl Pts',(3.32218125618968,1.,-2.21725135110898));
#51766=CARTESIAN_POINT('Ctrl Pts',(3.3266964672289,-1.,-2.22338548312772));
#51767=CARTESIAN_POINT('Ctrl Pts',(3.3266964672289,1.,-2.22338548312772));
#51768=CARTESIAN_POINT('Ctrl Pts',(3.33118487773611,-1.,-2.22955308907233));
#51769=CARTESIAN_POINT('Ctrl Pts',(3.33118487773611,1.,-2.22955308907233));
#51770=CARTESIAN_POINT('Ctrl Pts',(3.33564495756481,-1.,-2.23575256328812));
#51771=CARTESIAN_POINT('Ctrl Pts',(3.33564495756481,1.,-2.23575256328812));
#51772=CARTESIAN_POINT('Ctrl Pts',(3.34007543738025,-1.,-2.24198249391422));
#51773=CARTESIAN_POINT('Ctrl Pts',(3.34007543738025,1.,-2.24198249391422));
#51774=CARTESIAN_POINT('Ctrl Pts',(3.34447596770723,-1.,-2.24824207678256));
#51775=CARTESIAN_POINT('Ctrl Pts',(3.34447596770723,1.,-2.24824207678256));
#51776=CARTESIAN_POINT('Ctrl Pts',(3.34884690292285,-1.,-2.25453097693483));
#51777=CARTESIAN_POINT('Ctrl Pts',(3.34884690292285,1.,-2.25453097693483));
#51778=CARTESIAN_POINT('Ctrl Pts',(3.35318902552626,-1.,-2.26084915222449));
#51779=CARTESIAN_POINT('Ctrl Pts',(3.35318902552626,1.,-2.26084915222449));
#51780=CARTESIAN_POINT('Ctrl Pts',(3.35750328523061,-1.,-2.2671966857991));
#51781=CARTESIAN_POINT('Ctrl Pts',(3.35750328523061,1.,-2.2671966857991));
#51782=CARTESIAN_POINT('Ctrl Pts',(3.36179055004409,-1.,-2.2735736262093));
#51783=CARTESIAN_POINT('Ctrl Pts',(3.36179055004409,1.,-2.2735736262093));
#51784=CARTESIAN_POINT('Ctrl Pts',(3.36605130713076,-1.,-2.27997979458037));
#51785=CARTESIAN_POINT('Ctrl Pts',(3.36605130713076,1.,-2.27997979458037));
#51786=CARTESIAN_POINT('Ctrl Pts',(3.37028570206488,-1.,-2.28641481081137));
#51787=CARTESIAN_POINT('Ctrl Pts',(3.37028570206488,1.,-2.28641481081137));
#51788=CARTESIAN_POINT('Ctrl Pts',(3.37449367172826,-1.,-2.29287818007393));
#51789=CARTESIAN_POINT('Ctrl Pts',(3.37449367172826,1.,-2.29287818007393));
#51790=CARTESIAN_POINT('Ctrl Pts',(3.37867504959433,-1.,-2.29936936127624));
#51791=CARTESIAN_POINT('Ctrl Pts',(3.37867504959433,1.,-2.29936936127624));
#51792=CARTESIAN_POINT('Ctrl Pts',(3.3828296733661,-1.,-2.30588783640343));
#51793=CARTESIAN_POINT('Ctrl Pts',(3.3828296733661,1.,-2.30588783640343));
#51794=CARTESIAN_POINT('Ctrl Pts',(3.38695751492462,-1.,-2.31243319489367));
#51795=CARTESIAN_POINT('Ctrl Pts',(3.38695751492462,1.,-2.31243319489367));
#51796=CARTESIAN_POINT('Ctrl Pts',(3.39105869474822,-1.,-2.31900513925424));
#51797=CARTESIAN_POINT('Ctrl Pts',(3.39105869474822,1.,-2.31900513925424));
#51798=CARTESIAN_POINT('Ctrl Pts',(3.39513342019756,-1.,-2.3256034390248));
#51799=CARTESIAN_POINT('Ctrl Pts',(3.39513342019756,1.,-2.3256034390248));
#51800=CARTESIAN_POINT('Ctrl Pts',(3.39918194577956,-1.,-2.33222789882489));
#51801=CARTESIAN_POINT('Ctrl Pts',(3.39918194577956,1.,-2.33222789882489));
#51802=CARTESIAN_POINT('Ctrl Pts',(3.40320452776743,-1.,-2.33887832342782));
#51803=CARTESIAN_POINT('Ctrl Pts',(3.40320452776743,1.,-2.33887832342782));
#51804=CARTESIAN_POINT('Ctrl Pts',(3.40720137404297,-1.,-2.34555447649188));
#51805=CARTESIAN_POINT('Ctrl Pts',(3.40720137404297,1.,-2.34555447649188));
#51806=CARTESIAN_POINT('Ctrl Pts',(3.41117262314119,-1.,-2.35225606824109));
#51807=CARTESIAN_POINT('Ctrl Pts',(3.41117262314119,1.,-2.35225606824109));
#51808=CARTESIAN_POINT('Ctrl Pts',(3.41511836751469,-1.,-2.35898278606946));
#51809=CARTESIAN_POINT('Ctrl Pts',(3.41511836751469,1.,-2.35898278606946));
#51810=CARTESIAN_POINT('Ctrl Pts',(3.41903866635852,-1.,-2.36573431470642));
#51811=CARTESIAN_POINT('Ctrl Pts',(3.41903866635852,1.,-2.36573431470642));
#51812=CARTESIAN_POINT('Ctrl Pts',(3.42293356216511,-1.,-2.37251035954292));
#51813=CARTESIAN_POINT('Ctrl Pts',(3.42293356216511,1.,-2.37251035954292));
#51814=CARTESIAN_POINT('Ctrl Pts',(3.42680309754399,-1.,-2.37931067028926));
#51815=CARTESIAN_POINT('Ctrl Pts',(3.42680309754399,1.,-2.37931067028926));
#51816=CARTESIAN_POINT('Ctrl Pts',(3.43064732712919,-1.,-2.38613505843552));
#51817=CARTESIAN_POINT('Ctrl Pts',(3.43064732712919,1.,-2.38613505843552));
#51818=CARTESIAN_POINT('Ctrl Pts',(3.4344663067854,-1.,-2.39298338804493));
#51819=CARTESIAN_POINT('Ctrl Pts',(3.4344663067854,1.,-2.39298338804493));
#51820=CARTESIAN_POINT('Ctrl Pts',(3.43750133064416,-1.,-2.39848113410292));
#51821=CARTESIAN_POINT('Ctrl Pts',(3.43750133064416,1.,-2.39848113410292));
#51822=CARTESIAN_POINT('Ctrl Pts',(3.43976627484234,-1.,-2.40261515589405));
#51823=CARTESIAN_POINT('Ctrl Pts',(3.43976627484234,1.,-2.40261515589405));
#51824=CARTESIAN_POINT('Ctrl Pts',(3.44127120683039,-1.,-2.4053759295909));
#51825=CARTESIAN_POINT('Ctrl Pts',(3.44127120683039,1.,-2.4053759295909));
#51826=CARTESIAN_POINT('Ctrl Pts',(3.44202241512147,-1.,-2.40675750623143));
#51827=CARTESIAN_POINT('Ctrl Pts',(3.44202241512147,1.,-2.40675750623143));
#51828=CARTESIAN_POINT('',(3.14877060440327,1.,-2.03660101169715));
#51829=CARTESIAN_POINT('Ctrl Pts',(3.14877060440327,-1.,-2.03660101169715));
#51830=CARTESIAN_POINT('Ctrl Pts',(3.14877060440327,-0.666666666666667,
-2.03660101169715));
#51831=CARTESIAN_POINT('Ctrl Pts',(3.14877060440327,-0.333333333333333,
-2.03660101169715));
#51832=CARTESIAN_POINT('Ctrl Pts',(3.14877060440327,0.333333333333333,-2.03660101169715));
#51833=CARTESIAN_POINT('Ctrl Pts',(3.14877060440328,0.666666666666667,-2.03660101169714));
#51834=CARTESIAN_POINT('Ctrl Pts',(3.14877060440328,1.,-2.03660101169714));
#51835=CARTESIAN_POINT('',(3.44202241512147,1.,-2.40675750623143));
#51836=CARTESIAN_POINT('',(3.44202241512147,0.,-2.40675750623143));
#51837=CARTESIAN_POINT('Ctrl Pts',(3.14877060440327,1.,-2.03660101169715));
#51838=CARTESIAN_POINT('Ctrl Pts',(3.14881939088124,1.,-2.03659701539259));
#51839=CARTESIAN_POINT('Ctrl Pts',(3.1490119366901,1.,-2.03663974554932));
#51840=CARTESIAN_POINT('Ctrl Pts',(3.14959882629804,1.,-2.03693188810544));
#51841=CARTESIAN_POINT('Ctrl Pts',(3.15102344775328,1.,-2.03783225495961));
#51842=CARTESIAN_POINT('Ctrl Pts',(3.15389991674792,1.,-2.03984073791519));
#51843=CARTESIAN_POINT('Ctrl Pts',(3.15817983946367,1.,-2.04297406404027));
#51844=CARTESIAN_POINT('Ctrl Pts',(3.16343165058912,1.,-2.04693331247446));
#51845=CARTESIAN_POINT('Ctrl Pts',(3.16936341689527,1.,-2.05151770247233));
#51846=CARTESIAN_POINT('Ctrl Pts',(3.17564906975371,1.,-2.05650186773132));
#51847=CARTESIAN_POINT('Ctrl Pts',(3.18197692964614,1.,-2.06166849827101));
#51848=CARTESIAN_POINT('Ctrl Pts',(3.18809755562368,1.,-2.06684062744112));
#51849=CARTESIAN_POINT('Ctrl Pts',(3.19388465568252,1.,-2.07192253497857));
#51850=CARTESIAN_POINT('Ctrl Pts',(3.19934132836019,1.,-2.07690441870722));
#51851=CARTESIAN_POINT('Ctrl Pts',(3.2045481863073,1.,-2.08182850370878));
#51852=CARTESIAN_POINT('Ctrl Pts',(3.20962575845463,1.,-2.08676465517455));
#51853=CARTESIAN_POINT('Ctrl Pts',(3.21469429601654,1.,-2.09178419460443));
#51854=CARTESIAN_POINT('Ctrl Pts',(3.21982707347009,1.,-2.09692958434895));
#51855=CARTESIAN_POINT('Ctrl Pts',(3.22503437553434,1.,-2.10220384298492));
#51856=CARTESIAN_POINT('Ctrl Pts',(3.23028945793289,1.,-2.10758699642451));
#51857=CARTESIAN_POINT('Ctrl Pts',(3.23554444767099,1.,-2.11304604021773));
#51858=CARTESIAN_POINT('Ctrl Pts',(3.24074905517293,1.,-2.11854673326979));
#51859=CARTESIAN_POINT('Ctrl Pts',(3.24587102613376,1.,-2.12406646410962));
#51860=CARTESIAN_POINT('Ctrl Pts',(3.25090574494028,1.,-2.12960028396832));
#51861=CARTESIAN_POINT('Ctrl Pts',(3.25586495065054,1.,-2.13515375878803));
#51862=CARTESIAN_POINT('Ctrl Pts',(3.26077002641879,1.,-2.14073870754264));
#51863=CARTESIAN_POINT('Ctrl Pts',(3.26564388189759,1.,-2.1463680529566));
#51864=CARTESIAN_POINT('Ctrl Pts',(3.27050245897228,1.,-2.15205043199808));
#51865=CARTESIAN_POINT('Ctrl Pts',(3.27534954469187,1.,-2.15778690038347));
#51866=CARTESIAN_POINT('Ctrl Pts',(3.280181508414,1.,-2.16357391934425));
#51867=CARTESIAN_POINT('Ctrl Pts',(3.28499019979724,1.,-2.16940517773455));
#51868=CARTESIAN_POINT('Ctrl Pts',(3.28976645712568,1.,-2.17527380048423));
#51869=CARTESIAN_POINT('Ctrl Pts',(3.2945036150049,1.,-2.18117455557065));
#51870=CARTESIAN_POINT('Ctrl Pts',(3.29920022557639,1.,-2.18710556500327));
#51871=CARTESIAN_POINT('Ctrl Pts',(3.30385816281831,1.,-2.19306710376111));
#51872=CARTESIAN_POINT('Ctrl Pts',(3.30848134694595,1.,-2.19906078949923));
#51873=CARTESIAN_POINT('Ctrl Pts',(3.31307424608949,1.,-2.20508863150607));
#51874=CARTESIAN_POINT('Ctrl Pts',(3.31764044024235,1.,-2.21115211847875));
#51875=CARTESIAN_POINT('Ctrl Pts',(3.32218125618968,1.,-2.21725135110898));
#51876=CARTESIAN_POINT('Ctrl Pts',(3.3266964672289,1.,-2.22338548312772));
#51877=CARTESIAN_POINT('Ctrl Pts',(3.33118487773611,1.,-2.22955308907233));
#51878=CARTESIAN_POINT('Ctrl Pts',(3.33564495756481,1.,-2.23575256328812));
#51879=CARTESIAN_POINT('Ctrl Pts',(3.34007543738025,1.,-2.24198249391422));
#51880=CARTESIAN_POINT('Ctrl Pts',(3.34447596770723,1.,-2.24824207678256));
#51881=CARTESIAN_POINT('Ctrl Pts',(3.34884690292285,1.,-2.25453097693483));
#51882=CARTESIAN_POINT('Ctrl Pts',(3.35318902552626,1.,-2.26084915222449));
#51883=CARTESIAN_POINT('Ctrl Pts',(3.35750328523061,1.,-2.2671966857991));
#51884=CARTESIAN_POINT('Ctrl Pts',(3.36179055004409,1.,-2.2735736262093));
#51885=CARTESIAN_POINT('Ctrl Pts',(3.36605130713076,1.,-2.27997979458037));
#51886=CARTESIAN_POINT('Ctrl Pts',(3.37028570206488,1.,-2.28641481081137));
#51887=CARTESIAN_POINT('Ctrl Pts',(3.37449367172826,1.,-2.29287818007393));
#51888=CARTESIAN_POINT('Ctrl Pts',(3.37867504959433,1.,-2.29936936127624));
#51889=CARTESIAN_POINT('Ctrl Pts',(3.3828296733661,1.,-2.30588783640343));
#51890=CARTESIAN_POINT('Ctrl Pts',(3.38695751492462,1.,-2.31243319489367));
#51891=CARTESIAN_POINT('Ctrl Pts',(3.39105869474822,1.,-2.31900513925424));
#51892=CARTESIAN_POINT('Ctrl Pts',(3.39513342019756,1.,-2.3256034390248));
#51893=CARTESIAN_POINT('Ctrl Pts',(3.39918194577956,1.,-2.33222789882489));
#51894=CARTESIAN_POINT('Ctrl Pts',(3.40320452776743,1.,-2.33887832342782));
#51895=CARTESIAN_POINT('Ctrl Pts',(3.40720137404297,1.,-2.34555447649188));
#51896=CARTESIAN_POINT('Ctrl Pts',(3.41117262314119,1.,-2.35225606824109));
#51897=CARTESIAN_POINT('Ctrl Pts',(3.41511836751469,1.,-2.35898278606946));
#51898=CARTESIAN_POINT('Ctrl Pts',(3.41903866635852,1.,-2.36573431470642));
#51899=CARTESIAN_POINT('Ctrl Pts',(3.42293356216511,1.,-2.37251035954292));
#51900=CARTESIAN_POINT('Ctrl Pts',(3.42680309754399,1.,-2.37931067028926));
#51901=CARTESIAN_POINT('Ctrl Pts',(3.43064732712919,1.,-2.38613505843552));
#51902=CARTESIAN_POINT('Ctrl Pts',(3.4344663067854,1.,-2.39298338804493));
#51903=CARTESIAN_POINT('Ctrl Pts',(3.43750133064416,1.,-2.39848113410292));
#51904=CARTESIAN_POINT('Ctrl Pts',(3.43976627484234,1.,-2.40261515589405));
#51905=CARTESIAN_POINT('Ctrl Pts',(3.44127120683039,1.,-2.4053759295909));
#51906=CARTESIAN_POINT('Ctrl Pts',(3.44202241512147,1.,-2.40675750623143));
#51907=CARTESIAN_POINT('Origin',(3.44202241512147,0.,-2.40675750623143));
#51908=CARTESIAN_POINT('',(3.35260583073571,1.,-2.52982887637028));
#51909=CARTESIAN_POINT('Origin',(0.,0.,0.));
#51910=CARTESIAN_POINT('',(3.24413672884812,1.,-1.88097764062697));
#51911=CARTESIAN_POINT('Origin',(0.,1.,0.));
#51912=CARTESIAN_POINT('Ctrl Pts',(3.24413672884812,1.,-1.88097764062697));
#51913=CARTESIAN_POINT('Ctrl Pts',(3.24413672884812,0.666666666666667,-1.88097764062697));
#51914=CARTESIAN_POINT('Ctrl Pts',(3.24413672884812,0.333333333333333,-1.88097764062697));
#51915=CARTESIAN_POINT('Ctrl Pts',(3.24413672884812,-0.333333333333333,
-1.88097764062697));
#51916=CARTESIAN_POINT('Ctrl Pts',(3.24413672884812,-0.666666666666667,
-1.88097764062697));
#51917=CARTESIAN_POINT('Ctrl Pts',(3.24413672884812,-1.,-1.88097764062697));
#51918=CARTESIAN_POINT('Ctrl Pts',(3.70708211654725,-1.,-1.97421938526992));
#51919=CARTESIAN_POINT('Ctrl Pts',(3.70708211654725,1.,-1.97421938526992));
#51920=CARTESIAN_POINT('Ctrl Pts',(3.70551008132332,-1.,-1.97417727645308));
#51921=CARTESIAN_POINT('Ctrl Pts',(3.70551008132332,1.,-1.97417727645308));
#51922=CARTESIAN_POINT('Ctrl Pts',(3.70236698912904,-1.,-1.97408973726715));
#51923=CARTESIAN_POINT('Ctrl Pts',(3.70236698912904,1.,-1.97408973726715));
#51924=CARTESIAN_POINT('Ctrl Pts',(3.6976552856004,-1.,-1.97394846383216));
#51925=CARTESIAN_POINT('Ctrl Pts',(3.6976552856004,1.,-1.97394846383216));
#51926=CARTESIAN_POINT('Ctrl Pts',(3.69137888599902,-1.,-1.97374016225483));
#51927=CARTESIAN_POINT('Ctrl Pts',(3.69137888599902,1.,-1.97374016225483));
#51928=CARTESIAN_POINT('Ctrl Pts',(3.68354319915092,-1.,-1.97344650304519));
#51929=CARTESIAN_POINT('Ctrl Pts',(3.68354319915092,1.,-1.97344650304519));
#51930=CARTESIAN_POINT('Ctrl Pts',(3.67571738107084,-1.,-1.97311947678517));
#51931=CARTESIAN_POINT('Ctrl Pts',(3.67571738107084,1.,-1.97311947678517));
#51932=CARTESIAN_POINT('Ctrl Pts',(3.66790152752075,-1.,-1.97275897198678));
#51933=CARTESIAN_POINT('Ctrl Pts',(3.66790152752075,1.,-1.97275897198678));
#51934=CARTESIAN_POINT('Ctrl Pts',(3.6600957816636,-1.,-1.9723648543905));
#51935=CARTESIAN_POINT('Ctrl Pts',(3.6600957816636,1.,-1.9723648543905));
#51936=CARTESIAN_POINT('Ctrl Pts',(3.652300347166,-1.,-1.9719369724024));
#51937=CARTESIAN_POINT('Ctrl Pts',(3.652300347166,1.,-1.9719369724024));
#51938=CARTESIAN_POINT('Ctrl Pts',(3.64451546723514,-1.,-1.97147515441164));
#51939=CARTESIAN_POINT('Ctrl Pts',(3.64451546723514,1.,-1.97147515441164));
#51940=CARTESIAN_POINT('Ctrl Pts',(3.63674139590412,-1.,-1.97097920454464));
#51941=CARTESIAN_POINT('Ctrl Pts',(3.63674139590412,1.,-1.97097920454464));
#51942=CARTESIAN_POINT('Ctrl Pts',(3.62897836973293,-1.,-1.97044889850463));
#51943=CARTESIAN_POINT('Ctrl Pts',(3.62897836973293,1.,-1.97044889850463));
#51944=CARTESIAN_POINT('Ctrl Pts',(3.62122658401893,-1.,-1.96988398129978));
#51945=CARTESIAN_POINT('Ctrl Pts',(3.62122658401893,1.,-1.96988398129978));
#51946=CARTESIAN_POINT('Ctrl Pts',(3.61348615496704,-1.,-1.96928416040877));
#51947=CARTESIAN_POINT('Ctrl Pts',(3.61348615496704,1.,-1.96928416040877));
#51948=CARTESIAN_POINT('Ctrl Pts',(3.60575714017989,-1.,-1.9686491188594));
#51949=CARTESIAN_POINT('Ctrl Pts',(3.60575714017989,1.,-1.9686491188594));
#51950=CARTESIAN_POINT('Ctrl Pts',(3.59803959819938,-1.,-1.96797854118369));
#51951=CARTESIAN_POINT('Ctrl Pts',(3.59803959819938,1.,-1.96797854118369));
#51952=CARTESIAN_POINT('Ctrl Pts',(3.59033364022801,-1.,-1.96727213799544));
#51953=CARTESIAN_POINT('Ctrl Pts',(3.59033364022801,1.,-1.96727213799544));
#51954=CARTESIAN_POINT('Ctrl Pts',(3.58263947663829,-1.,-1.96652966688911));
#51955=CARTESIAN_POINT('Ctrl Pts',(3.58263947663829,1.,-1.96652966688911));
#51956=CARTESIAN_POINT('Ctrl Pts',(3.57495748600959,-1.,-1.96575096652789));
#51957=CARTESIAN_POINT('Ctrl Pts',(3.57495748600959,1.,-1.96575096652789));
#51958=CARTESIAN_POINT('Ctrl Pts',(3.56728820357791,-1.,-1.96493594634567));
#51959=CARTESIAN_POINT('Ctrl Pts',(3.56728820357791,1.,-1.96493594634567));
#51960=CARTESIAN_POINT('Ctrl Pts',(3.55963218706096,-1.,-1.96408450906812));
#51961=CARTESIAN_POINT('Ctrl Pts',(3.55963218706096,1.,-1.96408450906812));
#51962=CARTESIAN_POINT('Ctrl Pts',(3.55198990600886,-1.,-1.96319648628644));
#51963=CARTESIAN_POINT('Ctrl Pts',(3.55198990600886,1.,-1.96319648628644));
#51964=CARTESIAN_POINT('Ctrl Pts',(3.54436163300443,-1.,-1.96227157573067));
#51965=CARTESIAN_POINT('Ctrl Pts',(3.54436163300443,1.,-1.96227157573067));
#51966=CARTESIAN_POINT('Ctrl Pts',(3.53674730625813,-1.,-1.96130926212689));
#51967=CARTESIAN_POINT('Ctrl Pts',(3.53674730625813,1.,-1.96130926212689));
#51968=CARTESIAN_POINT('Ctrl Pts',(3.52914648844351,-1.,-1.96030879411566));
#51969=CARTESIAN_POINT('Ctrl Pts',(3.52914648844351,1.,-1.96030879411566));
#51970=CARTESIAN_POINT('Ctrl Pts',(3.52155867431486,-1.,-1.95926936324461));
#51971=CARTESIAN_POINT('Ctrl Pts',(3.52155867431486,1.,-1.95926936324461));
#51972=CARTESIAN_POINT('Ctrl Pts',(3.51398354617794,-1.,-1.95819025316779));
#51973=CARTESIAN_POINT('Ctrl Pts',(3.51398354617794,1.,-1.95819025316779));
#51974=CARTESIAN_POINT('Ctrl Pts',(3.50642124159909,-1.,-1.95707099606511));
#51975=CARTESIAN_POINT('Ctrl Pts',(3.50642124159909,1.,-1.95707099606511));
#51976=CARTESIAN_POINT('Ctrl Pts',(3.49887263575583,-1.,-1.95591153823661));
#51977=CARTESIAN_POINT('Ctrl Pts',(3.49887263575583,1.,-1.95591153823661));
#51978=CARTESIAN_POINT('Ctrl Pts',(3.49133956289133,-1.,-1.95471236969643));
#51979=CARTESIAN_POINT('Ctrl Pts',(3.49133956289133,1.,-1.95471236969643));
#51980=CARTESIAN_POINT('Ctrl Pts',(3.48382414832634,-1.,-1.95347412486309));
#51981=CARTESIAN_POINT('Ctrl Pts',(3.48382414832634,1.,-1.95347412486309));
#51982=CARTESIAN_POINT('Ctrl Pts',(3.47632820495921,-1.,-1.95219722189876));
#51983=CARTESIAN_POINT('Ctrl Pts',(3.47632820495921,1.,-1.95219722189876));
#51984=CARTESIAN_POINT('Ctrl Pts',(3.46885258974191,-1.,-1.95088147859877));
#51985=CARTESIAN_POINT('Ctrl Pts',(3.46885258974191,1.,-1.95088147859877));
#51986=CARTESIAN_POINT('Ctrl Pts',(3.46139661060962,-1.,-1.94952575850197));
#51987=CARTESIAN_POINT('Ctrl Pts',(3.46139661060962,1.,-1.94952575850197));
#51988=CARTESIAN_POINT('Ctrl Pts',(3.45395731584051,-1.,-1.94812754766524));
#51989=CARTESIAN_POINT('Ctrl Pts',(3.45395731584051,1.,-1.94812754766524));
#51990=CARTESIAN_POINT('Ctrl Pts',(3.44653088665681,-1.,-1.94668377715329));
#51991=CARTESIAN_POINT('Ctrl Pts',(3.44653088665681,1.,-1.94668377715329));
#51992=CARTESIAN_POINT('Ctrl Pts',(3.43911410197687,-1.,-1.94519168842879));
#51993=CARTESIAN_POINT('Ctrl Pts',(3.43911410197687,1.,-1.94519168842879));
#51994=CARTESIAN_POINT('Ctrl Pts',(3.43170586602434,-1.,-1.94364973660284));
#51995=CARTESIAN_POINT('Ctrl Pts',(3.43170586602434,1.,-1.94364973660284));
#51996=CARTESIAN_POINT('Ctrl Pts',(3.42430850941503,-1.,-1.94205835913696));
#51997=CARTESIAN_POINT('Ctrl Pts',(3.42430850941503,1.,-1.94205835913696));
#51998=CARTESIAN_POINT('Ctrl Pts',(3.41692971994096,-1.,-1.94042111965246));
#51999=CARTESIAN_POINT('Ctrl Pts',(3.41692971994096,1.,-1.94042111965246));
#52000=CARTESIAN_POINT('Ctrl Pts',(3.40957978266642,-1.,-1.93874306008143));
#52001=CARTESIAN_POINT('Ctrl Pts',(3.40957978266642,1.,-1.93874306008143));
#52002=CARTESIAN_POINT('Ctrl Pts',(3.40226802104109,-1.,-1.93702857723098));
#52003=CARTESIAN_POINT('Ctrl Pts',(3.40226802104109,1.,-1.93702857723098));
#52004=CARTESIAN_POINT('Ctrl Pts',(3.39499923640795,-1.,-1.93527929945985));
#52005=CARTESIAN_POINT('Ctrl Pts',(3.39499923640795,1.,-1.93527929945985));
#52006=CARTESIAN_POINT('Ctrl Pts',(3.38777076883256,-1.,-1.93349233176788));
#52007=CARTESIAN_POINT('Ctrl Pts',(3.38777076883256,1.,-1.93349233176788));
#52008=CARTESIAN_POINT('Ctrl Pts',(3.3805676852555,-1.,-1.93165739093276));
#52009=CARTESIAN_POINT('Ctrl Pts',(3.3805676852555,1.,-1.93165739093276));
#52010=CARTESIAN_POINT('Ctrl Pts',(3.37336807068043,-1.,-1.92975993109877));
#52011=CARTESIAN_POINT('Ctrl Pts',(3.37336807068043,1.,-1.92975993109877));
#52012=CARTESIAN_POINT('Ctrl Pts',(3.36615168657567,-1.,-1.92778626543786));
#52013=CARTESIAN_POINT('Ctrl Pts',(3.36615168657567,1.,-1.92778626543786));
#52014=CARTESIAN_POINT('Ctrl Pts',(3.35890824422965,-1.,-1.92572846125756));
#52015=CARTESIAN_POINT('Ctrl Pts',(3.35890824422965,1.,-1.92572846125756));
#52016=CARTESIAN_POINT('Ctrl Pts',(3.35164424847223,-1.,-1.92358838440528));
#52017=CARTESIAN_POINT('Ctrl Pts',(3.35164424847223,1.,-1.92358838440528));
#52018=CARTESIAN_POINT('Ctrl Pts',(3.34439448941961,-1.,-1.92138450828404));
#52019=CARTESIAN_POINT('Ctrl Pts',(3.34439448941961,1.,-1.92138450828404));
#52020=CARTESIAN_POINT('Ctrl Pts',(3.33721230710012,-1.,-1.9191460961021));
#52021=CARTESIAN_POINT('Ctrl Pts',(3.33721230710012,1.,-1.9191460961021));
#52022=CARTESIAN_POINT('Ctrl Pts',(3.33014884257873,-1.,-1.91690081930332));
#52023=CARTESIAN_POINT('Ctrl Pts',(3.33014884257873,1.,-1.91690081930332));
#52024=CARTESIAN_POINT('Ctrl Pts',(3.32323403454535,-1.,-1.91466343916628));
#52025=CARTESIAN_POINT('Ctrl Pts',(3.32323403454535,1.,-1.91466343916628));
#52026=CARTESIAN_POINT('Ctrl Pts',(3.31646052426364,-1.,-1.91242616234442));
#52027=CARTESIAN_POINT('Ctrl Pts',(3.31646052426364,1.,-1.91242616234442));
#52028=CARTESIAN_POINT('Ctrl Pts',(3.30975721158596,-1.,-1.91014297830446));
#52029=CARTESIAN_POINT('Ctrl Pts',(3.30975721158596,1.,-1.91014297830446));
#52030=CARTESIAN_POINT('Ctrl Pts',(3.30300595568195,-1.,-1.90773912171341));
#52031=CARTESIAN_POINT('Ctrl Pts',(3.30300595568195,1.,-1.90773912171341));
#52032=CARTESIAN_POINT('Ctrl Pts',(3.29608978722113,-1.,-1.90513891864087));
#52033=CARTESIAN_POINT('Ctrl Pts',(3.29608978722113,1.,-1.90513891864087));
#52034=CARTESIAN_POINT('Ctrl Pts',(3.2889344860029,-1.,-1.90228971247527));
#52035=CARTESIAN_POINT('Ctrl Pts',(3.2889344860029,1.,-1.90228971247527));
#52036=CARTESIAN_POINT('Ctrl Pts',(3.28154737912352,-1.,-1.89918429230462));
#52037=CARTESIAN_POINT('Ctrl Pts',(3.28154737912352,1.,-1.89918429230462));
#52038=CARTESIAN_POINT('Ctrl Pts',(3.27407108933139,-1.,-1.89589172903793));
#52039=CARTESIAN_POINT('Ctrl Pts',(3.27407108933139,1.,-1.89589172903793));
#52040=CARTESIAN_POINT('Ctrl Pts',(3.26677653888676,-1.,-1.89255393500965));
#52041=CARTESIAN_POINT('Ctrl Pts',(3.26677653888676,1.,-1.89255393500965));
#52042=CARTESIAN_POINT('Ctrl Pts',(3.25999885193947,-1.,-1.88934996203698));
#52043=CARTESIAN_POINT('Ctrl Pts',(3.25999885193947,1.,-1.88934996203698));
#52044=CARTESIAN_POINT('Ctrl Pts',(3.25408686339463,-1.,-1.88646802523466));
#52045=CARTESIAN_POINT('Ctrl Pts',(3.25408686339463,1.,-1.88646802523466));
#52046=CARTESIAN_POINT('Ctrl Pts',(3.24935200511918,-1.,-1.88407708646357));
#52047=CARTESIAN_POINT('Ctrl Pts',(3.24935200511918,1.,-1.88407708646357));
#52048=CARTESIAN_POINT('Ctrl Pts',(3.24600543790443,-1.,-1.88229202582941));
#52049=CARTESIAN_POINT('Ctrl Pts',(3.24600543790443,1.,-1.88229202582941));
#52050=CARTESIAN_POINT('Ctrl Pts',(3.24451807186481,-1.,-1.88139187908074));
#52051=CARTESIAN_POINT('Ctrl Pts',(3.24451807186481,1.,-1.88139187908074));
#52052=CARTESIAN_POINT('Ctrl Pts',(3.24408699284121,-1.,-1.88102201872555));
#52053=CARTESIAN_POINT('Ctrl Pts',(3.24408699284121,1.,-1.88102201872555));
#52054=CARTESIAN_POINT('Ctrl Pts',(3.24410359189609,-1.,-1.88091100680349));
#52055=CARTESIAN_POINT('Ctrl Pts',(3.24410359189609,1.,-1.88091100680349));
#52056=CARTESIAN_POINT('Ctrl Pts',(3.24418789321065,-1.,-1.8808893942881));
#52057=CARTESIAN_POINT('Ctrl Pts',(3.24418789321065,1.,-1.8808893942881));
#52058=CARTESIAN_POINT('',(3.70708211654725,1.,-1.97421938526992));
#52059=CARTESIAN_POINT('Ctrl Pts',(3.70708211654725,1.,-1.97421938526992));
#52060=CARTESIAN_POINT('Ctrl Pts',(3.70551008132332,1.,-1.97417727645308));
#52061=CARTESIAN_POINT('Ctrl Pts',(3.70236698912904,1.,-1.97408973726715));
#52062=CARTESIAN_POINT('Ctrl Pts',(3.6976552856004,1.,-1.97394846383216));
#52063=CARTESIAN_POINT('Ctrl Pts',(3.69137888599902,1.,-1.97374016225483));
#52064=CARTESIAN_POINT('Ctrl Pts',(3.68354319915092,1.,-1.97344650304519));
#52065=CARTESIAN_POINT('Ctrl Pts',(3.67571738107084,1.,-1.97311947678517));
#52066=CARTESIAN_POINT('Ctrl Pts',(3.66790152752075,1.,-1.97275897198678));
#52067=CARTESIAN_POINT('Ctrl Pts',(3.6600957816636,1.,-1.9723648543905));
#52068=CARTESIAN_POINT('Ctrl Pts',(3.652300347166,1.,-1.9719369724024));
#52069=CARTESIAN_POINT('Ctrl Pts',(3.64451546723514,1.,-1.97147515441164));
#52070=CARTESIAN_POINT('Ctrl Pts',(3.63674139590412,1.,-1.97097920454464));
#52071=CARTESIAN_POINT('Ctrl Pts',(3.62897836973293,1.,-1.97044889850463));
#52072=CARTESIAN_POINT('Ctrl Pts',(3.62122658401893,1.,-1.96988398129978));
#52073=CARTESIAN_POINT('Ctrl Pts',(3.61348615496704,1.,-1.96928416040877));
#52074=CARTESIAN_POINT('Ctrl Pts',(3.60575714017989,1.,-1.9686491188594));
#52075=CARTESIAN_POINT('Ctrl Pts',(3.59803959819938,1.,-1.96797854118369));
#52076=CARTESIAN_POINT('Ctrl Pts',(3.59033364022801,1.,-1.96727213799544));
#52077=CARTESIAN_POINT('Ctrl Pts',(3.58263947663829,1.,-1.96652966688911));
#52078=CARTESIAN_POINT('Ctrl Pts',(3.57495748600959,1.,-1.96575096652789));
#52079=CARTESIAN_POINT('Ctrl Pts',(3.56728820357791,1.,-1.96493594634567));
#52080=CARTESIAN_POINT('Ctrl Pts',(3.55963218706096,1.,-1.96408450906812));
#52081=CARTESIAN_POINT('Ctrl Pts',(3.55198990600886,1.,-1.96319648628644));
#52082=CARTESIAN_POINT('Ctrl Pts',(3.54436163300443,1.,-1.96227157573067));
#52083=CARTESIAN_POINT('Ctrl Pts',(3.53674730625813,1.,-1.96130926212689));
#52084=CARTESIAN_POINT('Ctrl Pts',(3.52914648844351,1.,-1.96030879411566));
#52085=CARTESIAN_POINT('Ctrl Pts',(3.52155867431486,1.,-1.95926936324461));
#52086=CARTESIAN_POINT('Ctrl Pts',(3.51398354617794,1.,-1.95819025316779));
#52087=CARTESIAN_POINT('Ctrl Pts',(3.50642124159909,1.,-1.95707099606511));
#52088=CARTESIAN_POINT('Ctrl Pts',(3.49887263575583,1.,-1.95591153823661));
#52089=CARTESIAN_POINT('Ctrl Pts',(3.49133956289133,1.,-1.95471236969643));
#52090=CARTESIAN_POINT('Ctrl Pts',(3.48382414832634,1.,-1.95347412486309));
#52091=CARTESIAN_POINT('Ctrl Pts',(3.47632820495921,1.,-1.95219722189876));
#52092=CARTESIAN_POINT('Ctrl Pts',(3.46885258974191,1.,-1.95088147859877));
#52093=CARTESIAN_POINT('Ctrl Pts',(3.46139661060962,1.,-1.94952575850197));
#52094=CARTESIAN_POINT('Ctrl Pts',(3.45395731584051,1.,-1.94812754766524));
#52095=CARTESIAN_POINT('Ctrl Pts',(3.44653088665681,1.,-1.94668377715329));
#52096=CARTESIAN_POINT('Ctrl Pts',(3.43911410197687,1.,-1.94519168842879));
#52097=CARTESIAN_POINT('Ctrl Pts',(3.43170586602434,1.,-1.94364973660284));
#52098=CARTESIAN_POINT('Ctrl Pts',(3.42430850941503,1.,-1.94205835913696));
#52099=CARTESIAN_POINT('Ctrl Pts',(3.41692971994096,1.,-1.94042111965246));
#52100=CARTESIAN_POINT('Ctrl Pts',(3.40957978266642,1.,-1.93874306008143));
#52101=CARTESIAN_POINT('Ctrl Pts',(3.40226802104109,1.,-1.93702857723098));
#52102=CARTESIAN_POINT('Ctrl Pts',(3.39499923640795,1.,-1.93527929945985));
#52103=CARTESIAN_POINT('Ctrl Pts',(3.38777076883256,1.,-1.93349233176788));
#52104=CARTESIAN_POINT('Ctrl Pts',(3.3805676852555,1.,-1.93165739093276));
#52105=CARTESIAN_POINT('Ctrl Pts',(3.37336807068043,1.,-1.92975993109877));
#52106=CARTESIAN_POINT('Ctrl Pts',(3.36615168657567,1.,-1.92778626543786));
#52107=CARTESIAN_POINT('Ctrl Pts',(3.35890824422965,1.,-1.92572846125756));
#52108=CARTESIAN_POINT('Ctrl Pts',(3.35164424847223,1.,-1.92358838440528));
#52109=CARTESIAN_POINT('Ctrl Pts',(3.34439448941961,1.,-1.92138450828404));
#52110=CARTESIAN_POINT('Ctrl Pts',(3.33721230710012,1.,-1.9191460961021));
#52111=CARTESIAN_POINT('Ctrl Pts',(3.33014884257873,1.,-1.91690081930332));
#52112=CARTESIAN_POINT('Ctrl Pts',(3.32323403454535,1.,-1.91466343916628));
#52113=CARTESIAN_POINT('Ctrl Pts',(3.31646052426364,1.,-1.91242616234442));
#52114=CARTESIAN_POINT('Ctrl Pts',(3.30975721158596,1.,-1.91014297830446));
#52115=CARTESIAN_POINT('Ctrl Pts',(3.30300595568195,1.,-1.90773912171341));
#52116=CARTESIAN_POINT('Ctrl Pts',(3.29608978722113,1.,-1.90513891864087));
#52117=CARTESIAN_POINT('Ctrl Pts',(3.2889344860029,1.,-1.90228971247527));
#52118=CARTESIAN_POINT('Ctrl Pts',(3.28154737912352,1.,-1.89918429230462));
#52119=CARTESIAN_POINT('Ctrl Pts',(3.27407108933139,1.,-1.89589172903793));
#52120=CARTESIAN_POINT('Ctrl Pts',(3.26677653888676,1.,-1.89255393500965));
#52121=CARTESIAN_POINT('Ctrl Pts',(3.25999885193947,1.,-1.88934996203698));
#52122=CARTESIAN_POINT('Ctrl Pts',(3.25408686339463,1.,-1.88646802523466));
#52123=CARTESIAN_POINT('Ctrl Pts',(3.24935200511918,1.,-1.88407708646357));
#52124=CARTESIAN_POINT('Ctrl Pts',(3.2462565441079,1.,-1.88242596600454));
#52125=CARTESIAN_POINT('Ctrl Pts',(3.24480754676064,1.,-1.88156537699203));
#52126=CARTESIAN_POINT('Ctrl Pts',(3.24428080353022,1.,-1.88117508446775));
#52127=CARTESIAN_POINT('Ctrl Pts',(3.24415531671284,1.,-1.8810229239812));
#52128=CARTESIAN_POINT('Ctrl Pts',(3.24413672884812,1.,-1.88097764062697));
#52129=CARTESIAN_POINT('',(3.70708211654725,0.,-1.97421938526992));
#52130=CARTESIAN_POINT('Ctrl Pts',(3.42855728381368,-1.,-1.519044091397));
#52131=CARTESIAN_POINT('Ctrl Pts',(3.42855728381368,1.,-1.519044091397));
#52132=CARTESIAN_POINT('Ctrl Pts',(3.42852521763778,-1.,-1.51896318668366));
#52133=CARTESIAN_POINT('Ctrl Pts',(3.42852521763778,1.,-1.51896318668366));
#52134=CARTESIAN_POINT('Ctrl Pts',(3.42860527149177,-1.,-1.51888450659652));
#52135=CARTESIAN_POINT('Ctrl Pts',(3.42860527149177,1.,-1.51888450659652));
#52136=CARTESIAN_POINT('Ctrl Pts',(3.42915787669893,-1.,-1.51901585839109));
#52137=CARTESIAN_POINT('Ctrl Pts',(3.42915787669893,1.,-1.51901585839109));
#52138=CARTESIAN_POINT('Ctrl Pts',(3.43076036253837,-1.,-1.51969006980999));
#52139=CARTESIAN_POINT('Ctrl Pts',(3.43076036253837,1.,-1.51969006980999));
#52140=CARTESIAN_POINT('Ctrl Pts',(3.43417156977893,-1.,-1.52134826724293));
#52141=CARTESIAN_POINT('Ctrl Pts',(3.43417156977893,1.,-1.52134826724293));
#52142=CARTESIAN_POINT('Ctrl Pts',(3.4388889597401,-1.,-1.5237734895035));
#52143=CARTESIAN_POINT('Ctrl Pts',(3.4388889597401,1.,-1.5237734895035));
#52144=CARTESIAN_POINT('Ctrl Pts',(3.44469547526647,-1.,-1.52686242875556));
#52145=CARTESIAN_POINT('Ctrl Pts',(3.44469547526647,1.,-1.52686242875556));
#52146=CARTESIAN_POINT('Ctrl Pts',(3.45127136828305,-1.,-1.53046244461635));
#52147=CARTESIAN_POINT('Ctrl Pts',(3.45127136828305,1.,-1.53046244461635));
#52148=CARTESIAN_POINT('Ctrl Pts',(3.45825932955032,-1.,-1.53440195378792));
#52149=CARTESIAN_POINT('Ctrl Pts',(3.45825932955032,1.,-1.53440195378792));
#52150=CARTESIAN_POINT('Ctrl Pts',(3.46531752207153,-1.,-1.53851507915502));
#52151=CARTESIAN_POINT('Ctrl Pts',(3.46531752207153,1.,-1.53851507915502));
#52152=CARTESIAN_POINT('Ctrl Pts',(3.47217189224653,-1.,-1.54266605398188));
#52153=CARTESIAN_POINT('Ctrl Pts',(3.47217189224653,1.,-1.54266605398188));
#52154=CARTESIAN_POINT('Ctrl Pts',(3.47868272898751,-1.,-1.54678009290276));
#52155=CARTESIAN_POINT('Ctrl Pts',(3.47868272898751,1.,-1.54678009290276));
#52156=CARTESIAN_POINT('Ctrl Pts',(3.48485155928567,-1.,-1.55084702970452));
#52157=CARTESIAN_POINT('Ctrl Pts',(3.48485155928567,1.,-1.55084702970452));
#52158=CARTESIAN_POINT('Ctrl Pts',(3.4907646087742,-1.,-1.55489595901116));
#52159=CARTESIAN_POINT('Ctrl Pts',(3.4907646087742,1.,-1.55489595901116));
#52160=CARTESIAN_POINT('Ctrl Pts',(3.49655185179655,-1.,-1.55897703097874));
#52161=CARTESIAN_POINT('Ctrl Pts',(3.49655185179655,1.,-1.55897703097874));
#52162=CARTESIAN_POINT('Ctrl Pts',(3.50234321621578,-1.,-1.56314187758675));
#52163=CARTESIAN_POINT('Ctrl Pts',(3.50234321621578,1.,-1.56314187758675));
#52164=CARTESIAN_POINT('Ctrl Pts',(3.50821771695363,-1.,-1.56742097575012));
#52165=CARTESIAN_POINT('Ctrl Pts',(3.50821771695363,1.,-1.56742097575012));
#52166=CARTESIAN_POINT('Ctrl Pts',(3.51418598431665,-1.,-1.57181569799743));
#52167=CARTESIAN_POINT('Ctrl Pts',(3.51418598431665,1.,-1.57181569799743));
#52168=CARTESIAN_POINT('Ctrl Pts',(3.52021847865912,-1.,-1.57631049988158));
#52169=CARTESIAN_POINT('Ctrl Pts',(3.52021847865912,1.,-1.57631049988158));
#52170=CARTESIAN_POINT('Ctrl Pts',(3.52626275334881,-1.,-1.58088027227848));
#52171=CARTESIAN_POINT('Ctrl Pts',(3.52626275334881,1.,-1.58088027227848));
#52172=CARTESIAN_POINT('Ctrl Pts',(3.5322637814708,-1.,-1.58549906268088));
#52173=CARTESIAN_POINT('Ctrl Pts',(3.5322637814708,1.,-1.58549906268088));
#52174=CARTESIAN_POINT('Ctrl Pts',(3.53818616861077,-1.,-1.59014958368739));
#52175=CARTESIAN_POINT('Ctrl Pts',(3.53818616861077,1.,-1.59014958368739));
#52176=CARTESIAN_POINT('Ctrl Pts',(3.54402458182337,-1.,-1.59482766949766));
#52177=CARTESIAN_POINT('Ctrl Pts',(3.54402458182337,1.,-1.59482766949766));
#52178=CARTESIAN_POINT('Ctrl Pts',(3.54979148634454,-1.,-1.59953698113457));
#52179=CARTESIAN_POINT('Ctrl Pts',(3.54979148634454,1.,-1.59953698113457));
#52180=CARTESIAN_POINT('Ctrl Pts',(3.55550985096129,-1.,-1.60428584699853));
#52181=CARTESIAN_POINT('Ctrl Pts',(3.55550985096129,1.,-1.60428584699853));
#52182=CARTESIAN_POINT('Ctrl Pts',(3.5612043248298,-1.,-1.60908344685457));
#52183=CARTESIAN_POINT('Ctrl Pts',(3.5612043248298,1.,-1.60908344685457));
#52184=CARTESIAN_POINT('Ctrl Pts',(3.56689200468387,-1.,-1.61393581747514));
#52185=CARTESIAN_POINT('Ctrl Pts',(3.56689200468387,1.,-1.61393581747514));
#52186=CARTESIAN_POINT('Ctrl Pts',(3.57257679609806,-1.,-1.61884340915404));
#52187=CARTESIAN_POINT('Ctrl Pts',(3.57257679609806,1.,-1.61884340915404));
#52188=CARTESIAN_POINT('Ctrl Pts',(3.5782545595439,-1.,-1.62380329464844));
#52189=CARTESIAN_POINT('Ctrl Pts',(3.5782545595439,1.,-1.62380329464844));
#52190=CARTESIAN_POINT('Ctrl Pts',(3.58391625774343,-1.,-1.62881051550745));
#52191=CARTESIAN_POINT('Ctrl Pts',(3.58391625774343,1.,-1.62881051550745));
#52192=CARTESIAN_POINT('Ctrl Pts',(3.58955176627879,-1.,-1.6338597145126));
#52193=CARTESIAN_POINT('Ctrl Pts',(3.58955176627879,1.,-1.6338597145126));
#52194=CARTESIAN_POINT('Ctrl Pts',(3.59515368334893,-1.,-1.63894676675352));
#52195=CARTESIAN_POINT('Ctrl Pts',(3.59515368334893,1.,-1.63894676675352));
#52196=CARTESIAN_POINT('Ctrl Pts',(3.60072028513845,-1.,-1.64407004385582));
#52197=CARTESIAN_POINT('Ctrl Pts',(3.60072028513845,1.,-1.64407004385582));
#52198=CARTESIAN_POINT('Ctrl Pts',(3.60625346556992,-1.,-1.64922952425832));
#52199=CARTESIAN_POINT('Ctrl Pts',(3.60625346556992,1.,-1.64922952425832));
#52200=CARTESIAN_POINT('Ctrl Pts',(3.61175734965127,-1.,-1.65442619244325));
#52201=CARTESIAN_POINT('Ctrl Pts',(3.61175734965127,1.,-1.65442619244325));
#52202=CARTESIAN_POINT('Ctrl Pts',(3.61723666482456,-1.,-1.65966133399186));
#52203=CARTESIAN_POINT('Ctrl Pts',(3.61723666482456,1.,-1.65966133399186));
#52204=CARTESIAN_POINT('Ctrl Pts',(3.62269517989109,-1.,-1.66493585923855));
#52205=CARTESIAN_POINT('Ctrl Pts',(3.62269517989109,1.,-1.66493585923855));
#52206=CARTESIAN_POINT('Ctrl Pts',(3.62813422105271,-1.,-1.67024966008045));
#52207=CARTESIAN_POINT('Ctrl Pts',(3.62813422105271,1.,-1.67024966008045));
#52208=CARTESIAN_POINT('Ctrl Pts',(3.63355343201232,-1.,-1.67560193613156));
#52209=CARTESIAN_POINT('Ctrl Pts',(3.63355343201232,1.,-1.67560193613156));
#52210=CARTESIAN_POINT('Ctrl Pts',(3.63895140887462,-1.,-1.68099146651586));
#52211=CARTESIAN_POINT('Ctrl Pts',(3.63895140887462,1.,-1.68099146651586));
#52212=CARTESIAN_POINT('Ctrl Pts',(3.64432638915203,-1.,-1.68641690471457));
#52213=CARTESIAN_POINT('Ctrl Pts',(3.64432638915203,1.,-1.68641690471457));
#52214=CARTESIAN_POINT('Ctrl Pts',(3.64967689827371,-1.,-1.69187705481689));
#52215=CARTESIAN_POINT('Ctrl Pts',(3.64967689827371,1.,-1.69187705481689));
#52216=CARTESIAN_POINT('Ctrl Pts',(3.65500246526749,-1.,-1.69737117722534));
#52217=CARTESIAN_POINT('Ctrl Pts',(3.65500246526749,1.,-1.69737117722534));
#52218=CARTESIAN_POINT('Ctrl Pts',(3.66030338774847,-1.,-1.70289888566873));
#52219=CARTESIAN_POINT('Ctrl Pts',(3.66030338774847,1.,-1.70289888566873));
#52220=CARTESIAN_POINT('Ctrl Pts',(3.66558043198876,-1.,-1.70846001610956));
#52221=CARTESIAN_POINT('Ctrl Pts',(3.66558043198876,1.,-1.70846001610956));
#52222=CARTESIAN_POINT('Ctrl Pts',(3.67083454901611,-1.,-1.71405450210384));
#52223=CARTESIAN_POINT('Ctrl Pts',(3.67083454901611,1.,-1.71405450210384));
#52224=CARTESIAN_POINT('Ctrl Pts',(3.67606660374709,-1.,-1.71968225581808));
#52225=CARTESIAN_POINT('Ctrl Pts',(3.67606660374709,1.,-1.71968225581808));
#52226=CARTESIAN_POINT('Ctrl Pts',(3.68127704936579,-1.,-1.72534302437056));
#52227=CARTESIAN_POINT('Ctrl Pts',(3.68127704936579,1.,-1.72534302437056));
#52228=CARTESIAN_POINT('Ctrl Pts',(3.68646597019332,-1.,-1.73103640956717));
#52229=CARTESIAN_POINT('Ctrl Pts',(3.68646597019332,1.,-1.73103640956717));
#52230=CARTESIAN_POINT('Ctrl Pts',(3.69163322648036,-1.,-1.73676193254557));
#52231=CARTESIAN_POINT('Ctrl Pts',(3.69163322648036,1.,-1.73676193254557));
#52232=CARTESIAN_POINT('Ctrl Pts',(3.69677856910517,-1.,-1.74251908492617));
#52233=CARTESIAN_POINT('Ctrl Pts',(3.69677856910517,1.,-1.74251908492617));
#52234=CARTESIAN_POINT('Ctrl Pts',(3.7019017567335,-1.,-1.74830738046057));
#52235=CARTESIAN_POINT('Ctrl Pts',(3.7019017567335,1.,-1.74830738046057));
#52236=CARTESIAN_POINT('Ctrl Pts',(3.70700269736659,-1.,-1.75412641804042));
#52237=CARTESIAN_POINT('Ctrl Pts',(3.70700269736659,1.,-1.75412641804042));
#52238=CARTESIAN_POINT('Ctrl Pts',(3.71208146346136,-1.,-1.75997588498865));
#52239=CARTESIAN_POINT('Ctrl Pts',(3.71208146346136,1.,-1.75997588498865));
#52240=CARTESIAN_POINT('Ctrl Pts',(3.71713822377359,-1.,-1.76585552124394));
#52241=CARTESIAN_POINT('Ctrl Pts',(3.71713822377359,1.,-1.76585552124394));
#52242=CARTESIAN_POINT('Ctrl Pts',(3.72217319911254,-1.,-1.77176509401761));
#52243=CARTESIAN_POINT('Ctrl Pts',(3.72217319911254,1.,-1.77176509401761));
#52244=CARTESIAN_POINT('Ctrl Pts',(3.72718661205609,-1.,-1.77770437039658));
#52245=CARTESIAN_POINT('Ctrl Pts',(3.72718661205609,1.,-1.77770437039658));
#52246=CARTESIAN_POINT('Ctrl Pts',(3.7321786309547,-1.,-1.78367308442901));
#52247=CARTESIAN_POINT('Ctrl Pts',(3.7321786309547,1.,-1.78367308442901));
#52248=CARTESIAN_POINT('Ctrl Pts',(3.73714934730681,-1.,-1.78967092823491));
#52249=CARTESIAN_POINT('Ctrl Pts',(3.73714934730681,1.,-1.78967092823491));
#52250=CARTESIAN_POINT('Ctrl Pts',(3.74209880352445,-1.,-1.79569757859422));
#52251=CARTESIAN_POINT('Ctrl Pts',(3.74209880352445,1.,-1.79569757859422));
#52252=CARTESIAN_POINT('Ctrl Pts',(3.74702700875467,-1.,-1.8017527148577));
#52253=CARTESIAN_POINT('Ctrl Pts',(3.74702700875467,1.,-1.8017527148577));
#52254=CARTESIAN_POINT('Ctrl Pts',(3.75193395887977,-1.,-1.80783603939617));
#52255=CARTESIAN_POINT('Ctrl Pts',(3.75193395887977,1.,-1.80783603939617));
#52256=CARTESIAN_POINT('Ctrl Pts',(3.75681965683071,-1.,-1.8139472983358));
#52257=CARTESIAN_POINT('Ctrl Pts',(3.75681965683071,1.,-1.8139472983358));
#52258=CARTESIAN_POINT('Ctrl Pts',(3.76168412707948,-1.,-1.82008629694091));
#52259=CARTESIAN_POINT('Ctrl Pts',(3.76168412707948,1.,-1.82008629694091));
#52260=CARTESIAN_POINT('Ctrl Pts',(3.76652740353775,-1.,-1.82625289220915));
#52261=CARTESIAN_POINT('Ctrl Pts',(3.76652740353775,1.,-1.82625289220915));
#52262=CARTESIAN_POINT('Ctrl Pts',(3.77038509817999,-1.,-1.83120816955646));
#52263=CARTESIAN_POINT('Ctrl Pts',(3.77038509817999,1.,-1.83120816955646));
#52264=CARTESIAN_POINT('Ctrl Pts',(3.77326886064398,-1.,-1.83493697934534));
#52265=CARTESIAN_POINT('Ctrl Pts',(3.77326886064398,1.,-1.83493697934534));
#52266=CARTESIAN_POINT('Ctrl Pts',(3.77518714457833,-1.,-1.83742834010626));
#52267=CARTESIAN_POINT('Ctrl Pts',(3.77518714457833,1.,-1.83742834010626));
#52268=CARTESIAN_POINT('Ctrl Pts',(3.77614523045147,-1.,-1.83867539237861));
#52269=CARTESIAN_POINT('Ctrl Pts',(3.77614523045147,1.,-1.83867539237861));
#52270=CARTESIAN_POINT('',(3.42859860294306,1.,-1.5189508286633));
#52271=CARTESIAN_POINT('Ctrl Pts',(3.42859860294306,-1.,-1.5189508286633));
#52272=CARTESIAN_POINT('Ctrl Pts',(3.42859860294306,-0.666666666666667,
-1.5189508286633));
#52273=CARTESIAN_POINT('Ctrl Pts',(3.42859860294306,-0.333333333333333,
-1.5189508286633));
#52274=CARTESIAN_POINT('Ctrl Pts',(3.42859860294306,0.333333333333333,-1.5189508286633));
#52275=CARTESIAN_POINT('Ctrl Pts',(3.42859860294306,0.666666666666667,-1.5189508286633));
#52276=CARTESIAN_POINT('Ctrl Pts',(3.42859860294306,1.,-1.5189508286633));
#52277=CARTESIAN_POINT('',(3.77614523045147,1.,-1.83867539237861));
#52278=CARTESIAN_POINT('',(3.77614523045147,0.,-1.83867539237861));
#52279=CARTESIAN_POINT('Ctrl Pts',(3.42859860294306,1.,-1.5189508286633));
#52280=CARTESIAN_POINT('Ctrl Pts',(3.42864616361875,1.,-1.51893924967331));
#52281=CARTESIAN_POINT('Ctrl Pts',(3.42884302333841,1.,-1.5189513329503));
#52282=CARTESIAN_POINT('Ctrl Pts',(3.42946838852588,1.,-1.51914806898491));
#52283=CARTESIAN_POINT('Ctrl Pts',(3.43101631893414,1.,-1.5198144909338));
#52284=CARTESIAN_POINT('Ctrl Pts',(3.43417156977893,1.,-1.52134826724293));
#52285=CARTESIAN_POINT('Ctrl Pts',(3.4388889597401,1.,-1.5237734895035));
#52286=CARTESIAN_POINT('Ctrl Pts',(3.44469547526647,1.,-1.52686242875556));
#52287=CARTESIAN_POINT('Ctrl Pts',(3.45127136828305,1.,-1.53046244461635));
#52288=CARTESIAN_POINT('Ctrl Pts',(3.45825932955032,1.,-1.53440195378792));
#52289=CARTESIAN_POINT('Ctrl Pts',(3.46531752207153,1.,-1.53851507915502));
#52290=CARTESIAN_POINT('Ctrl Pts',(3.47217189224653,1.,-1.54266605398188));
#52291=CARTESIAN_POINT('Ctrl Pts',(3.47868272898751,1.,-1.54678009290276));
#52292=CARTESIAN_POINT('Ctrl Pts',(3.48485155928567,1.,-1.55084702970452));
#52293=CARTESIAN_POINT('Ctrl Pts',(3.4907646087742,1.,-1.55489595901116));
#52294=CARTESIAN_POINT('Ctrl Pts',(3.49655185179655,1.,-1.55897703097874));
#52295=CARTESIAN_POINT('Ctrl Pts',(3.50234321621578,1.,-1.56314187758675));
#52296=CARTESIAN_POINT('Ctrl Pts',(3.50821771695363,1.,-1.56742097575012));
#52297=CARTESIAN_POINT('Ctrl Pts',(3.51418598431665,1.,-1.57181569799743));
#52298=CARTESIAN_POINT('Ctrl Pts',(3.52021847865912,1.,-1.57631049988158));
#52299=CARTESIAN_POINT('Ctrl Pts',(3.52626275334881,1.,-1.58088027227848));
#52300=CARTESIAN_POINT('Ctrl Pts',(3.5322637814708,1.,-1.58549906268088));
#52301=CARTESIAN_POINT('Ctrl Pts',(3.53818616861077,1.,-1.59014958368739));
#52302=CARTESIAN_POINT('Ctrl Pts',(3.54402458182337,1.,-1.59482766949766));
#52303=CARTESIAN_POINT('Ctrl Pts',(3.54979148634454,1.,-1.59953698113457));
#52304=CARTESIAN_POINT('Ctrl Pts',(3.55550985096129,1.,-1.60428584699853));
#52305=CARTESIAN_POINT('Ctrl Pts',(3.5612043248298,1.,-1.60908344685457));
#52306=CARTESIAN_POINT('Ctrl Pts',(3.56689200468387,1.,-1.61393581747514));
#52307=CARTESIAN_POINT('Ctrl Pts',(3.57257679609806,1.,-1.61884340915404));
#52308=CARTESIAN_POINT('Ctrl Pts',(3.5782545595439,1.,-1.62380329464844));
#52309=CARTESIAN_POINT('Ctrl Pts',(3.58391625774343,1.,-1.62881051550745));
#52310=CARTESIAN_POINT('Ctrl Pts',(3.58955176627879,1.,-1.6338597145126));
#52311=CARTESIAN_POINT('Ctrl Pts',(3.59515368334893,1.,-1.63894676675352));
#52312=CARTESIAN_POINT('Ctrl Pts',(3.60072028513845,1.,-1.64407004385582));
#52313=CARTESIAN_POINT('Ctrl Pts',(3.60625346556992,1.,-1.64922952425832));
#52314=CARTESIAN_POINT('Ctrl Pts',(3.61175734965127,1.,-1.65442619244325));
#52315=CARTESIAN_POINT('Ctrl Pts',(3.61723666482456,1.,-1.65966133399186));
#52316=CARTESIAN_POINT('Ctrl Pts',(3.62269517989109,1.,-1.66493585923855));
#52317=CARTESIAN_POINT('Ctrl Pts',(3.62813422105271,1.,-1.67024966008045));
#52318=CARTESIAN_POINT('Ctrl Pts',(3.63355343201232,1.,-1.67560193613156));
#52319=CARTESIAN_POINT('Ctrl Pts',(3.63895140887462,1.,-1.68099146651586));
#52320=CARTESIAN_POINT('Ctrl Pts',(3.64432638915203,1.,-1.68641690471457));
#52321=CARTESIAN_POINT('Ctrl Pts',(3.64967689827371,1.,-1.69187705481689));
#52322=CARTESIAN_POINT('Ctrl Pts',(3.65500246526749,1.,-1.69737117722534));
#52323=CARTESIAN_POINT('Ctrl Pts',(3.66030338774847,1.,-1.70289888566873));
#52324=CARTESIAN_POINT('Ctrl Pts',(3.66558043198876,1.,-1.70846001610956));
#52325=CARTESIAN_POINT('Ctrl Pts',(3.67083454901611,1.,-1.71405450210384));
#52326=CARTESIAN_POINT('Ctrl Pts',(3.67606660374709,1.,-1.71968225581808));
#52327=CARTESIAN_POINT('Ctrl Pts',(3.68127704936579,1.,-1.72534302437056));
#52328=CARTESIAN_POINT('Ctrl Pts',(3.68646597019332,1.,-1.73103640956717));
#52329=CARTESIAN_POINT('Ctrl Pts',(3.69163322648036,1.,-1.73676193254557));
#52330=CARTESIAN_POINT('Ctrl Pts',(3.69677856910517,1.,-1.74251908492617));
#52331=CARTESIAN_POINT('Ctrl Pts',(3.7019017567335,1.,-1.74830738046057));
#52332=CARTESIAN_POINT('Ctrl Pts',(3.70700269736659,1.,-1.75412641804042));
#52333=CARTESIAN_POINT('Ctrl Pts',(3.71208146346136,1.,-1.75997588498865));
#52334=CARTESIAN_POINT('Ctrl Pts',(3.71713822377359,1.,-1.76585552124394));
#52335=CARTESIAN_POINT('Ctrl Pts',(3.72217319911254,1.,-1.77176509401761));
#52336=CARTESIAN_POINT('Ctrl Pts',(3.72718661205609,1.,-1.77770437039658));
#52337=CARTESIAN_POINT('Ctrl Pts',(3.7321786309547,1.,-1.78367308442901));
#52338=CARTESIAN_POINT('Ctrl Pts',(3.73714934730681,1.,-1.78967092823491));
#52339=CARTESIAN_POINT('Ctrl Pts',(3.74209880352445,1.,-1.79569757859422));
#52340=CARTESIAN_POINT('Ctrl Pts',(3.74702700875467,1.,-1.8017527148577));
#52341=CARTESIAN_POINT('Ctrl Pts',(3.75193395887977,1.,-1.80783603939617));
#52342=CARTESIAN_POINT('Ctrl Pts',(3.75681965683071,1.,-1.8139472983358));
#52343=CARTESIAN_POINT('Ctrl Pts',(3.76168412707948,1.,-1.82008629694091));
#52344=CARTESIAN_POINT('Ctrl Pts',(3.76652740353775,1.,-1.82625289220915));
#52345=CARTESIAN_POINT('Ctrl Pts',(3.77038509817999,1.,-1.83120816955646));
#52346=CARTESIAN_POINT('Ctrl Pts',(3.77326886064398,1.,-1.83493697934534));
#52347=CARTESIAN_POINT('Ctrl Pts',(3.77518714457833,1.,-1.83742834010626));
#52348=CARTESIAN_POINT('Ctrl Pts',(3.77614523045147,1.,-1.83867539237861));
#52349=CARTESIAN_POINT('Origin',(3.77614523045147,0.,-1.83867539237861));
#52350=CARTESIAN_POINT('',(3.70708211654725,1.,-1.97421938526992));
#52351=CARTESIAN_POINT('Origin',(0.,0.,0.));
#52352=CARTESIAN_POINT('',(3.49844575334386,1.,-1.35032489087269));
#52353=CARTESIAN_POINT('Origin',(0.,1.,0.));
#52354=CARTESIAN_POINT('Ctrl Pts',(3.49844575334386,1.,-1.35032489087269));
#52355=CARTESIAN_POINT('Ctrl Pts',(3.49844575334386,0.666666666666667,-1.35032489087269));
#52356=CARTESIAN_POINT('Ctrl Pts',(3.49844575334386,0.333333333333333,-1.35032489087269));
#52357=CARTESIAN_POINT('Ctrl Pts',(3.49844575334386,-0.333333333333333,
-1.35032489087269));
#52358=CARTESIAN_POINT('Ctrl Pts',(3.49844575334386,-0.666666666666667,
-1.35032489087269));
#52359=CARTESIAN_POINT('Ctrl Pts',(3.49844575334386,-1.,-1.35032489087269));
#52360=CARTESIAN_POINT('Ctrl Pts',(3.97027773754922,-1.,-1.36999806084572));
#52361=CARTESIAN_POINT('Ctrl Pts',(3.97027773754922,1.,-1.36999806084572));
#52362=CARTESIAN_POINT('Ctrl Pts',(3.9687184694173,-1.,-1.37020239094758));
#52363=CARTESIAN_POINT('Ctrl Pts',(3.9687184694173,1.,-1.37020239094758));
#52364=CARTESIAN_POINT('Ctrl Pts',(3.96560037975788,-1.,-1.37060761746027));
#52365=CARTESIAN_POINT('Ctrl Pts',(3.96560037975788,1.,-1.37060761746027));
#52366=CARTESIAN_POINT('Ctrl Pts',(3.96092458508407,-1.,-1.37120515615663));
#52367=CARTESIAN_POINT('Ctrl Pts',(3.96092458508407,1.,-1.37120515615663));
#52368=CARTESIAN_POINT('Ctrl Pts',(3.95469287283105,-1.,-1.37198126433139));
#52369=CARTESIAN_POINT('Ctrl Pts',(3.95469287283105,1.,-1.37198126433139));
#52370=CARTESIAN_POINT('Ctrl Pts',(3.94690771786926,-1.,-1.37291699203423));
#52371=CARTESIAN_POINT('Ctrl Pts',(3.94690771786926,1.,-1.37291699203423));
#52372=CARTESIAN_POINT('Ctrl Pts',(3.93912709041791,-1.,-1.37381821967499));
#52373=CARTESIAN_POINT('Ctrl Pts',(3.93912709041791,1.,-1.37381821967499));
#52374=CARTESIAN_POINT('Ctrl Pts',(3.93135106761941,-1.,-1.37468482215784));
#52375=CARTESIAN_POINT('Ctrl Pts',(3.93135106761941,1.,-1.37468482215784));
#52376=CARTESIAN_POINT('Ctrl Pts',(3.92357976987132,-1.,-1.37551664448057));
#52377=CARTESIAN_POINT('Ctrl Pts',(3.92357976987132,1.,-1.37551664448057));
#52378=CARTESIAN_POINT('Ctrl Pts',(3.91581337461825,-1.,-1.37631350505516));
#52379=CARTESIAN_POINT('Ctrl Pts',(3.91581337461825,1.,-1.37631350505516));
#52380=CARTESIAN_POINT('Ctrl Pts',(3.90805209522729,-1.,-1.3770751963376));
#52381=CARTESIAN_POINT('Ctrl Pts',(3.90805209522729,1.,-1.3770751963376));
#52382=CARTESIAN_POINT('Ctrl Pts',(3.90029615196255,-1.,-1.3778014851263));
#52383=CARTESIAN_POINT('Ctrl Pts',(3.90029615196255,1.,-1.3778014851263));
#52384=CARTESIAN_POINT('Ctrl Pts',(3.89254574338385,-1.,-1.37849211287981));
#52385=CARTESIAN_POINT('Ctrl Pts',(3.89254574338385,1.,-1.37849211287981));
#52386=CARTESIAN_POINT('Ctrl Pts',(3.88480102249461,-1.,-1.37914679719446));
#52387=CARTESIAN_POINT('Ctrl Pts',(3.88480102249461,1.,-1.37914679719446));
#52388=CARTESIAN_POINT('Ctrl Pts',(3.87706205830865,-1.,-1.37976523097187));
#52389=CARTESIAN_POINT('Ctrl Pts',(3.87706205830865,1.,-1.37976523097187));
#52390=CARTESIAN_POINT('Ctrl Pts',(3.86932885813403,-1.,-1.38034709213129));
#52391=CARTESIAN_POINT('Ctrl Pts',(3.86932885813403,1.,-1.38034709213129));
#52392=CARTESIAN_POINT('Ctrl Pts',(3.86160143044187,-1.,-1.38089205993068));
#52393=CARTESIAN_POINT('Ctrl Pts',(3.86160143044187,1.,-1.38089205993068));
#52394=CARTESIAN_POINT('Ctrl Pts',(3.85387983979557,-1.,-1.38139983115075));
#52395=CARTESIAN_POINT('Ctrl Pts',(3.85387983979557,1.,-1.38139983115075));
#52396=CARTESIAN_POINT('Ctrl Pts',(3.84616425605705,-1.,-1.38187013346089));
#52397=CARTESIAN_POINT('Ctrl Pts',(3.84616425605705,1.,-1.38187013346089));
#52398=CARTESIAN_POINT('Ctrl Pts',(3.83845502790609,-1.,-1.38230274828774));
#52399=CARTESIAN_POINT('Ctrl Pts',(3.83845502790609,1.,-1.38230274828774));
#52400=CARTESIAN_POINT('Ctrl Pts',(3.83075266982138,-1.,-1.38269750245086));
#52401=CARTESIAN_POINT('Ctrl Pts',(3.83075266982138,1.,-1.38269750245086));
#52402=CARTESIAN_POINT('Ctrl Pts',(3.82305771743715,-1.,-1.38305421262724));
#52403=CARTESIAN_POINT('Ctrl Pts',(3.82305771743715,1.,-1.38305421262724));
#52404=CARTESIAN_POINT('Ctrl Pts',(3.81537060817765,-1.,-1.38337263902766));
#52405=CARTESIAN_POINT('Ctrl Pts',(3.81537060817765,1.,-1.38337263902766));
#52406=CARTESIAN_POINT('Ctrl Pts',(3.80769156398429,-1.,-1.38365244046226));
#52407=CARTESIAN_POINT('Ctrl Pts',(3.80769156398429,1.,-1.38365244046226));
#52408=CARTESIAN_POINT('Ctrl Pts',(3.80002044322169,-1.,-1.38389311766701));
#52409=CARTESIAN_POINT('Ctrl Pts',(3.80002044322169,1.,-1.38389311766701));
#52410=CARTESIAN_POINT('Ctrl Pts',(3.79235669640907,-1.,-1.38409399694589));
#52411=CARTESIAN_POINT('Ctrl Pts',(3.79235669640907,1.,-1.38409399694589));
#52412=CARTESIAN_POINT('Ctrl Pts',(3.78469969805134,-1.,-1.38425435883773));
#52413=CARTESIAN_POINT('Ctrl Pts',(3.78469969805134,1.,-1.38425435883773));
#52414=CARTESIAN_POINT('Ctrl Pts',(3.77704902230441,-1.,-1.38437354551435));
#52415=CARTESIAN_POINT('Ctrl Pts',(3.77704902230441,1.,-1.38437354551435));
#52416=CARTESIAN_POINT('Ctrl Pts',(3.76940473185775,-1.,-1.38445107339517));
#52417=CARTESIAN_POINT('Ctrl Pts',(3.76940473185775,1.,-1.38445107339517));
#52418=CARTESIAN_POINT('Ctrl Pts',(3.76176768271347,-1.,-1.38448675253343));
#52419=CARTESIAN_POINT('Ctrl Pts',(3.76176768271347,1.,-1.38448675253343));
#52420=CARTESIAN_POINT('Ctrl Pts',(3.75413976318727,-1.,-1.38448077997155));
#52421=CARTESIAN_POINT('Ctrl Pts',(3.75413976318727,1.,-1.38448077997155));
#52422=CARTESIAN_POINT('Ctrl Pts',(3.7465231716786,-1.,-1.38443344984389));
#52423=CARTESIAN_POINT('Ctrl Pts',(3.7465231716786,1.,-1.38443344984389));
#52424=CARTESIAN_POINT('Ctrl Pts',(3.73891976418099,-1.,-1.38434489156456));
#52425=CARTESIAN_POINT('Ctrl Pts',(3.73891976418099,1.,-1.38434489156456));
#52426=CARTESIAN_POINT('Ctrl Pts',(3.73133035859283,-1.,-1.38421479111531));
#52427=CARTESIAN_POINT('Ctrl Pts',(3.73133035859283,1.,-1.38421479111531));
#52428=CARTESIAN_POINT('Ctrl Pts',(3.72375409358805,-1.,-1.3840421342895));
#52429=CARTESIAN_POINT('Ctrl Pts',(3.72375409358805,1.,-1.3840421342895));
#52430=CARTESIAN_POINT('Ctrl Pts',(3.7161876605181,-1.,-1.38382489984585));
#52431=CARTESIAN_POINT('Ctrl Pts',(3.7161876605181,1.,-1.38382489984585));
#52432=CARTESIAN_POINT('Ctrl Pts',(3.70862680753343,-1.,-1.38356065402122));
#52433=CARTESIAN_POINT('Ctrl Pts',(3.70862680753343,1.,-1.38356065402122));
#52434=CARTESIAN_POINT('Ctrl Pts',(3.70106792167894,-1.,-1.38324717612862));
#52435=CARTESIAN_POINT('Ctrl Pts',(3.70106792167894,1.,-1.38324717612862));
#52436=CARTESIAN_POINT('Ctrl Pts',(3.69350967899523,-1.,-1.38288311171649));
#52437=CARTESIAN_POINT('Ctrl Pts',(3.69350967899523,1.,-1.38288311171649));
#52438=CARTESIAN_POINT('Ctrl Pts',(3.68595444983844,-1.,-1.38246852827185));
#52439=CARTESIAN_POINT('Ctrl Pts',(3.68595444983844,1.,-1.38246852827185));
#52440=CARTESIAN_POINT('Ctrl Pts',(3.6784103848243,-1.,-1.38200574290626));
#52441=CARTESIAN_POINT('Ctrl Pts',(3.6784103848243,1.,-1.38200574290626));
#52442=CARTESIAN_POINT('Ctrl Pts',(3.67088843112282,-1.,-1.38149812653876));
#52443=CARTESIAN_POINT('Ctrl Pts',(3.67088843112282,1.,-1.38149812653876));
#52444=CARTESIAN_POINT('Ctrl Pts',(3.66339848520874,-1.,-1.38094856333558));
#52445=CARTESIAN_POINT('Ctrl Pts',(3.66339848520874,1.,-1.38094856333558));
#52446=CARTESIAN_POINT('Ctrl Pts',(3.65594554404396,-1.,-1.38035791051215));
#52447=CARTESIAN_POINT('Ctrl Pts',(3.65594554404396,1.,-1.38035791051215));
#52448=CARTESIAN_POINT('Ctrl Pts',(3.64852652756444,-1.,-1.37972372481598));
#52449=CARTESIAN_POINT('Ctrl Pts',(3.64852652756444,1.,-1.37972372481598));
#52450=CARTESIAN_POINT('Ctrl Pts',(3.64112507791112,-1.,-1.37903818567347));
#52451=CARTESIAN_POINT('Ctrl Pts',(3.64112507791112,1.,-1.37903818567347));
#52452=CARTESIAN_POINT('Ctrl Pts',(3.63371727442448,-1.,-1.37829035457325));
#52453=CARTESIAN_POINT('Ctrl Pts',(3.63371727442448,1.,-1.37829035457325));
#52454=CARTESIAN_POINT('Ctrl Pts',(3.62628098665112,-1.,-1.37746987919868));
#52455=CARTESIAN_POINT('Ctrl Pts',(3.62628098665112,1.,-1.37746987919868));
#52456=CARTESIAN_POINT('Ctrl Pts',(3.61880481160408,-1.,-1.37657053403102));
#52457=CARTESIAN_POINT('Ctrl Pts',(3.61880481160408,1.,-1.37657053403102));
#52458=CARTESIAN_POINT('Ctrl Pts',(3.61129546591082,-1.,-1.37559314436641));
#52459=CARTESIAN_POINT('Ctrl Pts',(3.61129546591082,1.,-1.37559314436641));
#52460=CARTESIAN_POINT('Ctrl Pts',(3.60379020124038,-1.,-1.37455051379642));
#52461=CARTESIAN_POINT('Ctrl Pts',(3.60379020124038,1.,-1.37455051379642));
#52462=CARTESIAN_POINT('Ctrl Pts',(3.59634627869117,-1.,-1.37346320103184));
#52463=CARTESIAN_POINT('Ctrl Pts',(3.59634627869117,1.,-1.37346320103184));
#52464=CARTESIAN_POINT('Ctrl Pts',(3.5890185384643,-1.,-1.37235053661));
#52465=CARTESIAN_POINT('Ctrl Pts',(3.5890185384643,1.,-1.37235053661));
#52466=CARTESIAN_POINT('Ctrl Pts',(3.58183885982745,-1.,-1.37122241663073));
#52467=CARTESIAN_POINT('Ctrl Pts',(3.58183885982745,1.,-1.37122241663073));
#52468=CARTESIAN_POINT('Ctrl Pts',(3.57479875549453,-1.,-1.37007229485646));
#52469=CARTESIAN_POINT('Ctrl Pts',(3.57479875549453,1.,-1.37007229485646));
#52470=CARTESIAN_POINT('Ctrl Pts',(3.56782080304554,-1.,-1.36886584973349));
#52471=CARTESIAN_POINT('Ctrl Pts',(3.56782080304554,1.,-1.36886584973349));
#52472=CARTESIAN_POINT('Ctrl Pts',(3.56077662028492,-1.,-1.36754771771174));
#52473=CARTESIAN_POINT('Ctrl Pts',(3.56077662028492,1.,-1.36754771771174));
#52474=CARTESIAN_POINT('Ctrl Pts',(3.55353883995793,-1.,-1.36606145456711));
#52475=CARTESIAN_POINT('Ctrl Pts',(3.55353883995793,1.,-1.36606145456711));
#52476=CARTESIAN_POINT('Ctrl Pts',(3.54602591832893,-1.,-1.36436666257568));
#52477=CARTESIAN_POINT('Ctrl Pts',(3.54602591832893,1.,-1.36436666257568));
#52478=CARTESIAN_POINT('Ctrl Pts',(3.53824396425032,-1.,-1.36245507339334));
#52479=CARTESIAN_POINT('Ctrl Pts',(3.53824396425032,1.,-1.36245507339334));
#52480=CARTESIAN_POINT('Ctrl Pts',(3.53034464961849,-1.,-1.36037259643827));
#52481=CARTESIAN_POINT('Ctrl Pts',(3.53034464961849,1.,-1.36037259643827));
#52482=CARTESIAN_POINT('Ctrl Pts',(3.52261776117121,-1.,-1.35821701528975));
#52483=CARTESIAN_POINT('Ctrl Pts',(3.52261776117121,1.,-1.35821701528975));
#52484=CARTESIAN_POINT('Ctrl Pts',(3.51542230699919,-1.,-1.35611275237288));
#52485=CARTESIAN_POINT('Ctrl Pts',(3.51542230699919,1.,-1.35611275237288));
#52486=CARTESIAN_POINT('Ctrl Pts',(3.50913227060177,-1.,-1.35419113576022));
#52487=CARTESIAN_POINT('Ctrl Pts',(3.50913227060177,1.,-1.35419113576022));
#52488=CARTESIAN_POINT('Ctrl Pts',(3.50408168106113,-1.,-1.3525703284343));
#52489=CARTESIAN_POINT('Ctrl Pts',(3.50408168106113,1.,-1.3525703284343));
#52490=CARTESIAN_POINT('Ctrl Pts',(3.50049707063673,-1.,-1.35133076331065));
#52491=CARTESIAN_POINT('Ctrl Pts',(3.50049707063673,1.,-1.35133076331065));
#52492=CARTESIAN_POINT('Ctrl Pts',(3.49888720256612,-1.,-1.35067437417289));
#52493=CARTESIAN_POINT('Ctrl Pts',(3.49888720256612,1.,-1.35067437417289));
#52494=CARTESIAN_POINT('Ctrl Pts',(3.49840357193384,-1.,-1.35037650302887));
#52495=CARTESIAN_POINT('Ctrl Pts',(3.49840357193384,1.,-1.35037650302887));
#52496=CARTESIAN_POINT('Ctrl Pts',(3.49840260053616,-1.,-1.35026426118352));
#52497=CARTESIAN_POINT('Ctrl Pts',(3.49840260053616,1.,-1.35026426118352));
#52498=CARTESIAN_POINT('Ctrl Pts',(3.49848248301936,-1.,-1.35022972712301));
#52499=CARTESIAN_POINT('Ctrl Pts',(3.49848248301936,1.,-1.35022972712301));
#52500=CARTESIAN_POINT('',(3.97027773754922,1.,-1.36999806084572));
#52501=CARTESIAN_POINT('Ctrl Pts',(3.97027773754922,1.,-1.36999806084572));
#52502=CARTESIAN_POINT('Ctrl Pts',(3.9687184694173,1.,-1.37020239094758));
#52503=CARTESIAN_POINT('Ctrl Pts',(3.96560037975788,1.,-1.37060761746027));
#52504=CARTESIAN_POINT('Ctrl Pts',(3.96092458508407,1.,-1.37120515615663));
#52505=CARTESIAN_POINT('Ctrl Pts',(3.95469287283105,1.,-1.37198126433139));
#52506=CARTESIAN_POINT('Ctrl Pts',(3.94690771786926,1.,-1.37291699203423));
#52507=CARTESIAN_POINT('Ctrl Pts',(3.93912709041791,1.,-1.37381821967499));
#52508=CARTESIAN_POINT('Ctrl Pts',(3.93135106761941,1.,-1.37468482215784));
#52509=CARTESIAN_POINT('Ctrl Pts',(3.92357976987132,1.,-1.37551664448057));
#52510=CARTESIAN_POINT('Ctrl Pts',(3.91581337461825,1.,-1.37631350505516));
#52511=CARTESIAN_POINT('Ctrl Pts',(3.90805209522729,1.,-1.3770751963376));
#52512=CARTESIAN_POINT('Ctrl Pts',(3.90029615196255,1.,-1.3778014851263));
#52513=CARTESIAN_POINT('Ctrl Pts',(3.89254574338385,1.,-1.37849211287981));
#52514=CARTESIAN_POINT('Ctrl Pts',(3.88480102249461,1.,-1.37914679719446));
#52515=CARTESIAN_POINT('Ctrl Pts',(3.87706205830865,1.,-1.37976523097187));
#52516=CARTESIAN_POINT('Ctrl Pts',(3.86932885813403,1.,-1.38034709213129));
#52517=CARTESIAN_POINT('Ctrl Pts',(3.86160143044187,1.,-1.38089205993068));
#52518=CARTESIAN_POINT('Ctrl Pts',(3.85387983979557,1.,-1.38139983115075));
#52519=CARTESIAN_POINT('Ctrl Pts',(3.84616425605705,1.,-1.38187013346089));
#52520=CARTESIAN_POINT('Ctrl Pts',(3.83845502790609,1.,-1.38230274828774));
#52521=CARTESIAN_POINT('Ctrl Pts',(3.83075266982138,1.,-1.38269750245086));
#52522=CARTESIAN_POINT('Ctrl Pts',(3.82305771743715,1.,-1.38305421262724));
#52523=CARTESIAN_POINT('Ctrl Pts',(3.81537060817765,1.,-1.38337263902766));
#52524=CARTESIAN_POINT('Ctrl Pts',(3.80769156398429,1.,-1.38365244046226));
#52525=CARTESIAN_POINT('Ctrl Pts',(3.80002044322169,1.,-1.38389311766701));
#52526=CARTESIAN_POINT('Ctrl Pts',(3.79235669640907,1.,-1.38409399694589));
#52527=CARTESIAN_POINT('Ctrl Pts',(3.78469969805134,1.,-1.38425435883773));
#52528=CARTESIAN_POINT('Ctrl Pts',(3.77704902230441,1.,-1.38437354551435));
#52529=CARTESIAN_POINT('Ctrl Pts',(3.76940473185775,1.,-1.38445107339517));
#52530=CARTESIAN_POINT('Ctrl Pts',(3.76176768271347,1.,-1.38448675253343));
#52531=CARTESIAN_POINT('Ctrl Pts',(3.75413976318727,1.,-1.38448077997155));
#52532=CARTESIAN_POINT('Ctrl Pts',(3.7465231716786,1.,-1.38443344984389));
#52533=CARTESIAN_POINT('Ctrl Pts',(3.73891976418099,1.,-1.38434489156456));
#52534=CARTESIAN_POINT('Ctrl Pts',(3.73133035859283,1.,-1.38421479111531));
#52535=CARTESIAN_POINT('Ctrl Pts',(3.72375409358805,1.,-1.3840421342895));
#52536=CARTESIAN_POINT('Ctrl Pts',(3.7161876605181,1.,-1.38382489984585));
#52537=CARTESIAN_POINT('Ctrl Pts',(3.70862680753343,1.,-1.38356065402122));
#52538=CARTESIAN_POINT('Ctrl Pts',(3.70106792167894,1.,-1.38324717612862));
#52539=CARTESIAN_POINT('Ctrl Pts',(3.69350967899523,1.,-1.38288311171649));
#52540=CARTESIAN_POINT('Ctrl Pts',(3.68595444983844,1.,-1.38246852827185));
#52541=CARTESIAN_POINT('Ctrl Pts',(3.6784103848243,1.,-1.38200574290626));
#52542=CARTESIAN_POINT('Ctrl Pts',(3.67088843112282,1.,-1.38149812653876));
#52543=CARTESIAN_POINT('Ctrl Pts',(3.66339848520874,1.,-1.38094856333558));
#52544=CARTESIAN_POINT('Ctrl Pts',(3.65594554404396,1.,-1.38035791051215));
#52545=CARTESIAN_POINT('Ctrl Pts',(3.64852652756444,1.,-1.37972372481598));
#52546=CARTESIAN_POINT('Ctrl Pts',(3.64112507791112,1.,-1.37903818567347));
#52547=CARTESIAN_POINT('Ctrl Pts',(3.63371727442448,1.,-1.37829035457325));
#52548=CARTESIAN_POINT('Ctrl Pts',(3.62628098665112,1.,-1.37746987919868));
#52549=CARTESIAN_POINT('Ctrl Pts',(3.61880481160408,1.,-1.37657053403102));
#52550=CARTESIAN_POINT('Ctrl Pts',(3.61129546591082,1.,-1.37559314436641));
#52551=CARTESIAN_POINT('Ctrl Pts',(3.60379020124038,1.,-1.37455051379642));
#52552=CARTESIAN_POINT('Ctrl Pts',(3.59634627869117,1.,-1.37346320103184));
#52553=CARTESIAN_POINT('Ctrl Pts',(3.5890185384643,1.,-1.37235053661));
#52554=CARTESIAN_POINT('Ctrl Pts',(3.58183885982745,1.,-1.37122241663073));
#52555=CARTESIAN_POINT('Ctrl Pts',(3.57479875549453,1.,-1.37007229485646));
#52556=CARTESIAN_POINT('Ctrl Pts',(3.56782080304554,1.,-1.36886584973349));
#52557=CARTESIAN_POINT('Ctrl Pts',(3.56077662028492,1.,-1.36754771771174));
#52558=CARTESIAN_POINT('Ctrl Pts',(3.55353883995793,1.,-1.36606145456711));
#52559=CARTESIAN_POINT('Ctrl Pts',(3.54602591832893,1.,-1.36436666257568));
#52560=CARTESIAN_POINT('Ctrl Pts',(3.53824396425032,1.,-1.36245507339334));
#52561=CARTESIAN_POINT('Ctrl Pts',(3.53034464961849,1.,-1.36037259643827));
#52562=CARTESIAN_POINT('Ctrl Pts',(3.52261776117121,1.,-1.35821701528975));
#52563=CARTESIAN_POINT('Ctrl Pts',(3.51542230699919,1.,-1.35611275237288));
#52564=CARTESIAN_POINT('Ctrl Pts',(3.50913227060177,1.,-1.35419113576022));
#52565=CARTESIAN_POINT('Ctrl Pts',(3.50408168106113,1.,-1.3525703284343));
#52566=CARTESIAN_POINT('Ctrl Pts',(3.5007660381658,1.,-1.35142377279535));
#52567=CARTESIAN_POINT('Ctrl Pts',(3.49920025459856,1.,-1.35080045218652));
#52568=CARTESIAN_POINT('Ctrl Pts',(3.49861894124915,1.,-1.35049736560633));
#52569=CARTESIAN_POINT('Ctrl Pts',(3.49847119623841,1.,-1.35036670893102));
#52570=CARTESIAN_POINT('Ctrl Pts',(3.49844575334386,1.,-1.35032489087269));
#52571=CARTESIAN_POINT('',(3.97027773754922,0.,-1.36999806084572));
#52572=CARTESIAN_POINT('Ctrl Pts',(3.62397690409552,-1.,-0.963997613369571));
#52573=CARTESIAN_POINT('Ctrl Pts',(3.62397690409552,1.,-0.963997613369571));
#52574=CARTESIAN_POINT('Ctrl Pts',(3.62393257642191,-1.,-0.963922720982576));
#52575=CARTESIAN_POINT('Ctrl Pts',(3.62393257642191,1.,-0.963922720982576));
#52576=CARTESIAN_POINT('Ctrl Pts',(3.62399933640277,-1.,-0.963832486396056));
#52577=CARTESIAN_POINT('Ctrl Pts',(3.62399933640277,1.,-0.963832486396056));
#52578=CARTESIAN_POINT('Ctrl Pts',(3.62456568607055,-1.,-0.963875774532103));
#52579=CARTESIAN_POINT('Ctrl Pts',(3.62456568607055,1.,-0.963875774532103));
#52580=CARTESIAN_POINT('Ctrl Pts',(3.62625391255277,-1.,-0.964291001274619));
#52581=CARTESIAN_POINT('Ctrl Pts',(3.62625391255277,1.,-0.964291001274619));
#52582=CARTESIAN_POINT('Ctrl Pts',(3.62988252139998,-1.,-0.965395153165716));
#52583=CARTESIAN_POINT('Ctrl Pts',(3.62988252139998,1.,-0.965395153165716));
#52584=CARTESIAN_POINT('Ctrl Pts',(3.6349212208096,-1.,-0.967052554540878));
#52585=CARTESIAN_POINT('Ctrl Pts',(3.6349212208096,1.,-0.967052554540878));
#52586=CARTESIAN_POINT('Ctrl Pts',(3.64113946505393,-1.,-0.969195124674829));
#52587=CARTESIAN_POINT('Ctrl Pts',(3.64113946505393,1.,-0.969195124674829));
#52588=CARTESIAN_POINT('Ctrl Pts',(3.64819756447072,-1.,-0.971722122060278));
#52589=CARTESIAN_POINT('Ctrl Pts',(3.64819756447072,1.,-0.971722122060278));
#52590=CARTESIAN_POINT('Ctrl Pts',(3.6557157673487,-1.,-0.974519971354139));
#52591=CARTESIAN_POINT('Ctrl Pts',(3.6557157673487,1.,-0.974519971354139));
#52592=CARTESIAN_POINT('Ctrl Pts',(3.66333049637403,-1.,-0.977478312751416));
#52593=CARTESIAN_POINT('Ctrl Pts',(3.66333049637403,1.,-0.977478312751416));
#52594=CARTESIAN_POINT('Ctrl Pts',(3.67074983340444,-1.,-0.980505922458495));
#52595=CARTESIAN_POINT('Ctrl Pts',(3.67074983340444,1.,-0.980505922458495));
#52596=CARTESIAN_POINT('Ctrl Pts',(3.67782408841876,-1.,-0.983550791470865));
#52597=CARTESIAN_POINT('Ctrl Pts',(3.67782408841876,1.,-0.983550791470865));
#52598=CARTESIAN_POINT('Ctrl Pts',(3.6845531792623,-1.,-0.986602639864286));
#52599=CARTESIAN_POINT('Ctrl Pts',(3.6845531792623,1.,-0.986602639864286));
#52600=CARTESIAN_POINT('Ctrl Pts',(3.69102682138955,-1.,-0.989676715398859));
#52601=CARTESIAN_POINT('Ctrl Pts',(3.69102682138955,1.,-0.989676715398859));
#52602=CARTESIAN_POINT('Ctrl Pts',(3.69738123415696,-1.,-0.992802218332104));
#52603=CARTESIAN_POINT('Ctrl Pts',(3.69738123415696,1.,-0.992802218332104));
#52604=CARTESIAN_POINT('Ctrl Pts',(3.70375282282107,-1.,-0.996009819772432));
#52605=CARTESIAN_POINT('Ctrl Pts',(3.70375282282107,1.,-0.996009819772432));
#52606=CARTESIAN_POINT('Ctrl Pts',(3.7102243971387,-1.,-0.999317260756345));
#52607=CARTESIAN_POINT('Ctrl Pts',(3.7102243971387,1.,-0.999317260756345));
#52608=CARTESIAN_POINT('Ctrl Pts',(3.71680667125047,-1.,-1.00272423396802));
#52609=CARTESIAN_POINT('Ctrl Pts',(3.71680667125047,1.,-1.00272423396802));
#52610=CARTESIAN_POINT('Ctrl Pts',(3.72346803750544,-1.,-1.00622000735696));
#52611=CARTESIAN_POINT('Ctrl Pts',(3.72346803750544,1.,-1.00622000735696));
#52612=CARTESIAN_POINT('Ctrl Pts',(3.73015276704407,-1.,-1.00978798539491));
#52613=CARTESIAN_POINT('Ctrl Pts',(3.73015276704407,1.,-1.00978798539491));
#52614=CARTESIAN_POINT('Ctrl Pts',(3.73680245055747,-1.,-1.01341114319906));
#52615=CARTESIAN_POINT('Ctrl Pts',(3.73680245055747,1.,-1.01341114319906));
#52616=CARTESIAN_POINT('Ctrl Pts',(3.74337942504993,-1.,-1.01707794311088));
#52617=CARTESIAN_POINT('Ctrl Pts',(3.74337942504993,1.,-1.01707794311088));
#52618=CARTESIAN_POINT('Ctrl Pts',(3.74987777155873,-1.,-1.02078510487439));
#52619=CARTESIAN_POINT('Ctrl Pts',(3.74987777155873,1.,-1.02078510487439));
#52620=CARTESIAN_POINT('Ctrl Pts',(3.75631037456224,-1.,-1.02453429444668));
#52621=CARTESIAN_POINT('Ctrl Pts',(3.75631037456224,1.,-1.02453429444668));
#52622=CARTESIAN_POINT('Ctrl Pts',(3.76270122291245,-1.,-1.02833014458184));
#52623=CARTESIAN_POINT('Ctrl Pts',(3.76270122291245,1.,-1.02833014458184));
#52624=CARTESIAN_POINT('Ctrl Pts',(3.76907609832516,-1.,-1.03217786604919));
#52625=CARTESIAN_POINT('Ctrl Pts',(3.76907609832516,1.,-1.03217786604919));
#52626=CARTESIAN_POINT('Ctrl Pts',(3.77545283140427,-1.,-1.03608074678008));
#52627=CARTESIAN_POINT('Ctrl Pts',(3.77545283140427,1.,-1.03608074678008));
#52628=CARTESIAN_POINT('Ctrl Pts',(3.7818353500817,-1.,-1.04003862055798));
#52629=CARTESIAN_POINT('Ctrl Pts',(3.7818353500817,1.,-1.04003862055798));
#52630=CARTESIAN_POINT('Ctrl Pts',(3.78821910787179,-1.,-1.04404924374422));
#52631=CARTESIAN_POINT('Ctrl Pts',(3.78821910787179,1.,-1.04404924374422));
#52632=CARTESIAN_POINT('Ctrl Pts',(3.79459440308786,-1.,-1.04810913267639));
#52633=CARTESIAN_POINT('Ctrl Pts',(3.79459440308786,1.,-1.04810913267639));
#52634=CARTESIAN_POINT('Ctrl Pts',(3.80095039790681,-1.,-1.05221457990016));
#52635=CARTESIAN_POINT('Ctrl Pts',(3.80095039790681,1.,-1.05221457990016));
#52636=CARTESIAN_POINT('Ctrl Pts',(3.80727913637791,-1.,-1.05636266918644));
#52637=CARTESIAN_POINT('Ctrl Pts',(3.80727913637791,1.,-1.05636266918644));
#52638=CARTESIAN_POINT('Ctrl Pts',(3.8135786611749,-1.,-1.06055206187299));
#52639=CARTESIAN_POINT('Ctrl Pts',(3.8135786611749,1.,-1.06055206187299));
#52640=CARTESIAN_POINT('Ctrl Pts',(3.81985083953012,-1.,-1.0647824403893));
#52641=CARTESIAN_POINT('Ctrl Pts',(3.81985083953012,1.,-1.0647824403893));
#52642=CARTESIAN_POINT('Ctrl Pts',(3.82609989967276,-1.,-1.06905413180359));
#52643=CARTESIAN_POINT('Ctrl Pts',(3.82609989967276,1.,-1.06905413180359));
#52644=CARTESIAN_POINT('Ctrl Pts',(3.83233071195144,-1.,-1.07336766633459));
#52645=CARTESIAN_POINT('Ctrl Pts',(3.83233071195144,1.,-1.07336766633459));
#52646=CARTESIAN_POINT('Ctrl Pts',(3.83854714117491,-1.,-1.07772335353858));
#52647=CARTESIAN_POINT('Ctrl Pts',(3.83854714117491,1.,-1.07772335353858));
#52648=CARTESIAN_POINT('Ctrl Pts',(3.8447504803063,-1.,-1.08212087917991));
#52649=CARTESIAN_POINT('Ctrl Pts',(3.8447504803063,1.,-1.08212087917991));
#52650=CARTESIAN_POINT('Ctrl Pts',(3.85094025222713,-1.,-1.08655950846384));
#52651=CARTESIAN_POINT('Ctrl Pts',(3.85094025222713,1.,-1.08655950846384));
#52652=CARTESIAN_POINT('Ctrl Pts',(3.85711487933931,-1.,-1.09103825516294));
#52653=CARTESIAN_POINT('Ctrl Pts',(3.85711487933931,1.,-1.09103825516294));
#52654=CARTESIAN_POINT('Ctrl Pts',(3.86327241021247,-1.,-1.09555606505013));
#52655=CARTESIAN_POINT('Ctrl Pts',(3.86327241021247,1.,-1.09555606505013));
#52656=CARTESIAN_POINT('Ctrl Pts',(3.86941120134849,-1.,-1.10011198761195));
#52657=CARTESIAN_POINT('Ctrl Pts',(3.86941120134849,1.,-1.10011198761195));
#52658=CARTESIAN_POINT('Ctrl Pts',(3.87553067187514,-1.,-1.10470536603287));
#52659=CARTESIAN_POINT('Ctrl Pts',(3.87553067187514,1.,-1.10470536603287));
#52660=CARTESIAN_POINT('Ctrl Pts',(3.88163105531724,-1.,-1.10933577224008));
#52661=CARTESIAN_POINT('Ctrl Pts',(3.88163105531724,1.,-1.10933577224008));
#52662=CARTESIAN_POINT('Ctrl Pts',(3.88771308285171,-1.,-1.11400292434429));
#52663=CARTESIAN_POINT('Ctrl Pts',(3.88771308285171,1.,-1.11400292434429));
#52664=CARTESIAN_POINT('Ctrl Pts',(3.89377768340344,-1.,-1.11870660794603));
#52665=CARTESIAN_POINT('Ctrl Pts',(3.89377768340344,1.,-1.11870660794603));
#52666=CARTESIAN_POINT('Ctrl Pts',(3.89982569750025,-1.,-1.12344660099043));
#52667=CARTESIAN_POINT('Ctrl Pts',(3.89982569750025,1.,-1.12344660099043));
#52668=CARTESIAN_POINT('Ctrl Pts',(3.90585753318737,-1.,-1.12822258281553));
#52669=CARTESIAN_POINT('Ctrl Pts',(3.90585753318737,1.,-1.12822258281553));
#52670=CARTESIAN_POINT('Ctrl Pts',(3.91187321145649,-1.,-1.13303414693896));
#52671=CARTESIAN_POINT('Ctrl Pts',(3.91187321145649,1.,-1.13303414693896));
#52672=CARTESIAN_POINT('Ctrl Pts',(3.91787251936827,-1.,-1.13788084225554));
#52673=CARTESIAN_POINT('Ctrl Pts',(3.91787251936827,1.,-1.13788084225554));
#52674=CARTESIAN_POINT('Ctrl Pts',(3.92385513133997,-1.,-1.14276220561593));
#52675=CARTESIAN_POINT('Ctrl Pts',(3.92385513133997,1.,-1.14276220561593));
#52676=CARTESIAN_POINT('Ctrl Pts',(3.92982073294257,-1.,-1.14767779451124));
#52677=CARTESIAN_POINT('Ctrl Pts',(3.92982073294257,1.,-1.14767779451124));
#52678=CARTESIAN_POINT('Ctrl Pts',(3.9357691705628,-1.,-1.1526272271632));
#52679=CARTESIAN_POINT('Ctrl Pts',(3.9357691705628,1.,-1.1526272271632));
#52680=CARTESIAN_POINT('Ctrl Pts',(3.94170046685203,-1.,-1.15761018340956));
#52681=CARTESIAN_POINT('Ctrl Pts',(3.94170046685203,1.,-1.15761018340956));
#52682=CARTESIAN_POINT('Ctrl Pts',(3.94761474780583,-1.,-1.16262637999157));
#52683=CARTESIAN_POINT('Ctrl Pts',(3.94761474780583,1.,-1.16262637999157));
#52684=CARTESIAN_POINT('Ctrl Pts',(3.95351219509876,-1.,-1.16767555244438));
#52685=CARTESIAN_POINT('Ctrl Pts',(3.95351219509876,1.,-1.16767555244438));
#52686=CARTESIAN_POINT('Ctrl Pts',(3.95939299213276,-1.,-1.17275743590361));
#52687=CARTESIAN_POINT('Ctrl Pts',(3.95939299213276,1.,-1.17275743590361));
#52688=CARTESIAN_POINT('Ctrl Pts',(3.96525726358159,-1.,-1.17787174135592));
#52689=CARTESIAN_POINT('Ctrl Pts',(3.96525726358159,1.,-1.17787174135592));
#52690=CARTESIAN_POINT('Ctrl Pts',(3.97110505165415,-1.,-1.18301815039831));
#52691=CARTESIAN_POINT('Ctrl Pts',(3.97110505165415,1.,-1.18301815039831));
#52692=CARTESIAN_POINT('Ctrl Pts',(3.97693634767754,-1.,-1.18819633715539));
#52693=CARTESIAN_POINT('Ctrl Pts',(3.97693634767754,1.,-1.18819633715539));
#52694=CARTESIAN_POINT('Ctrl Pts',(3.98275111052561,-1.,-1.19340598349475));
#52695=CARTESIAN_POINT('Ctrl Pts',(3.98275111052561,1.,-1.19340598349475));
#52696=CARTESIAN_POINT('Ctrl Pts',(3.98854928957189,-1.,-1.19864679609566));
#52697=CARTESIAN_POINT('Ctrl Pts',(3.98854928957189,1.,-1.19864679609566));
#52698=CARTESIAN_POINT('Ctrl Pts',(3.99433084799666,-1.,-1.20391852375139));
#52699=CARTESIAN_POINT('Ctrl Pts',(3.99433084799666,1.,-1.20391852375139));
#52700=CARTESIAN_POINT('Ctrl Pts',(4.00009577950721,-1.,-1.20922097029551));
#52701=CARTESIAN_POINT('Ctrl Pts',(4.00009577950721,1.,-1.20922097029551));
#52702=CARTESIAN_POINT('Ctrl Pts',(4.00584409522722,-1.,-1.21455398918133));
#52703=CARTESIAN_POINT('Ctrl Pts',(4.00584409522722,1.,-1.21455398918133));
#52704=CARTESIAN_POINT('Ctrl Pts',(4.01042947140789,-1.,-1.21884478244403));
#52705=CARTESIAN_POINT('Ctrl Pts',(4.01042947140789,1.,-1.21884478244403));
#52706=CARTESIAN_POINT('Ctrl Pts',(4.01386104433519,-1.,-1.22207656455845));
#52707=CARTESIAN_POINT('Ctrl Pts',(4.01386104433519,1.,-1.22207656455845));
#52708=CARTESIAN_POINT('Ctrl Pts',(4.01614544569895,-1.,-1.22423716681317));
#52709=CARTESIAN_POINT('Ctrl Pts',(4.01614544569895,1.,-1.22423716681317));
#52710=CARTESIAN_POINT('Ctrl Pts',(4.01728681790024,-1.,-1.22531898815164));
#52711=CARTESIAN_POINT('Ctrl Pts',(4.01728681790024,1.,-1.22531898815164));
#52712=CARTESIAN_POINT('',(3.62400312501199,1.,-0.963899035118984));
#52713=CARTESIAN_POINT('Ctrl Pts',(3.62400312501199,-1.,-0.963899035118986));
#52714=CARTESIAN_POINT('Ctrl Pts',(3.62400312501199,-0.666666666666667,
-0.963899035118986));
#52715=CARTESIAN_POINT('Ctrl Pts',(3.62400312501199,-0.333333333333333,
-0.963899035118986));
#52716=CARTESIAN_POINT('Ctrl Pts',(3.62400312501199,0.333333333333333,-0.963899035118986));
#52717=CARTESIAN_POINT('Ctrl Pts',(3.62400312501199,0.666666666666667,-0.963899035118986));
#52718=CARTESIAN_POINT('Ctrl Pts',(3.62400312501199,1.,-0.963899035118986));
#52719=CARTESIAN_POINT('',(4.01728681790024,1.,-1.22531898815164));
#52720=CARTESIAN_POINT('',(4.01728681790024,0.,-1.22531898815164));
#52721=CARTESIAN_POINT('Ctrl Pts',(3.62400312501199,1.,-0.963899035118985));
#52722=CARTESIAN_POINT('Ctrl Pts',(3.62404828878374,1.,-0.963880158556713));
#52723=CARTESIAN_POINT('Ctrl Pts',(3.62424461507455,1.,-0.963861297423579));
#52724=CARTESIAN_POINT('Ctrl Pts',(3.62489305727516,1.,-0.96395778264259));
#52725=CARTESIAN_POINT('Ctrl Pts',(3.62652618145252,1.,-0.964373850166082));
#52726=CARTESIAN_POINT('Ctrl Pts',(3.62988252139998,1.,-0.965395153165716));
#52727=CARTESIAN_POINT('Ctrl Pts',(3.6349212208096,1.,-0.967052554540878));
#52728=CARTESIAN_POINT('Ctrl Pts',(3.64113946505393,1.,-0.969195124674829));
#52729=CARTESIAN_POINT('Ctrl Pts',(3.64819756447072,1.,-0.971722122060278));
#52730=CARTESIAN_POINT('Ctrl Pts',(3.6557157673487,1.,-0.974519971354139));
#52731=CARTESIAN_POINT('Ctrl Pts',(3.66333049637403,1.,-0.977478312751416));
#52732=CARTESIAN_POINT('Ctrl Pts',(3.67074983340444,1.,-0.980505922458495));
#52733=CARTESIAN_POINT('Ctrl Pts',(3.67782408841876,1.,-0.983550791470865));
#52734=CARTESIAN_POINT('Ctrl Pts',(3.6845531792623,1.,-0.986602639864286));
#52735=CARTESIAN_POINT('Ctrl Pts',(3.69102682138955,1.,-0.989676715398859));
#52736=CARTESIAN_POINT('Ctrl Pts',(3.69738123415696,1.,-0.992802218332104));
#52737=CARTESIAN_POINT('Ctrl Pts',(3.70375282282107,1.,-0.996009819772432));
#52738=CARTESIAN_POINT('Ctrl Pts',(3.7102243971387,1.,-0.999317260756345));
#52739=CARTESIAN_POINT('Ctrl Pts',(3.71680667125047,1.,-1.00272423396802));
#52740=CARTESIAN_POINT('Ctrl Pts',(3.72346803750544,1.,-1.00622000735696));
#52741=CARTESIAN_POINT('Ctrl Pts',(3.73015276704407,1.,-1.00978798539491));
#52742=CARTESIAN_POINT('Ctrl Pts',(3.73680245055747,1.,-1.01341114319906));
#52743=CARTESIAN_POINT('Ctrl Pts',(3.74337942504993,1.,-1.01707794311088));
#52744=CARTESIAN_POINT('Ctrl Pts',(3.74987777155873,1.,-1.02078510487439));
#52745=CARTESIAN_POINT('Ctrl Pts',(3.75631037456224,1.,-1.02453429444668));
#52746=CARTESIAN_POINT('Ctrl Pts',(3.76270122291245,1.,-1.02833014458184));
#52747=CARTESIAN_POINT('Ctrl Pts',(3.76907609832516,1.,-1.03217786604919));
#52748=CARTESIAN_POINT('Ctrl Pts',(3.77545283140427,1.,-1.03608074678008));
#52749=CARTESIAN_POINT('Ctrl Pts',(3.7818353500817,1.,-1.04003862055798));
#52750=CARTESIAN_POINT('Ctrl Pts',(3.78821910787179,1.,-1.04404924374422));
#52751=CARTESIAN_POINT('Ctrl Pts',(3.79459440308786,1.,-1.04810913267639));
#52752=CARTESIAN_POINT('Ctrl Pts',(3.80095039790681,1.,-1.05221457990016));
#52753=CARTESIAN_POINT('Ctrl Pts',(3.80727913637791,1.,-1.05636266918644));
#52754=CARTESIAN_POINT('Ctrl Pts',(3.8135786611749,1.,-1.06055206187299));
#52755=CARTESIAN_POINT('Ctrl Pts',(3.81985083953012,1.,-1.0647824403893));
#52756=CARTESIAN_POINT('Ctrl Pts',(3.82609989967276,1.,-1.06905413180359));
#52757=CARTESIAN_POINT('Ctrl Pts',(3.83233071195144,1.,-1.07336766633459));
#52758=CARTESIAN_POINT('Ctrl Pts',(3.83854714117491,1.,-1.07772335353858));
#52759=CARTESIAN_POINT('Ctrl Pts',(3.8447504803063,1.,-1.08212087917991));
#52760=CARTESIAN_POINT('Ctrl Pts',(3.85094025222713,1.,-1.08655950846384));
#52761=CARTESIAN_POINT('Ctrl Pts',(3.85711487933931,1.,-1.09103825516294));
#52762=CARTESIAN_POINT('Ctrl Pts',(3.86327241021247,1.,-1.09555606505013));
#52763=CARTESIAN_POINT('Ctrl Pts',(3.86941120134849,1.,-1.10011198761195));
#52764=CARTESIAN_POINT('Ctrl Pts',(3.87553067187514,1.,-1.10470536603287));
#52765=CARTESIAN_POINT('Ctrl Pts',(3.88163105531724,1.,-1.10933577224008));
#52766=CARTESIAN_POINT('Ctrl Pts',(3.88771308285171,1.,-1.11400292434429));
#52767=CARTESIAN_POINT('Ctrl Pts',(3.89377768340344,1.,-1.11870660794603));
#52768=CARTESIAN_POINT('Ctrl Pts',(3.89982569750025,1.,-1.12344660099043));
#52769=CARTESIAN_POINT('Ctrl Pts',(3.90585753318737,1.,-1.12822258281553));
#52770=CARTESIAN_POINT('Ctrl Pts',(3.91187321145649,1.,-1.13303414693896));
#52771=CARTESIAN_POINT('Ctrl Pts',(3.91787251936827,1.,-1.13788084225554));
#52772=CARTESIAN_POINT('Ctrl Pts',(3.92385513133997,1.,-1.14276220561593));
#52773=CARTESIAN_POINT('Ctrl Pts',(3.92982073294257,1.,-1.14767779451124));
#52774=CARTESIAN_POINT('Ctrl Pts',(3.9357691705628,1.,-1.1526272271632));
#52775=CARTESIAN_POINT('Ctrl Pts',(3.94170046685203,1.,-1.15761018340956));
#52776=CARTESIAN_POINT('Ctrl Pts',(3.94761474780583,1.,-1.16262637999157));
#52777=CARTESIAN_POINT('Ctrl Pts',(3.95351219509876,1.,-1.16767555244438));
#52778=CARTESIAN_POINT('Ctrl Pts',(3.95939299213276,1.,-1.17275743590361));
#52779=CARTESIAN_POINT('Ctrl Pts',(3.96525726358159,1.,-1.17787174135592));
#52780=CARTESIAN_POINT('Ctrl Pts',(3.97110505165415,1.,-1.18301815039831));
#52781=CARTESIAN_POINT('Ctrl Pts',(3.97693634767754,1.,-1.18819633715539));
#52782=CARTESIAN_POINT('Ctrl Pts',(3.98275111052561,1.,-1.19340598349475));
#52783=CARTESIAN_POINT('Ctrl Pts',(3.98854928957189,1.,-1.19864679609566));
#52784=CARTESIAN_POINT('Ctrl Pts',(3.99433084799666,1.,-1.20391852375139));
#52785=CARTESIAN_POINT('Ctrl Pts',(4.00009577950721,1.,-1.20922097029551));
#52786=CARTESIAN_POINT('Ctrl Pts',(4.00584409522722,1.,-1.21455398918133));
#52787=CARTESIAN_POINT('Ctrl Pts',(4.01042947140789,1.,-1.21884478244403));
#52788=CARTESIAN_POINT('Ctrl Pts',(4.01386104433519,1.,-1.22207656455845));
#52789=CARTESIAN_POINT('Ctrl Pts',(4.01614544569895,1.,-1.22423716681317));
#52790=CARTESIAN_POINT('Ctrl Pts',(4.01728681790024,1.,-1.22531898815164));
#52791=CARTESIAN_POINT('Origin',(4.01728681790024,0.,-1.22531898815164));
#52792=CARTESIAN_POINT('',(3.97027773754922,1.,-1.36999806084572));
#52793=CARTESIAN_POINT('Origin',(0.,0.,0.));
#52794=CARTESIAN_POINT('',(3.66661143271648,1.,-0.786422660833743));
#52795=CARTESIAN_POINT('Origin',(0.,1.,0.));
#52796=CARTESIAN_POINT('Ctrl Pts',(3.66661143271648,1.,-0.786422660833743));
#52797=CARTESIAN_POINT('Ctrl Pts',(3.66661143271648,0.666666666666667,-0.786422660833743));
#52798=CARTESIAN_POINT('Ctrl Pts',(3.66661143271648,0.333333333333333,-0.786422660833743));
#52799=CARTESIAN_POINT('Ctrl Pts',(3.66661143271648,-0.333333333333333,
-0.786422660833743));
#52800=CARTESIAN_POINT('Ctrl Pts',(3.66661143271648,-0.666666666666667,
-0.786422660833742));
#52801=CARTESIAN_POINT('Ctrl Pts',(3.66661143271648,-1.,-0.786422660833742));
#52802=CARTESIAN_POINT('Ctrl Pts',(4.13571194405636,-1.,-0.73204283740062));
#52803=CARTESIAN_POINT('Ctrl Pts',(4.13571194405636,1.,-0.73204283740062));
#52804=CARTESIAN_POINT('Ctrl Pts',(4.13420383737278,-1.,-0.732488575135926));
#52805=CARTESIAN_POINT('Ctrl Pts',(4.13420383737278,1.,-0.732488575135926));
#52806=CARTESIAN_POINT('Ctrl Pts',(4.13118752796397,-1.,-0.733376589325634));
#52807=CARTESIAN_POINT('Ctrl Pts',(4.13118752796397,1.,-0.733376589325634));
#52808=CARTESIAN_POINT('Ctrl Pts',(4.12666277572794,-1.,-0.734698226767513));
#52809=CARTESIAN_POINT('Ctrl Pts',(4.12666277572794,1.,-0.734698226767513));
#52810=CARTESIAN_POINT('Ctrl Pts',(4.12062919626082,-1.,-0.736439634335347));
#52811=CARTESIAN_POINT('Ctrl Pts',(4.12062919626082,1.,-0.736439634335347));
#52812=CARTESIAN_POINT('Ctrl Pts',(4.11308626953795,-1.,-0.738581708229119));
#52813=CARTESIAN_POINT('Ctrl Pts',(4.11308626953795,1.,-0.738581708229119));
#52814=CARTESIAN_POINT('Ctrl Pts',(4.1055424175856,-1.,-0.740688998555152));
#52815=CARTESIAN_POINT('Ctrl Pts',(4.1055424175856,1.,-0.740688998555152));
#52816=CARTESIAN_POINT('Ctrl Pts',(4.09799769702712,-1.,-0.742761369690018));
#52817=CARTESIAN_POINT('Ctrl Pts',(4.09799769702712,1.,-0.742761369690018));
#52818=CARTESIAN_POINT('Ctrl Pts',(4.09045220253011,-1.,-0.744798649705514));
#52819=CARTESIAN_POINT('Ctrl Pts',(4.09045220253011,1.,-0.744798649705514));
#52820=CARTESIAN_POINT('Ctrl Pts',(4.08290608094789,-1.,-0.746800631490822));
#52821=CARTESIAN_POINT('Ctrl Pts',(4.08290608094789,1.,-0.746800631490822));
#52822=CARTESIAN_POINT('Ctrl Pts',(4.07535951055363,-1.,-0.748767076679177));
#52823=CARTESIAN_POINT('Ctrl Pts',(4.07535951055363,1.,-0.748767076679177));
#52824=CARTESIAN_POINT('Ctrl Pts',(4.06781267241886,-1.,-0.750697720483176));
#52825=CARTESIAN_POINT('Ctrl Pts',(4.06781267241886,1.,-0.750697720483176));
#52826=CARTESIAN_POINT('Ctrl Pts',(4.06026572221399,-1.,-0.752592276482869));
#52827=CARTESIAN_POINT('Ctrl Pts',(4.06026572221399,1.,-0.752592276482869));
#52828=CARTESIAN_POINT('Ctrl Pts',(4.05271876688106,-1.,-0.754450441816412));
#52829=CARTESIAN_POINT('Ctrl Pts',(4.05271876688106,1.,-0.754450441816412));
#52830=CARTESIAN_POINT('Ctrl Pts',(4.04517182654344,-1.,-0.756271902370187));
#52831=CARTESIAN_POINT('Ctrl Pts',(4.04517182654344,1.,-0.756271902370187));
#52832=CARTESIAN_POINT('Ctrl Pts',(4.03762485803468,-1.,-0.758056338885554));
#52833=CARTESIAN_POINT('Ctrl Pts',(4.03762485803468,1.,-0.758056338885554));
#52834=CARTESIAN_POINT('Ctrl Pts',(4.0300778195465,-1.,-0.759803433244166));
#52835=CARTESIAN_POINT('Ctrl Pts',(4.0300778195465,1.,-0.759803433244166));
#52836=CARTESIAN_POINT('Ctrl Pts',(4.02253072741347,-1.,-0.761512875859942));
#52837=CARTESIAN_POINT('Ctrl Pts',(4.02253072741347,1.,-0.761512875859942));
#52838=CARTESIAN_POINT('Ctrl Pts',(4.01498370680434,-1.,-0.763184371182827));
#52839=CARTESIAN_POINT('Ctrl Pts',(4.01498370680434,1.,-0.763184371182827));
#52840=CARTESIAN_POINT('Ctrl Pts',(4.00743706791366,-1.,-0.764817648784947));
#52841=CARTESIAN_POINT('Ctrl Pts',(4.00743706791366,1.,-0.764817648784947));
#52842=CARTESIAN_POINT('Ctrl Pts',(3.99989129179464,-1.,-0.766412457135786));
#52843=CARTESIAN_POINT('Ctrl Pts',(3.99989129179464,1.,-0.766412457135786));
#52844=CARTESIAN_POINT('Ctrl Pts',(3.99234687880892,-1.,-0.767968531377708));
#52845=CARTESIAN_POINT('Ctrl Pts',(3.99234687880892,1.,-0.767968531377708));
#52846=CARTESIAN_POINT('Ctrl Pts',(3.98480422348403,-1.,-0.76948556624546));
#52847=CARTESIAN_POINT('Ctrl Pts',(3.98480422348403,1.,-0.76948556624546));
#52848=CARTESIAN_POINT('Ctrl Pts',(3.97726349165507,-1.,-0.770963190030504));
#52849=CARTESIAN_POINT('Ctrl Pts',(3.97726349165507,1.,-0.770963190030504));
#52850=CARTESIAN_POINT('Ctrl Pts',(3.96972446532832,-1.,-0.772400931772239));
#52851=CARTESIAN_POINT('Ctrl Pts',(3.96972446532832,1.,-0.772400931772239));
#52852=CARTESIAN_POINT('Ctrl Pts',(3.96218649639876,-1.,-0.773798212026683));
#52853=CARTESIAN_POINT('Ctrl Pts',(3.96218649639876,1.,-0.773798212026683));
#52854=CARTESIAN_POINT('Ctrl Pts',(3.95464885452364,-1.,-0.775154418039442));
#52855=CARTESIAN_POINT('Ctrl Pts',(3.95464885452364,1.,-0.775154418039442));
#52856=CARTESIAN_POINT('Ctrl Pts',(3.94711101619471,-1.,-0.77646896669796));
#52857=CARTESIAN_POINT('Ctrl Pts',(3.94711101619471,1.,-0.77646896669796));
#52858=CARTESIAN_POINT('Ctrl Pts',(3.93957296768098,-1.,-0.77774137056855));
#52859=CARTESIAN_POINT('Ctrl Pts',(3.93957296768098,1.,-0.77774137056855));
#52860=CARTESIAN_POINT('Ctrl Pts',(3.93203552473153,-1.,-0.778971308134786));
#52861=CARTESIAN_POINT('Ctrl Pts',(3.93203552473153,1.,-0.778971308134786));
#52862=CARTESIAN_POINT('Ctrl Pts',(3.92450058323799,-1.,-0.780158678615507));
#52863=CARTESIAN_POINT('Ctrl Pts',(3.92450058323799,1.,-0.780158678615507));
#52864=CARTESIAN_POINT('Ctrl Pts',(3.9169703605466,-1.,-0.781303428618344));
#52865=CARTESIAN_POINT('Ctrl Pts',(3.9169703605466,1.,-0.781303428618344));
#52866=CARTESIAN_POINT('Ctrl Pts',(3.90944671004536,-1.,-0.782405395622759));
#52867=CARTESIAN_POINT('Ctrl Pts',(3.90944671004536,1.,-0.782405395622759));
#52868=CARTESIAN_POINT('Ctrl Pts',(3.90193039043971,-1.,-0.783464141529083));
#52869=CARTESIAN_POINT('Ctrl Pts',(3.90193039043971,1.,-0.783464141529083));
#52870=CARTESIAN_POINT('Ctrl Pts',(3.89442039235105,-1.,-0.784478799358336));
#52871=CARTESIAN_POINT('Ctrl Pts',(3.89442039235105,1.,-0.784478799358336));
#52872=CARTESIAN_POINT('Ctrl Pts',(3.88691313167399,-1.,-0.785447890340723));
#52873=CARTESIAN_POINT('Ctrl Pts',(3.88691313167399,1.,-0.785447890340723));
#52874=CARTESIAN_POINT('Ctrl Pts',(3.87940402818186,-1.,-0.786369675812592));
#52875=CARTESIAN_POINT('Ctrl Pts',(3.87940402818186,1.,-0.786369675812592));
#52876=CARTESIAN_POINT('Ctrl Pts',(3.87188916600905,-1.,-0.787242527617981));
#52877=CARTESIAN_POINT('Ctrl Pts',(3.87188916600905,1.,-0.787242527617981));
#52878=CARTESIAN_POINT('Ctrl Pts',(3.86436702561342,-1.,-0.788065315093771));
#52879=CARTESIAN_POINT('Ctrl Pts',(3.86436702561342,1.,-0.788065315093771));
#52880=CARTESIAN_POINT('Ctrl Pts',(3.85683995872536,-1.,-0.788837734090688));
#52881=CARTESIAN_POINT('Ctrl Pts',(3.85683995872536,1.,-0.788837734090688));
#52882=CARTESIAN_POINT('Ctrl Pts',(3.8493163780891,-1.,-0.789560798155619));
#52883=CARTESIAN_POINT('Ctrl Pts',(3.8493163780891,1.,-0.789560798155619));
#52884=CARTESIAN_POINT('Ctrl Pts',(3.84180762342476,-1.,-0.790236124191289));
#52885=CARTESIAN_POINT('Ctrl Pts',(3.84180762342476,1.,-0.790236124191289));
#52886=CARTESIAN_POINT('Ctrl Pts',(3.83432392054804,-1.,-0.79086501270534));
#52887=CARTESIAN_POINT('Ctrl Pts',(3.83432392054804,1.,-0.79086501270534));
#52888=CARTESIAN_POINT('Ctrl Pts',(3.82687033899799,-1.,-0.791447528662381));
#52889=CARTESIAN_POINT('Ctrl Pts',(3.82687033899799,1.,-0.791447528662381));
#52890=CARTESIAN_POINT('Ctrl Pts',(3.81944345442237,-1.,-0.791981740718607));
#52891=CARTESIAN_POINT('Ctrl Pts',(3.81944345442237,1.,-0.791981740718607));
#52892=CARTESIAN_POINT('Ctrl Pts',(3.81202588694726,-1.,-0.792462483517568));
#52893=CARTESIAN_POINT('Ctrl Pts',(3.81202588694726,1.,-0.792462483517568));
#52894=CARTESIAN_POINT('Ctrl Pts',(3.80459229925598,-1.,-0.792882695234693));
#52895=CARTESIAN_POINT('Ctrl Pts',(3.80459229925598,1.,-0.792882695234693));
#52896=CARTESIAN_POINT('Ctrl Pts',(3.79711921389862,-1.,-0.793235612973201));
#52897=CARTESIAN_POINT('Ctrl Pts',(3.79711921389862,1.,-0.793235612973201));
#52898=CARTESIAN_POINT('Ctrl Pts',(3.78959439439222,-1.,-0.793516871680966));
#52899=CARTESIAN_POINT('Ctrl Pts',(3.78959439439222,1.,-0.793516871680966));
#52900=CARTESIAN_POINT('Ctrl Pts',(3.78202460377617,-1.,-0.79372623578134));
#52901=CARTESIAN_POINT('Ctrl Pts',(3.78202460377617,1.,-0.79372623578134));
#52902=CARTESIAN_POINT('Ctrl Pts',(3.77444863801264,-1.,-0.793870523787515));
#52903=CARTESIAN_POINT('Ctrl Pts',(3.77444863801264,1.,-0.793870523787515));
#52904=CARTESIAN_POINT('Ctrl Pts',(3.76692626931184,-1.,-0.793961083689141));
#52905=CARTESIAN_POINT('Ctrl Pts',(3.76692626931184,1.,-0.793961083689141));
#52906=CARTESIAN_POINT('Ctrl Pts',(3.75951468666325,-1.,-0.794008429135047));
#52907=CARTESIAN_POINT('Ctrl Pts',(3.75951468666325,1.,-0.794008429135047));
#52908=CARTESIAN_POINT('Ctrl Pts',(3.75224692493895,-1.,-0.794017347371441));
#52909=CARTESIAN_POINT('Ctrl Pts',(3.75224692493895,1.,-0.794017347371441));
#52910=CARTESIAN_POINT('Ctrl Pts',(3.74511357728827,-1.,-0.79398270045988));
#52911=CARTESIAN_POINT('Ctrl Pts',(3.74511357728827,1.,-0.79398270045988));
#52912=CARTESIAN_POINT('Ctrl Pts',(3.73803280541576,-1.,-0.793882700936791));
#52913=CARTESIAN_POINT('Ctrl Pts',(3.73803280541576,1.,-0.793882700936791));
#52914=CARTESIAN_POINT('Ctrl Pts',(3.7308691469564,-1.,-0.793682750269348));
#52915=CARTESIAN_POINT('Ctrl Pts',(3.7308691469564,1.,-0.793682750269348));
#52916=CARTESIAN_POINT('Ctrl Pts',(3.7234879729357,-1.,-0.793347023783871));
#52917=CARTESIAN_POINT('Ctrl Pts',(3.7234879729357,1.,-0.793347023783871));
#52918=CARTESIAN_POINT('Ctrl Pts',(3.7158024239604,-1.,-0.792848377370116));
#52919=CARTESIAN_POINT('Ctrl Pts',(3.7158024239604,1.,-0.792848377370116));
#52920=CARTESIAN_POINT('Ctrl Pts',(3.70781724021879,-1.,-0.792177688845968));
#52921=CARTESIAN_POINT('Ctrl Pts',(3.70781724021879,1.,-0.792177688845968));
#52922=CARTESIAN_POINT('Ctrl Pts',(3.69968940808982,-1.,-0.791356575696509));
#52923=CARTESIAN_POINT('Ctrl Pts',(3.69968940808982,1.,-0.791356575696509));
#52924=CARTESIAN_POINT('Ctrl Pts',(3.69172044327754,-1.,-0.79043628498958));
#52925=CARTESIAN_POINT('Ctrl Pts',(3.69172044327754,1.,-0.79043628498958));
#52926=CARTESIAN_POINT('Ctrl Pts',(3.68428439784285,-1.,-0.789483546065159));
#52927=CARTESIAN_POINT('Ctrl Pts',(3.68428439784285,1.,-0.789483546065159));
#52928=CARTESIAN_POINT('Ctrl Pts',(3.67777119516438,-1.,-0.788569566220663));
#52929=CARTESIAN_POINT('Ctrl Pts',(3.67777119516438,1.,-0.788569566220663));
#52930=CARTESIAN_POINT('Ctrl Pts',(3.672529236635,-1.,-0.787758799995427));
#52931=CARTESIAN_POINT('Ctrl Pts',(3.672529236635,1.,-0.787758799995427));
#52932=CARTESIAN_POINT('Ctrl Pts',(3.66879484800625,-1.,-0.787095252589508));
#52933=CARTESIAN_POINT('Ctrl Pts',(3.66879484800625,1.,-0.787095252589508));
#52934=CARTESIAN_POINT('Ctrl Pts',(3.66710211819938,-1.,-0.786698783541658));
#52935=CARTESIAN_POINT('Ctrl Pts',(3.66710211819938,1.,-0.786698783541658));
#52936=CARTESIAN_POINT('Ctrl Pts',(3.66657784454965,-1.,-0.786480236184947));
#52937=CARTESIAN_POINT('Ctrl Pts',(3.66657784454965,1.,-0.786480236184947));
#52938=CARTESIAN_POINT('Ctrl Pts',(3.66655932661846,-1.,-0.78636952818304));
#52939=CARTESIAN_POINT('Ctrl Pts',(3.66655932661846,1.,-0.78636952818304));
#52940=CARTESIAN_POINT('Ctrl Pts',(3.66663282329846,-1.,-0.786322922920599));
#52941=CARTESIAN_POINT('Ctrl Pts',(3.66663282329846,1.,-0.786322922920599));
#52942=CARTESIAN_POINT('',(4.13571194405636,1.,-0.73204283740062));
#52943=CARTESIAN_POINT('Ctrl Pts',(4.13571194405636,1.,-0.73204283740062));
#52944=CARTESIAN_POINT('Ctrl Pts',(4.13420383737278,1.,-0.732488575135926));
#52945=CARTESIAN_POINT('Ctrl Pts',(4.13118752796397,1.,-0.733376589325634));
#52946=CARTESIAN_POINT('Ctrl Pts',(4.12666277572794,1.,-0.734698226767513));
#52947=CARTESIAN_POINT('Ctrl Pts',(4.12062919626082,1.,-0.736439634335347));
#52948=CARTESIAN_POINT('Ctrl Pts',(4.11308626953795,1.,-0.738581708229119));
#52949=CARTESIAN_POINT('Ctrl Pts',(4.1055424175856,1.,-0.740688998555152));
#52950=CARTESIAN_POINT('Ctrl Pts',(4.09799769702712,1.,-0.742761369690018));
#52951=CARTESIAN_POINT('Ctrl Pts',(4.09045220253011,1.,-0.744798649705514));
#52952=CARTESIAN_POINT('Ctrl Pts',(4.08290608094789,1.,-0.746800631490822));
#52953=CARTESIAN_POINT('Ctrl Pts',(4.07535951055363,1.,-0.748767076679177));
#52954=CARTESIAN_POINT('Ctrl Pts',(4.06781267241886,1.,-0.750697720483176));
#52955=CARTESIAN_POINT('Ctrl Pts',(4.06026572221399,1.,-0.752592276482869));
#52956=CARTESIAN_POINT('Ctrl Pts',(4.05271876688106,1.,-0.754450441816412));
#52957=CARTESIAN_POINT('Ctrl Pts',(4.04517182654344,1.,-0.756271902370187));
#52958=CARTESIAN_POINT('Ctrl Pts',(4.03762485803468,1.,-0.758056338885554));
#52959=CARTESIAN_POINT('Ctrl Pts',(4.0300778195465,1.,-0.759803433244166));
#52960=CARTESIAN_POINT('Ctrl Pts',(4.02253072741347,1.,-0.761512875859942));
#52961=CARTESIAN_POINT('Ctrl Pts',(4.01498370680434,1.,-0.763184371182827));
#52962=CARTESIAN_POINT('Ctrl Pts',(4.00743706791366,1.,-0.764817648784947));
#52963=CARTESIAN_POINT('Ctrl Pts',(3.99989129179464,1.,-0.766412457135786));
#52964=CARTESIAN_POINT('Ctrl Pts',(3.99234687880892,1.,-0.767968531377708));
#52965=CARTESIAN_POINT('Ctrl Pts',(3.98480422348403,1.,-0.76948556624546));
#52966=CARTESIAN_POINT('Ctrl Pts',(3.97726349165507,1.,-0.770963190030504));
#52967=CARTESIAN_POINT('Ctrl Pts',(3.96972446532832,1.,-0.772400931772239));
#52968=CARTESIAN_POINT('Ctrl Pts',(3.96218649639876,1.,-0.773798212026683));
#52969=CARTESIAN_POINT('Ctrl Pts',(3.95464885452364,1.,-0.775154418039442));
#52970=CARTESIAN_POINT('Ctrl Pts',(3.94711101619471,1.,-0.77646896669796));
#52971=CARTESIAN_POINT('Ctrl Pts',(3.93957296768098,1.,-0.77774137056855));
#52972=CARTESIAN_POINT('Ctrl Pts',(3.93203552473153,1.,-0.778971308134786));
#52973=CARTESIAN_POINT('Ctrl Pts',(3.92450058323799,1.,-0.780158678615507));
#52974=CARTESIAN_POINT('Ctrl Pts',(3.9169703605466,1.,-0.781303428618344));
#52975=CARTESIAN_POINT('Ctrl Pts',(3.90944671004536,1.,-0.782405395622759));
#52976=CARTESIAN_POINT('Ctrl Pts',(3.90193039043971,1.,-0.783464141529083));
#52977=CARTESIAN_POINT('Ctrl Pts',(3.89442039235105,1.,-0.784478799358336));
#52978=CARTESIAN_POINT('Ctrl Pts',(3.88691313167399,1.,-0.785447890340723));
#52979=CARTESIAN_POINT('Ctrl Pts',(3.87940402818186,1.,-0.786369675812592));
#52980=CARTESIAN_POINT('Ctrl Pts',(3.87188916600905,1.,-0.787242527617981));
#52981=CARTESIAN_POINT('Ctrl Pts',(3.86436702561342,1.,-0.788065315093771));
#52982=CARTESIAN_POINT('Ctrl Pts',(3.85683995872536,1.,-0.788837734090688));
#52983=CARTESIAN_POINT('Ctrl Pts',(3.8493163780891,1.,-0.789560798155619));
#52984=CARTESIAN_POINT('Ctrl Pts',(3.84180762342476,1.,-0.790236124191289));
#52985=CARTESIAN_POINT('Ctrl Pts',(3.83432392054804,1.,-0.79086501270534));
#52986=CARTESIAN_POINT('Ctrl Pts',(3.82687033899799,1.,-0.791447528662381));
#52987=CARTESIAN_POINT('Ctrl Pts',(3.81944345442237,1.,-0.791981740718607));
#52988=CARTESIAN_POINT('Ctrl Pts',(3.81202588694726,1.,-0.792462483517568));
#52989=CARTESIAN_POINT('Ctrl Pts',(3.80459229925598,1.,-0.792882695234693));
#52990=CARTESIAN_POINT('Ctrl Pts',(3.79711921389862,1.,-0.793235612973201));
#52991=CARTESIAN_POINT('Ctrl Pts',(3.78959439439222,1.,-0.793516871680966));
#52992=CARTESIAN_POINT('Ctrl Pts',(3.78202460377617,1.,-0.79372623578134));
#52993=CARTESIAN_POINT('Ctrl Pts',(3.77444863801264,1.,-0.793870523787515));
#52994=CARTESIAN_POINT('Ctrl Pts',(3.76692626931184,1.,-0.793961083689141));
#52995=CARTESIAN_POINT('Ctrl Pts',(3.75951468666325,1.,-0.794008429135047));
#52996=CARTESIAN_POINT('Ctrl Pts',(3.75224692493895,1.,-0.794017347371441));
#52997=CARTESIAN_POINT('Ctrl Pts',(3.74511357728827,1.,-0.79398270045988));
#52998=CARTESIAN_POINT('Ctrl Pts',(3.73803280541576,1.,-0.793882700936791));
#52999=CARTESIAN_POINT('Ctrl Pts',(3.7308691469564,1.,-0.793682750269348));
#53000=CARTESIAN_POINT('Ctrl Pts',(3.7234879729357,1.,-0.793347023783871));
#53001=CARTESIAN_POINT('Ctrl Pts',(3.7158024239604,1.,-0.792848377370116));
#53002=CARTESIAN_POINT('Ctrl Pts',(3.70781724021879,1.,-0.792177688845968));
#53003=CARTESIAN_POINT('Ctrl Pts',(3.69968940808982,1.,-0.791356575696509));
#53004=CARTESIAN_POINT('Ctrl Pts',(3.69172044327754,1.,-0.79043628498958));
#53005=CARTESIAN_POINT('Ctrl Pts',(3.68428439784285,1.,-0.789483546065159));
#53006=CARTESIAN_POINT('Ctrl Pts',(3.67777119516438,1.,-0.788569566220663));
#53007=CARTESIAN_POINT('Ctrl Pts',(3.672529236635,1.,-0.787758799995427));
#53008=CARTESIAN_POINT('Ctrl Pts',(3.66907505398769,1.,-0.787145041181589));
#53009=CARTESIAN_POINT('Ctrl Pts',(3.66743103898844,1.,-0.7867743371985));
#53010=CARTESIAN_POINT('Ctrl Pts',(3.66680946938396,1.,-0.78656591955989));
#53011=CARTESIAN_POINT('Ctrl Pts',(3.66664310415236,1.,-0.786459983896781));
#53012=CARTESIAN_POINT('Ctrl Pts',(3.66661143271648,1.,-0.786422660833743));
#53013=CARTESIAN_POINT('',(4.13571194405636,0.,-0.73204283740062));
#53014=CARTESIAN_POINT('Origin',(4.15950947128175,0.,-0.581791163835815));
#53015=CARTESIAN_POINT('',(4.15950947128175,1.,-0.581791163835815));
#53016=CARTESIAN_POINT('',(4.13571194405636,1.,-0.73204283740062));
#53017=CARTESIAN_POINT('',(4.15950947128175,0.,-0.581791163835815));
#53018=CARTESIAN_POINT('Ctrl Pts',(3.73016218570874,-1.,-0.385214314776329));
#53019=CARTESIAN_POINT('Ctrl Pts',(3.73016218570874,1.,-0.385214314776329));
#53020=CARTESIAN_POINT('Ctrl Pts',(3.73010668803185,-1.,-0.385147278814804));
#53021=CARTESIAN_POINT('Ctrl Pts',(3.73010668803185,1.,-0.385147278814804));
#53022=CARTESIAN_POINT('Ctrl Pts',(3.73015851028729,-1.,-0.385047711603887));
#53023=CARTESIAN_POINT('Ctrl Pts',(3.73015851028729,1.,-0.385047711603887));
#53024=CARTESIAN_POINT('Ctrl Pts',(3.73072465900727,-1.,-0.385001870183842));
#53025=CARTESIAN_POINT('Ctrl Pts',(3.73072465900727,1.,-0.385001870183842));
#53026=CARTESIAN_POINT('Ctrl Pts',(3.73245705639337,-1.,-0.385147887989515));
#53027=CARTESIAN_POINT('Ctrl Pts',(3.73245705639337,1.,-0.385147887989515));
#53028=CARTESIAN_POINT('Ctrl Pts',(3.73621371845475,-1.,-0.385670806454744));
#53029=CARTESIAN_POINT('Ctrl Pts',(3.73621371845475,1.,-0.385670806454744));
#53030=CARTESIAN_POINT('Ctrl Pts',(3.74144965781088,-1.,-0.386519576222036));
#53031=CARTESIAN_POINT('Ctrl Pts',(3.74144965781088,1.,-0.386519576222036));
#53032=CARTESIAN_POINT('Ctrl Pts',(3.74792651696269,-1.,-0.387663020050396));
#53033=CARTESIAN_POINT('Ctrl Pts',(3.74792651696269,1.,-0.387663020050396));
#53034=CARTESIAN_POINT('Ctrl Pts',(3.75529302894757,-1.,-0.389054775898251));
#53035=CARTESIAN_POINT('Ctrl Pts',(3.75529302894757,1.,-0.389054775898251));
#53036=CARTESIAN_POINT('Ctrl Pts',(3.76315635032993,-1.,-0.390642072979259));
#53037=CARTESIAN_POINT('Ctrl Pts',(3.76315635032993,1.,-0.390642072979259));
#53038=CARTESIAN_POINT('Ctrl Pts',(3.77114011595892,-1.,-0.392372786223347));
#53039=CARTESIAN_POINT('Ctrl Pts',(3.77114011595892,1.,-0.392372786223347));
#53040=CARTESIAN_POINT('Ctrl Pts',(3.77894173114368,-1.,-0.394202481011595));
#53041=CARTESIAN_POINT('Ctrl Pts',(3.77894173114368,1.,-0.394202481011595));
#53042=CARTESIAN_POINT('Ctrl Pts',(3.78640521279479,-1.,-0.396103205335029));
#53043=CARTESIAN_POINT('Ctrl Pts',(3.78640521279479,1.,-0.396103205335029));
#53044=CARTESIAN_POINT('Ctrl Pts',(3.79352887163457,-1.,-0.398064818684159));
#53045=CARTESIAN_POINT('Ctrl Pts',(3.79352887163457,1.,-0.398064818684159));
#53046=CARTESIAN_POINT('Ctrl Pts',(3.80040370384659,-1.,-0.400088346504727));
#53047=CARTESIAN_POINT('Ctrl Pts',(3.80040370384659,1.,-0.400088346504727));
#53048=CARTESIAN_POINT('Ctrl Pts',(3.80716881962763,-1.,-0.402181320148475));
#53049=CARTESIAN_POINT('Ctrl Pts',(3.80716881962763,1.,-0.402181320148475));
#53050=CARTESIAN_POINT('Ctrl Pts',(3.81396374287762,-1.,-0.404352694628237));
#53051=CARTESIAN_POINT('Ctrl Pts',(3.81396374287762,1.,-0.404352694628237));
#53052=CARTESIAN_POINT('Ctrl Pts',(3.82087303913741,-1.,-0.406607038258907));
#53053=CARTESIAN_POINT('Ctrl Pts',(3.82087303913741,1.,-0.406607038258907));
#53054=CARTESIAN_POINT('Ctrl Pts',(3.82790724256397,-1.,-0.408942371447377));
#53055=CARTESIAN_POINT('Ctrl Pts',(3.82790724256397,1.,-0.408942371447377));
#53056=CARTESIAN_POINT('Ctrl Pts',(3.83503345578645,-1.,-0.41135303879846));
#53057=CARTESIAN_POINT('Ctrl Pts',(3.83503345578645,1.,-0.41135303879846));
#53058=CARTESIAN_POINT('Ctrl Pts',(3.84219403994742,-1.,-0.413831367016727));
#53059=CARTESIAN_POINT('Ctrl Pts',(3.84219403994742,1.,-0.413831367016727));
#53060=CARTESIAN_POINT('Ctrl Pts',(3.8493286415751,-1.,-0.41636967805292));
#53061=CARTESIAN_POINT('Ctrl Pts',(3.8493286415751,1.,-0.41636967805292));
#53062=CARTESIAN_POINT('Ctrl Pts',(3.85639825648031,-1.,-0.41896246808681));
#53063=CARTESIAN_POINT('Ctrl Pts',(3.85639825648031,1.,-0.41896246808681));
#53064=CARTESIAN_POINT('Ctrl Pts',(3.86339652542749,-1.,-0.421607423177576));
#53065=CARTESIAN_POINT('Ctrl Pts',(3.86339652542749,1.,-0.421607423177576));
#53066=CARTESIAN_POINT('Ctrl Pts',(3.87033643487882,-1.,-0.424304173195143));
#53067=CARTESIAN_POINT('Ctrl Pts',(3.87033643487882,1.,-0.424304173195143));
#53068=CARTESIAN_POINT('Ctrl Pts',(3.87724240306609,-1.,-0.427053541173469));
#53069=CARTESIAN_POINT('Ctrl Pts',(3.87724240306609,1.,-0.427053541173469));
#53070=CARTESIAN_POINT('Ctrl Pts',(3.88414070943334,-1.,-0.429856640579734));
#53071=CARTESIAN_POINT('Ctrl Pts',(3.88414070943334,1.,-0.429856640579734));
#53072=CARTESIAN_POINT('Ctrl Pts',(3.89104947940592,-1.,-0.43271392954444));
#53073=CARTESIAN_POINT('Ctrl Pts',(3.89104947940592,1.,-0.43271392954444));
#53074=CARTESIAN_POINT('Ctrl Pts',(3.8979725665544,-1.,-0.435624629433506));
#53075=CARTESIAN_POINT('Ctrl Pts',(3.8979725665544,1.,-0.435624629433506));
#53076=CARTESIAN_POINT('Ctrl Pts',(3.90490512938546,-1.,-0.438587235458234));
#53077=CARTESIAN_POINT('Ctrl Pts',(3.90490512938546,1.,-0.438587235458234));
#53078=CARTESIAN_POINT('Ctrl Pts',(3.91183704069146,-1.,-0.441599824524048));
#53079=CARTESIAN_POINT('Ctrl Pts',(3.91183704069146,1.,-0.441599824524048));
#53080=CARTESIAN_POINT('Ctrl Pts',(3.91875701610721,-1.,-0.444660430230593));
#53081=CARTESIAN_POINT('Ctrl Pts',(3.91875701610721,1.,-0.444660430230593));
#53082=CARTESIAN_POINT('Ctrl Pts',(3.92565674143424,-1.,-0.447767416837297));
#53083=CARTESIAN_POINT('Ctrl Pts',(3.92565674143424,1.,-0.447767416837297));
#53084=CARTESIAN_POINT('Ctrl Pts',(3.93253407403128,-1.,-0.450919768356347));
#53085=CARTESIAN_POINT('Ctrl Pts',(3.93253407403128,1.,-0.450919768356347));
#53086=CARTESIAN_POINT('Ctrl Pts',(3.93939080846298,-1.,-0.454116879027576));
#53087=CARTESIAN_POINT('Ctrl Pts',(3.93939080846298,1.,-0.454116879027576));
#53088=CARTESIAN_POINT('Ctrl Pts',(3.94623117206675,-1.,-0.457358410451674));
#53089=CARTESIAN_POINT('Ctrl Pts',(3.94623117206675,1.,-0.457358410451674));
#53090=CARTESIAN_POINT('Ctrl Pts',(3.95306005817363,-1.,-0.460644124429119));
#53091=CARTESIAN_POINT('Ctrl Pts',(3.95306005817363,1.,-0.460644124429119));
#53092=CARTESIAN_POINT('Ctrl Pts',(3.95988133243543,-1.,-0.463973722115745));
#53093=CARTESIAN_POINT('Ctrl Pts',(3.95988133243543,1.,-0.463973722115745));
#53094=CARTESIAN_POINT('Ctrl Pts',(3.96669622273946,-1.,-0.467346690880672));
#53095=CARTESIAN_POINT('Ctrl Pts',(3.96669622273946,1.,-0.467346690880672));
#53096=CARTESIAN_POINT('Ctrl Pts',(3.97350414289415,-1.,-0.470762379613478));
#53097=CARTESIAN_POINT('Ctrl Pts',(3.97350414289415,1.,-0.470762379613478));
#53098=CARTESIAN_POINT('Ctrl Pts',(3.9803033804443,-1.,-0.474220061019542));
#53099=CARTESIAN_POINT('Ctrl Pts',(3.9803033804443,1.,-0.474220061019542));
#53100=CARTESIAN_POINT('Ctrl Pts',(3.98709184306743,-1.,-0.477718999122033));
#53101=CARTESIAN_POINT('Ctrl Pts',(3.98709184306743,1.,-0.477718999122033));
#53102=CARTESIAN_POINT('Ctrl Pts',(3.99386775880655,-1.,-0.481258512209638));
#53103=CARTESIAN_POINT('Ctrl Pts',(3.99386775880655,1.,-0.481258512209638));
#53104=CARTESIAN_POINT('Ctrl Pts',(4.00063045119234,-1.,-0.484838042421754));
#53105=CARTESIAN_POINT('Ctrl Pts',(4.00063045119234,1.,-0.484838042421754));
#53106=CARTESIAN_POINT('Ctrl Pts',(4.0073800839092,-1.,-0.488457130424531));
#53107=CARTESIAN_POINT('Ctrl Pts',(4.0073800839092,1.,-0.488457130424531));
#53108=CARTESIAN_POINT('Ctrl Pts',(4.01411733503486,-1.,-0.492115383417931));
#53109=CARTESIAN_POINT('Ctrl Pts',(4.01411733503486,1.,-0.492115383417931));
#53110=CARTESIAN_POINT('Ctrl Pts',(4.02084308851813,-1.,-0.495812444326223));
#53111=CARTESIAN_POINT('Ctrl Pts',(4.02084308851813,1.,-0.495812444326223));
#53112=CARTESIAN_POINT('Ctrl Pts',(4.0275581398015,-1.,-0.49954796234089));
#53113=CARTESIAN_POINT('Ctrl Pts',(4.0275581398015,1.,-0.49954796234089));
#53114=CARTESIAN_POINT('Ctrl Pts',(4.0342628417439,-1.,-0.503321556915514));
#53115=CARTESIAN_POINT('Ctrl Pts',(4.0342628417439,1.,-0.503321556915514));
#53116=CARTESIAN_POINT('Ctrl Pts',(4.04095715149074,-1.,-0.507132823288362));
#53117=CARTESIAN_POINT('Ctrl Pts',(4.04095715149074,1.,-0.507132823288362));
#53118=CARTESIAN_POINT('Ctrl Pts',(4.04764078815591,-1.,-0.510981349219174));
#53119=CARTESIAN_POINT('Ctrl Pts',(4.04764078815591,1.,-0.510981349219174));
#53120=CARTESIAN_POINT('Ctrl Pts',(4.05431335771261,-1.,-0.514866728193104));
#53121=CARTESIAN_POINT('Ctrl Pts',(4.05431335771261,1.,-0.514866728193104));
#53122=CARTESIAN_POINT('Ctrl Pts',(4.06097448037934,-1.,-0.51878857233681));
#53123=CARTESIAN_POINT('Ctrl Pts',(4.06097448037934,1.,-0.51878857233681));
#53124=CARTESIAN_POINT('Ctrl Pts',(4.06762394471075,-1.,-0.522746528602768));
#53125=CARTESIAN_POINT('Ctrl Pts',(4.06762394471075,1.,-0.522746528602768));
#53126=CARTESIAN_POINT('Ctrl Pts',(4.07426172299496,-1.,-0.526740277227));
#53127=CARTESIAN_POINT('Ctrl Pts',(4.07426172299496,1.,-0.526740277227));
#53128=CARTESIAN_POINT('Ctrl Pts',(4.08088789536488,-1.,-0.530769518728076));
#53129=CARTESIAN_POINT('Ctrl Pts',(4.08088789536488,1.,-0.530769518728076));
#53130=CARTESIAN_POINT('Ctrl Pts',(4.08750259988693,-1.,-0.534833963477));
#53131=CARTESIAN_POINT('Ctrl Pts',(4.08750259988693,1.,-0.534833963477));
#53132=CARTESIAN_POINT('Ctrl Pts',(4.09410597627116,-1.,-0.538933321179921));
#53133=CARTESIAN_POINT('Ctrl Pts',(4.09410597627116,1.,-0.538933321179921));
#53134=CARTESIAN_POINT('Ctrl Pts',(4.10069810244473,-1.,-0.543067286878457));
#53135=CARTESIAN_POINT('Ctrl Pts',(4.10069810244473,1.,-0.543067286878457));
#53136=CARTESIAN_POINT('Ctrl Pts',(4.1072789702877,-1.,-0.54723553948676));
#53137=CARTESIAN_POINT('Ctrl Pts',(4.1072789702877,1.,-0.54723553948676));
#53138=CARTESIAN_POINT('Ctrl Pts',(4.11384852025578,-1.,-0.551437758498247));
#53139=CARTESIAN_POINT('Ctrl Pts',(4.11384852025578,1.,-0.551437758498247));
#53140=CARTESIAN_POINT('Ctrl Pts',(4.1204066619623,-1.,-0.555673636130778));
#53141=CARTESIAN_POINT('Ctrl Pts',(4.1204066619623,1.,-0.555673636130778));
#53142=CARTESIAN_POINT('Ctrl Pts',(4.12695329951859,-1.,-0.559942890594628));
#53143=CARTESIAN_POINT('Ctrl Pts',(4.12695329951859,1.,-0.559942890594628));
#53144=CARTESIAN_POINT('Ctrl Pts',(4.13348835726086,-1.,-0.564245279535706));
#53145=CARTESIAN_POINT('Ctrl Pts',(4.13348835726086,1.,-0.564245279535706));
#53146=CARTESIAN_POINT('Ctrl Pts',(4.14001179828669,-1.,-0.568580610187116));
#53147=CARTESIAN_POINT('Ctrl Pts',(4.14001179828669,1.,-0.568580610187116));
#53148=CARTESIAN_POINT('Ctrl Pts',(4.14652361065787,-1.,-0.572948736066277));
#53149=CARTESIAN_POINT('Ctrl Pts',(4.14652361065787,1.,-0.572948736066277));
#53150=CARTESIAN_POINT('Ctrl Pts',(4.1517237611974,-1.,-0.576469391673917));
#53151=CARTESIAN_POINT('Ctrl Pts',(4.1517237611974,1.,-0.576469391673917));
#53152=CARTESIAN_POINT('Ctrl Pts',(4.15561864787379,-1.,-0.579124568912544));
#53153=CARTESIAN_POINT('Ctrl Pts',(4.15561864787379,1.,-0.579124568912544));
#53154=CARTESIAN_POINT('Ctrl Pts',(4.15821291712391,-1.,-0.580901211462913));
#53155=CARTESIAN_POINT('Ctrl Pts',(4.15821291712391,1.,-0.580901211462913));
#53156=CARTESIAN_POINT('Ctrl Pts',(4.15950947128175,-1.,-0.581791163835815));
#53157=CARTESIAN_POINT('Ctrl Pts',(4.15950947128175,1.,-0.581791163835815));
#53158=CARTESIAN_POINT('',(3.73017266276632,1.,-0.385112848332548));
#53159=CARTESIAN_POINT('Ctrl Pts',(3.73017266276632,-1.,-0.385112848332549));
#53160=CARTESIAN_POINT('Ctrl Pts',(3.73017266276632,-0.666666666666667,
-0.385112848332549));
#53161=CARTESIAN_POINT('Ctrl Pts',(3.73017266276632,-0.333333333333333,
-0.385112848332549));
#53162=CARTESIAN_POINT('Ctrl Pts',(3.73017266276632,0.333333333333333,-0.385112848332549));
#53163=CARTESIAN_POINT('Ctrl Pts',(3.73017266276632,0.666666666666667,-0.38511284833255));
#53164=CARTESIAN_POINT('Ctrl Pts',(3.73017266276632,1.,-0.38511284833255));
#53165=CARTESIAN_POINT('Ctrl Pts',(3.73017266276632,1.,-0.385112848332549));
#53166=CARTESIAN_POINT('Ctrl Pts',(3.73021431755218,1.,-0.385087139001609));
#53167=CARTESIAN_POINT('Ctrl Pts',(3.73040527620929,1.,-0.385037797882046));
#53168=CARTESIAN_POINT('Ctrl Pts',(3.731060828624,1.,-0.385031656499142));
#53169=CARTESIAN_POINT('Ctrl Pts',(3.73273893363318,1.,-0.385187124633965));
#53170=CARTESIAN_POINT('Ctrl Pts',(3.73621371845475,1.,-0.385670806454744));
#53171=CARTESIAN_POINT('Ctrl Pts',(3.74144965781088,1.,-0.386519576222036));
#53172=CARTESIAN_POINT('Ctrl Pts',(3.74792651696269,1.,-0.387663020050396));
#53173=CARTESIAN_POINT('Ctrl Pts',(3.75529302894757,1.,-0.389054775898251));
#53174=CARTESIAN_POINT('Ctrl Pts',(3.76315635032993,1.,-0.390642072979259));
#53175=CARTESIAN_POINT('Ctrl Pts',(3.77114011595892,1.,-0.392372786223347));
#53176=CARTESIAN_POINT('Ctrl Pts',(3.77894173114368,1.,-0.394202481011595));
#53177=CARTESIAN_POINT('Ctrl Pts',(3.78640521279479,1.,-0.396103205335029));
#53178=CARTESIAN_POINT('Ctrl Pts',(3.79352887163457,1.,-0.398064818684159));
#53179=CARTESIAN_POINT('Ctrl Pts',(3.80040370384659,1.,-0.400088346504727));
#53180=CARTESIAN_POINT('Ctrl Pts',(3.80716881962763,1.,-0.402181320148475));
#53181=CARTESIAN_POINT('Ctrl Pts',(3.81396374287762,1.,-0.404352694628237));
#53182=CARTESIAN_POINT('Ctrl Pts',(3.82087303913741,1.,-0.406607038258907));
#53183=CARTESIAN_POINT('Ctrl Pts',(3.82790724256397,1.,-0.408942371447377));
#53184=CARTESIAN_POINT('Ctrl Pts',(3.83503345578645,1.,-0.41135303879846));
#53185=CARTESIAN_POINT('Ctrl Pts',(3.84219403994742,1.,-0.413831367016727));
#53186=CARTESIAN_POINT('Ctrl Pts',(3.8493286415751,1.,-0.41636967805292));
#53187=CARTESIAN_POINT('Ctrl Pts',(3.85639825648031,1.,-0.41896246808681));
#53188=CARTESIAN_POINT('Ctrl Pts',(3.86339652542749,1.,-0.421607423177576));
#53189=CARTESIAN_POINT('Ctrl Pts',(3.87033643487882,1.,-0.424304173195143));
#53190=CARTESIAN_POINT('Ctrl Pts',(3.87724240306609,1.,-0.427053541173469));
#53191=CARTESIAN_POINT('Ctrl Pts',(3.88414070943334,1.,-0.429856640579734));
#53192=CARTESIAN_POINT('Ctrl Pts',(3.89104947940592,1.,-0.43271392954444));
#53193=CARTESIAN_POINT('Ctrl Pts',(3.8979725665544,1.,-0.435624629433506));
#53194=CARTESIAN_POINT('Ctrl Pts',(3.90490512938546,1.,-0.438587235458234));
#53195=CARTESIAN_POINT('Ctrl Pts',(3.91183704069146,1.,-0.441599824524048));
#53196=CARTESIAN_POINT('Ctrl Pts',(3.91875701610721,1.,-0.444660430230593));
#53197=CARTESIAN_POINT('Ctrl Pts',(3.92565674143424,1.,-0.447767416837297));
#53198=CARTESIAN_POINT('Ctrl Pts',(3.93253407403128,1.,-0.450919768356347));
#53199=CARTESIAN_POINT('Ctrl Pts',(3.93939080846298,1.,-0.454116879027576));
#53200=CARTESIAN_POINT('Ctrl Pts',(3.94623117206675,1.,-0.457358410451674));
#53201=CARTESIAN_POINT('Ctrl Pts',(3.95306005817363,1.,-0.460644124429119));
#53202=CARTESIAN_POINT('Ctrl Pts',(3.95988133243543,1.,-0.463973722115745));
#53203=CARTESIAN_POINT('Ctrl Pts',(3.96669622273946,1.,-0.467346690880672));
#53204=CARTESIAN_POINT('Ctrl Pts',(3.97350414289415,1.,-0.470762379613478));
#53205=CARTESIAN_POINT('Ctrl Pts',(3.9803033804443,1.,-0.474220061019542));
#53206=CARTESIAN_POINT('Ctrl Pts',(3.98709184306743,1.,-0.477718999122033));
#53207=CARTESIAN_POINT('Ctrl Pts',(3.99386775880655,1.,-0.481258512209638));
#53208=CARTESIAN_POINT('Ctrl Pts',(4.00063045119234,1.,-0.484838042421754));
#53209=CARTESIAN_POINT('Ctrl Pts',(4.0073800839092,1.,-0.488457130424531));
#53210=CARTESIAN_POINT('Ctrl Pts',(4.01411733503486,1.,-0.492115383417931));
#53211=CARTESIAN_POINT('Ctrl Pts',(4.02084308851813,1.,-0.495812444326223));
#53212=CARTESIAN_POINT('Ctrl Pts',(4.0275581398015,1.,-0.49954796234089));
#53213=CARTESIAN_POINT('Ctrl Pts',(4.0342628417439,1.,-0.503321556915514));
#53214=CARTESIAN_POINT('Ctrl Pts',(4.04095715149074,1.,-0.507132823288362));
#53215=CARTESIAN_POINT('Ctrl Pts',(4.04764078815591,1.,-0.510981349219174));
#53216=CARTESIAN_POINT('Ctrl Pts',(4.05431335771261,1.,-0.514866728193104));
#53217=CARTESIAN_POINT('Ctrl Pts',(4.06097448037934,1.,-0.51878857233681));
#53218=CARTESIAN_POINT('Ctrl Pts',(4.06762394471075,1.,-0.522746528602768));
#53219=CARTESIAN_POINT('Ctrl Pts',(4.07426172299496,1.,-0.526740277227));
#53220=CARTESIAN_POINT('Ctrl Pts',(4.08088789536488,1.,-0.530769518728076));
#53221=CARTESIAN_POINT('Ctrl Pts',(4.08750259988693,1.,-0.534833963477));
#53222=CARTESIAN_POINT('Ctrl Pts',(4.09410597627116,1.,-0.538933321179921));
#53223=CARTESIAN_POINT('Ctrl Pts',(4.10069810244473,1.,-0.543067286878457));
#53224=CARTESIAN_POINT('Ctrl Pts',(4.1072789702877,1.,-0.54723553948676));
#53225=CARTESIAN_POINT('Ctrl Pts',(4.11384852025578,1.,-0.551437758498247));
#53226=CARTESIAN_POINT('Ctrl Pts',(4.1204066619623,1.,-0.555673636130778));
#53227=CARTESIAN_POINT('Ctrl Pts',(4.12695329951859,1.,-0.559942890594628));
#53228=CARTESIAN_POINT('Ctrl Pts',(4.13348835726086,1.,-0.564245279535706));
#53229=CARTESIAN_POINT('Ctrl Pts',(4.14001179828669,1.,-0.568580610187116));
#53230=CARTESIAN_POINT('Ctrl Pts',(4.14652361065787,1.,-0.572948736066277));
#53231=CARTESIAN_POINT('Ctrl Pts',(4.1517237611974,1.,-0.576469391673917));
#53232=CARTESIAN_POINT('Ctrl Pts',(4.15561864787379,1.,-0.579124568912544));
#53233=CARTESIAN_POINT('Ctrl Pts',(4.15821291712391,1.,-0.580901211462913));
#53234=CARTESIAN_POINT('Ctrl Pts',(4.15950947128175,1.,-0.581791163835815));
#53235=CARTESIAN_POINT('Origin',(0.,0.,0.));
#53236=CARTESIAN_POINT('',(3.74449296982994,1.,-0.203156094897896));
#53237=CARTESIAN_POINT('Origin',(0.,1.,0.));
#53238=CARTESIAN_POINT('Ctrl Pts',(3.74449296982994,1.,-0.203156094897896));
#53239=CARTESIAN_POINT('Ctrl Pts',(3.74449296982994,0.666666666666667,-0.203156094897896));
#53240=CARTESIAN_POINT('Ctrl Pts',(3.74449296982994,0.333333333333333,-0.203156094897896));
#53241=CARTESIAN_POINT('Ctrl Pts',(3.74449296982994,-0.333333333333333,
-0.203156094897896));
#53242=CARTESIAN_POINT('Ctrl Pts',(3.74449296982994,-0.666666666666667,
-0.203156094897895));
#53243=CARTESIAN_POINT('Ctrl Pts',(3.74449296982994,-1.,-0.203156094897895));
#53244=CARTESIAN_POINT('Ctrl Pts',(3.74449849461127,-1.,0.20305423869972));
#53245=CARTESIAN_POINT('Ctrl Pts',(3.74449849461127,1.,0.20305423869972));
#53246=CARTESIAN_POINT('Ctrl Pts',(3.7444331934681,-1.,0.203111767587923));
#53247=CARTESIAN_POINT('Ctrl Pts',(3.7444331934681,1.,0.203111767587923));
#53248=CARTESIAN_POINT('Ctrl Pts',(3.7444688019622,-1.,0.203218215748058));
#53249=CARTESIAN_POINT('Ctrl Pts',(3.7444688019622,1.,0.203218215748058));
#53250=CARTESIAN_POINT('Ctrl Pts',(3.74502080927395,-1.,0.203352057956297));
#53251=CARTESIAN_POINT('Ctrl Pts',(3.74502080927395,1.,0.203352057956297));
#53252=CARTESIAN_POINT('Ctrl Pts',(3.7467547201908,-1.,0.203478844530446));
#53253=CARTESIAN_POINT('Ctrl Pts',(3.7467547201908,1.,0.203478844530446));
#53254=CARTESIAN_POINT('Ctrl Pts',(3.75054693397875,-1.,0.203550035479166));
#53255=CARTESIAN_POINT('Ctrl Pts',(3.75054693397875,1.,0.203550035479166));
#53256=CARTESIAN_POINT('Ctrl Pts',(3.75585118707734,-1.,0.203530796848321));
#53257=CARTESIAN_POINT('Ctrl Pts',(3.75585118707734,1.,0.203530796848321));
#53258=CARTESIAN_POINT('Ctrl Pts',(3.76242717936885,-1.,0.203414634707478));
#53259=CARTESIAN_POINT('Ctrl Pts',(3.76242717936885,1.,0.203414634707478));
#53260=CARTESIAN_POINT('Ctrl Pts',(3.7699207159487,-1.,0.203192390045164));
#53261=CARTESIAN_POINT('Ctrl Pts',(3.7699207159487,1.,0.203192390045164));
#53262=CARTESIAN_POINT('Ctrl Pts',(3.77793553476614,-1.,0.20285472969908));
#53263=CARTESIAN_POINT('Ctrl Pts',(3.77793553476614,1.,0.20285472969908));
#53264=CARTESIAN_POINT('Ctrl Pts',(3.78609175019242,-1.,0.20239426051216));
#53265=CARTESIAN_POINT('Ctrl Pts',(3.78609175019242,1.,0.20239426051216));
#53266=CARTESIAN_POINT('Ctrl Pts',(3.7940835418736,-1.,0.201807533800837));
#53267=CARTESIAN_POINT('Ctrl Pts',(3.7940835418736,1.,0.201807533800837));
#53268=CARTESIAN_POINT('Ctrl Pts',(3.80175247447337,-1.,0.201097756307325));
#53269=CARTESIAN_POINT('Ctrl Pts',(3.80175247447337,1.,0.201097756307325));
#53270=CARTESIAN_POINT('Ctrl Pts',(3.80909529318669,-1.,0.200274679433364));
#53271=CARTESIAN_POINT('Ctrl Pts',(3.80909529318669,1.,0.200274679433364));
#53272=CARTESIAN_POINT('Ctrl Pts',(3.81620203429815,-1.,0.199351525297447));
#53273=CARTESIAN_POINT('Ctrl Pts',(3.81620203429815,1.,0.199351525297447));
#53274=CARTESIAN_POINT('Ctrl Pts',(3.82321127349016,-1.,0.198342616900486));
#53275=CARTESIAN_POINT('Ctrl Pts',(3.82321127349016,1.,0.198342616900486));
#53276=CARTESIAN_POINT('Ctrl Pts',(3.83026221776456,-1.,0.197260935827361));
#53277=CARTESIAN_POINT('Ctrl Pts',(3.83026221776456,1.,0.197260935827361));
#53278=CARTESIAN_POINT('Ctrl Pts',(3.83743910616195,-1.,0.196115198971858));
#53279=CARTESIAN_POINT('Ctrl Pts',(3.83743910616195,1.,0.196115198971858));
#53280=CARTESIAN_POINT('Ctrl Pts',(3.84475203346977,-1.,0.19490900946022));
#53281=CARTESIAN_POINT('Ctrl Pts',(3.84475203346977,1.,0.19490900946022));
#53282=CARTESIAN_POINT('Ctrl Pts',(3.85216762263966,-1.,0.193642806777722));
#53283=CARTESIAN_POINT('Ctrl Pts',(3.85216762263966,1.,0.193642806777722));
#53284=CARTESIAN_POINT('Ctrl Pts',(3.85962774407633,-1.,0.19231515304497));
#53285=CARTESIAN_POINT('Ctrl Pts',(3.85962774407633,1.,0.19231515304497));
#53286=CARTESIAN_POINT('Ctrl Pts',(3.86707158624783,-1.,0.190924190418619));
#53287=CARTESIAN_POINT('Ctrl Pts',(3.86707158624783,1.,0.190924190418619));
#53288=CARTESIAN_POINT('Ctrl Pts',(3.87445976418412,-1.,0.189469253358272));
#53289=CARTESIAN_POINT('Ctrl Pts',(3.87445976418412,1.,0.189469253358272));
#53290=CARTESIAN_POINT('Ctrl Pts',(3.88178563496228,-1.,0.187951632512684));
#53291=CARTESIAN_POINT('Ctrl Pts',(3.88178563496228,1.,0.187951632512684));
#53292=CARTESIAN_POINT('Ctrl Pts',(3.88906196725848,-1.,0.18637372498528));
#53293=CARTESIAN_POINT('Ctrl Pts',(3.88906196725848,1.,0.18637372498528));
#53294=CARTESIAN_POINT('Ctrl Pts',(3.89631300742646,-1.,0.184738537728042));
#53295=CARTESIAN_POINT('Ctrl Pts',(3.89631300742646,1.,0.184738537728042));
#53296=CARTESIAN_POINT('Ctrl Pts',(3.90356488555132,-1.,0.18304908199319));
#53297=CARTESIAN_POINT('Ctrl Pts',(3.90356488555132,1.,0.18304908199319));
#53298=CARTESIAN_POINT('Ctrl Pts',(3.91083557557175,-1.,0.181307740731785));
#53299=CARTESIAN_POINT('Ctrl Pts',(3.91083557557175,1.,0.181307740731785));
#53300=CARTESIAN_POINT('Ctrl Pts',(3.91812876180926,-1.,0.179515885822881));
#53301=CARTESIAN_POINT('Ctrl Pts',(3.91812876180926,1.,0.179515885822881));
#53302=CARTESIAN_POINT('Ctrl Pts',(3.92543942697655,-1.,0.177674246152317));
#53303=CARTESIAN_POINT('Ctrl Pts',(3.92543942697655,1.,0.177674246152317));
#53304=CARTESIAN_POINT('Ctrl Pts',(3.93275726771042,-1.,0.175783136893867));
#53305=CARTESIAN_POINT('Ctrl Pts',(3.93275726771042,1.,0.175783136893867));
#53306=CARTESIAN_POINT('Ctrl Pts',(3.94007083096217,-1.,0.173842734974609));
#53307=CARTESIAN_POINT('Ctrl Pts',(3.94007083096217,1.,0.173842734974609));
#53308=CARTESIAN_POINT('Ctrl Pts',(3.94737164900868,-1.,0.17185335536924));
#53309=CARTESIAN_POINT('Ctrl Pts',(3.94737164900868,1.,0.17185335536924));
#53310=CARTESIAN_POINT('Ctrl Pts',(3.95465744665268,-1.,0.169815666374138));
#53311=CARTESIAN_POINT('Ctrl Pts',(3.95465744665268,1.,0.169815666374138));
#53312=CARTESIAN_POINT('Ctrl Pts',(3.96192990160296,-1.,0.167730547023319));
#53313=CARTESIAN_POINT('Ctrl Pts',(3.96192990160296,1.,0.167730547023319));
#53314=CARTESIAN_POINT('Ctrl Pts',(3.96919313621407,-1.,0.165598992851102));
#53315=CARTESIAN_POINT('Ctrl Pts',(3.96919313621407,1.,0.165598992851102));
#53316=CARTESIAN_POINT('Ctrl Pts',(3.97645194630943,-1.,0.163422004609999));
#53317=CARTESIAN_POINT('Ctrl Pts',(3.97645194630943,1.,0.163422004609999));
#53318=CARTESIAN_POINT('Ctrl Pts',(3.98371010319872,-1.,0.161200482186084));
#53319=CARTESIAN_POINT('Ctrl Pts',(3.98371010319872,1.,0.161200482186084));
#53320=CARTESIAN_POINT('Ctrl Pts',(3.99096873945878,-1.,0.158935123982793));
#53321=CARTESIAN_POINT('Ctrl Pts',(3.99096873945878,1.,0.158935123982793));
#53322=CARTESIAN_POINT('Ctrl Pts',(3.99822717425893,-1.,0.156626481393734));
#53323=CARTESIAN_POINT('Ctrl Pts',(3.99822717425893,1.,0.156626481393734));
#53324=CARTESIAN_POINT('Ctrl Pts',(4.00548360245319,-1.,0.15427500487231));
#53325=CARTESIAN_POINT('Ctrl Pts',(4.00548360245319,1.,0.15427500487231));
#53326=CARTESIAN_POINT('Ctrl Pts',(4.01273584234689,-1.,0.15188109402291));
#53327=CARTESIAN_POINT('Ctrl Pts',(4.01273584234689,1.,0.15188109402291));
#53328=CARTESIAN_POINT('Ctrl Pts',(4.01998203715564,-1.,0.149445144968706));
#53329=CARTESIAN_POINT('Ctrl Pts',(4.01998203715564,1.,0.149445144968706));
#53330=CARTESIAN_POINT('Ctrl Pts',(4.02722143146994,-1.,0.146967602878994));
#53331=CARTESIAN_POINT('Ctrl Pts',(4.02722143146994,1.,0.146967602878994));
#53332=CARTESIAN_POINT('Ctrl Pts',(4.03445411510333,-1.,0.144448947038344));
#53333=CARTESIAN_POINT('Ctrl Pts',(4.03445411510333,1.,0.144448947038344));
#53334=CARTESIAN_POINT('Ctrl Pts',(4.04168069633781,-1.,0.1418896714855));
#53335=CARTESIAN_POINT('Ctrl Pts',(4.04168069633781,1.,0.1418896714855));
#53336=CARTESIAN_POINT('Ctrl Pts',(4.04890199238036,-1.,0.139290267180057));
#53337=CARTESIAN_POINT('Ctrl Pts',(4.04890199238036,1.,0.139290267180057));
#53338=CARTESIAN_POINT('Ctrl Pts',(4.05611873400172,-1.,0.136651205046119));
#53339=CARTESIAN_POINT('Ctrl Pts',(4.05611873400172,1.,0.136651205046119));
#53340=CARTESIAN_POINT('Ctrl Pts',(4.06333121018596,-1.,0.133972916144244));
#53341=CARTESIAN_POINT('Ctrl Pts',(4.06333121018596,1.,0.133972916144244));
#53342=CARTESIAN_POINT('Ctrl Pts',(4.0705393152874,-1.,0.13125579354894));
#53343=CARTESIAN_POINT('Ctrl Pts',(4.0705393152874,1.,0.13125579354894));
#53344=CARTESIAN_POINT('Ctrl Pts',(4.07774270738954,-1.,0.128500200484837));
#53345=CARTESIAN_POINT('Ctrl Pts',(4.07774270738954,1.,0.128500200484837));
#53346=CARTESIAN_POINT('Ctrl Pts',(4.08494093372377,-1.,0.125706476822539));
#53347=CARTESIAN_POINT('Ctrl Pts',(4.08494093372377,1.,0.125706476822539));
#53348=CARTESIAN_POINT('Ctrl Pts',(4.09213355850756,-1.,0.122874946249106));
#53349=CARTESIAN_POINT('Ctrl Pts',(4.09213355850756,1.,0.122874946249106));
#53350=CARTESIAN_POINT('Ctrl Pts',(4.09932031767002,-1.,0.120005924388124));
#53351=CARTESIAN_POINT('Ctrl Pts',(4.09932031767002,1.,0.120005924388124));
#53352=CARTESIAN_POINT('Ctrl Pts',(4.10650113381833,-1.,0.117099722731648));
#53353=CARTESIAN_POINT('Ctrl Pts',(4.10650113381833,1.,0.117099722731648));
#53354=CARTESIAN_POINT('Ctrl Pts',(4.11367603924961,-1.,0.114156649609545));
#53355=CARTESIAN_POINT('Ctrl Pts',(4.11367603924961,1.,0.114156649609545));
#53356=CARTESIAN_POINT('Ctrl Pts',(4.1208451250225,-1.,0.111177012683346));
#53357=CARTESIAN_POINT('Ctrl Pts',(4.1208451250225,1.,0.111177012683346));
#53358=CARTESIAN_POINT('Ctrl Pts',(4.12800848371504,-1.,0.108161120528369));
#53359=CARTESIAN_POINT('Ctrl Pts',(4.12800848371504,1.,0.108161120528369));
#53360=CARTESIAN_POINT('Ctrl Pts',(4.13516614458895,-1.,0.105109286538945));
#53361=CARTESIAN_POINT('Ctrl Pts',(4.13516614458895,1.,0.105109286538945));
#53362=CARTESIAN_POINT('Ctrl Pts',(4.14231804939538,-1.,0.102021826577583));
#53363=CARTESIAN_POINT('Ctrl Pts',(4.14231804939538,1.,0.102021826577583));
#53364=CARTESIAN_POINT('Ctrl Pts',(4.14946408918485,-1.,0.0988990478901221));
#53365=CARTESIAN_POINT('Ctrl Pts',(4.14946408918485,1.,0.0988990478901221));
#53366=CARTESIAN_POINT('Ctrl Pts',(4.15660412653577,-1.,0.0957412403298002));
#53367=CARTESIAN_POINT('Ctrl Pts',(4.15660412653577,1.,0.0957412403298002));
#53368=CARTESIAN_POINT('Ctrl Pts',(4.16373802265839,-1.,0.0925486672167526));
#53369=CARTESIAN_POINT('Ctrl Pts',(4.16373802265839,1.,0.0925486672167526));
#53370=CARTESIAN_POINT('Ctrl Pts',(4.17086566490794,-1.,0.0893215560848644));
#53371=CARTESIAN_POINT('Ctrl Pts',(4.17086566490794,1.,0.0893215560848644));
#53372=CARTESIAN_POINT('Ctrl Pts',(4.17798698668094,-1.,0.0860600915549391));
#53373=CARTESIAN_POINT('Ctrl Pts',(4.17798698668094,1.,0.0860600915549391));
#53374=CARTESIAN_POINT('Ctrl Pts',(4.18510195327123,-1.,0.0827644164385674));
#53375=CARTESIAN_POINT('Ctrl Pts',(4.18510195327123,1.,0.0827644164385674));
#53376=CARTESIAN_POINT('Ctrl Pts',(4.19078883320504,-1.,0.0801005887114315));
#53377=CARTESIAN_POINT('Ctrl Pts',(4.19078883320504,1.,0.0801005887114315));
#53378=CARTESIAN_POINT('Ctrl Pts',(4.19505112859416,-1.,0.0780873956242392));
#53379=CARTESIAN_POINT('Ctrl Pts',(4.19505112859416,1.,0.0780873956242392));
#53380=CARTESIAN_POINT('Ctrl Pts',(4.1978913862118,-1.,0.0767384596141459));
#53381=CARTESIAN_POINT('Ctrl Pts',(4.1978913862118,1.,0.0767384596141459));
#53382=CARTESIAN_POINT('Ctrl Pts',(4.19931119685982,-1.,0.0760622897878241));
#53383=CARTESIAN_POINT('Ctrl Pts',(4.19931119685982,1.,0.0760622897878241));
#53384=CARTESIAN_POINT('',(3.74449296983004,1.,0.2031560948961));
#53385=CARTESIAN_POINT('Ctrl Pts',(3.74449296983004,-1.,0.2031560948961));
#53386=CARTESIAN_POINT('Ctrl Pts',(3.74449296983004,-0.666666666666667,
0.2031560948961));
#53387=CARTESIAN_POINT('Ctrl Pts',(3.74449296983004,-0.333333333333333,
0.2031560948961));
#53388=CARTESIAN_POINT('Ctrl Pts',(3.74449296983004,0.333333333333333,0.2031560948961));
#53389=CARTESIAN_POINT('Ctrl Pts',(3.74449296983004,0.666666666666667,0.2031560948961));
#53390=CARTESIAN_POINT('Ctrl Pts',(3.74449296983004,1.,0.2031560948961));
#53391=CARTESIAN_POINT('',(4.19931119685982,1.,0.0760622897878241));
#53392=CARTESIAN_POINT('',(4.19931119685982,0.,0.0760622897878241));
#53393=CARTESIAN_POINT('Ctrl Pts',(3.74449296983004,1.,0.2031560948961));
#53394=CARTESIAN_POINT('Ctrl Pts',(3.74453008995092,1.,0.203188003946656));
#53395=CARTESIAN_POINT('Ctrl Pts',(3.74471097893845,1.,0.20326661011053));
#53396=CARTESIAN_POINT('Ctrl Pts',(3.74535749969115,1.,0.203375226874121));
#53397=CARTESIAN_POINT('Ctrl Pts',(3.74703926501752,1.,0.203484186269415));
#53398=CARTESIAN_POINT('Ctrl Pts',(3.75054693397875,1.,0.203550035479166));
#53399=CARTESIAN_POINT('Ctrl Pts',(3.75585118707734,1.,0.203530796848321));
#53400=CARTESIAN_POINT('Ctrl Pts',(3.76242717936885,1.,0.203414634707478));
#53401=CARTESIAN_POINT('Ctrl Pts',(3.7699207159487,1.,0.203192390045164));
#53402=CARTESIAN_POINT('Ctrl Pts',(3.77793553476614,1.,0.20285472969908));
#53403=CARTESIAN_POINT('Ctrl Pts',(3.78609175019242,1.,0.20239426051216));
#53404=CARTESIAN_POINT('Ctrl Pts',(3.7940835418736,1.,0.201807533800837));
#53405=CARTESIAN_POINT('Ctrl Pts',(3.80175247447337,1.,0.201097756307325));
#53406=CARTESIAN_POINT('Ctrl Pts',(3.80909529318669,1.,0.200274679433364));
#53407=CARTESIAN_POINT('Ctrl Pts',(3.81620203429815,1.,0.199351525297447));
#53408=CARTESIAN_POINT('Ctrl Pts',(3.82321127349016,1.,0.198342616900486));
#53409=CARTESIAN_POINT('Ctrl Pts',(3.83026221776456,1.,0.197260935827361));
#53410=CARTESIAN_POINT('Ctrl Pts',(3.83743910616195,1.,0.196115198971858));
#53411=CARTESIAN_POINT('Ctrl Pts',(3.84475203346977,1.,0.19490900946022));
#53412=CARTESIAN_POINT('Ctrl Pts',(3.85216762263966,1.,0.193642806777722));
#53413=CARTESIAN_POINT('Ctrl Pts',(3.85962774407633,1.,0.19231515304497));
#53414=CARTESIAN_POINT('Ctrl Pts',(3.86707158624783,1.,0.190924190418619));
#53415=CARTESIAN_POINT('Ctrl Pts',(3.87445976418412,1.,0.189469253358272));
#53416=CARTESIAN_POINT('Ctrl Pts',(3.88178563496228,1.,0.187951632512684));
#53417=CARTESIAN_POINT('Ctrl Pts',(3.88906196725848,1.,0.18637372498528));
#53418=CARTESIAN_POINT('Ctrl Pts',(3.89631300742646,1.,0.184738537728042));
#53419=CARTESIAN_POINT('Ctrl Pts',(3.90356488555132,1.,0.18304908199319));
#53420=CARTESIAN_POINT('Ctrl Pts',(3.91083557557175,1.,0.181307740731785));
#53421=CARTESIAN_POINT('Ctrl Pts',(3.91812876180926,1.,0.179515885822881));
#53422=CARTESIAN_POINT('Ctrl Pts',(3.92543942697655,1.,0.177674246152317));
#53423=CARTESIAN_POINT('Ctrl Pts',(3.93275726771042,1.,0.175783136893867));
#53424=CARTESIAN_POINT('Ctrl Pts',(3.94007083096217,1.,0.173842734974609));
#53425=CARTESIAN_POINT('Ctrl Pts',(3.94737164900868,1.,0.17185335536924));
#53426=CARTESIAN_POINT('Ctrl Pts',(3.95465744665268,1.,0.169815666374138));
#53427=CARTESIAN_POINT('Ctrl Pts',(3.96192990160296,1.,0.167730547023319));
#53428=CARTESIAN_POINT('Ctrl Pts',(3.96919313621407,1.,0.165598992851102));
#53429=CARTESIAN_POINT('Ctrl Pts',(3.97645194630943,1.,0.163422004609999));
#53430=CARTESIAN_POINT('Ctrl Pts',(3.98371010319872,1.,0.161200482186084));
#53431=CARTESIAN_POINT('Ctrl Pts',(3.99096873945878,1.,0.158935123982793));
#53432=CARTESIAN_POINT('Ctrl Pts',(3.99822717425893,1.,0.156626481393734));
#53433=CARTESIAN_POINT('Ctrl Pts',(4.00548360245319,1.,0.15427500487231));
#53434=CARTESIAN_POINT('Ctrl Pts',(4.01273584234689,1.,0.15188109402291));
#53435=CARTESIAN_POINT('Ctrl Pts',(4.01998203715564,1.,0.149445144968706));
#53436=CARTESIAN_POINT('Ctrl Pts',(4.02722143146994,1.,0.146967602878994));
#53437=CARTESIAN_POINT('Ctrl Pts',(4.03445411510333,1.,0.144448947038344));
#53438=CARTESIAN_POINT('Ctrl Pts',(4.04168069633781,1.,0.1418896714855));
#53439=CARTESIAN_POINT('Ctrl Pts',(4.04890199238036,1.,0.139290267180057));
#53440=CARTESIAN_POINT('Ctrl Pts',(4.05611873400172,1.,0.136651205046119));
#53441=CARTESIAN_POINT('Ctrl Pts',(4.06333121018596,1.,0.133972916144244));
#53442=CARTESIAN_POINT('Ctrl Pts',(4.0705393152874,1.,0.13125579354894));
#53443=CARTESIAN_POINT('Ctrl Pts',(4.07774270738954,1.,0.128500200484837));
#53444=CARTESIAN_POINT('Ctrl Pts',(4.08494093372377,1.,0.125706476822539));
#53445=CARTESIAN_POINT('Ctrl Pts',(4.09213355850756,1.,0.122874946249106));
#53446=CARTESIAN_POINT('Ctrl Pts',(4.09932031767002,1.,0.120005924388124));
#53447=CARTESIAN_POINT('Ctrl Pts',(4.10650113381833,1.,0.117099722731648));
#53448=CARTESIAN_POINT('Ctrl Pts',(4.11367603924961,1.,0.114156649609545));
#53449=CARTESIAN_POINT('Ctrl Pts',(4.1208451250225,1.,0.111177012683346));
#53450=CARTESIAN_POINT('Ctrl Pts',(4.12800848371504,1.,0.108161120528369));
#53451=CARTESIAN_POINT('Ctrl Pts',(4.13516614458895,1.,0.105109286538945));
#53452=CARTESIAN_POINT('Ctrl Pts',(4.14231804939538,1.,0.102021826577583));
#53453=CARTESIAN_POINT('Ctrl Pts',(4.14946408918485,1.,0.0988990478901221));
#53454=CARTESIAN_POINT('Ctrl Pts',(4.15660412653577,1.,0.0957412403298002));
#53455=CARTESIAN_POINT('Ctrl Pts',(4.16373802265839,1.,0.0925486672167526));
#53456=CARTESIAN_POINT('Ctrl Pts',(4.17086566490794,1.,0.0893215560848644));
#53457=CARTESIAN_POINT('Ctrl Pts',(4.17798698668094,1.,0.0860600915549391));
#53458=CARTESIAN_POINT('Ctrl Pts',(4.18510195327123,1.,0.0827644164385674));
#53459=CARTESIAN_POINT('Ctrl Pts',(4.19078883320504,1.,0.0801005887114315));
#53460=CARTESIAN_POINT('Ctrl Pts',(4.19505112859416,1.,0.0780873956242392));
#53461=CARTESIAN_POINT('Ctrl Pts',(4.1978913862118,1.,0.0767384596141459));
#53462=CARTESIAN_POINT('Ctrl Pts',(4.19931119685982,1.,0.0760622897878241));
#53463=CARTESIAN_POINT('Ctrl Pts',(4.19931119685982,-1.,-0.0760622897878241));
#53464=CARTESIAN_POINT('Ctrl Pts',(4.19931119685982,1.,-0.0760622897878241));
#53465=CARTESIAN_POINT('Ctrl Pts',(4.19789138621624,-1.,-0.07673845961422));
#53466=CARTESIAN_POINT('Ctrl Pts',(4.19789138621624,1.,-0.07673845961422));
#53467=CARTESIAN_POINT('Ctrl Pts',(4.19505112860624,-1.,-0.0780873956244407));
#53468=CARTESIAN_POINT('Ctrl Pts',(4.19505112860624,1.,-0.0780873956244407));
#53469=CARTESIAN_POINT('Ctrl Pts',(4.19078883322483,-1.,-0.0801005887117608));
#53470=CARTESIAN_POINT('Ctrl Pts',(4.19078883322483,1.,-0.0801005887117608));
#53471=CARTESIAN_POINT('Ctrl Pts',(4.1851019532944,-1.,-0.0827644164389515));
#53472=CARTESIAN_POINT('Ctrl Pts',(4.1851019532944,1.,-0.0827644164389515));
#53473=CARTESIAN_POINT('Ctrl Pts',(4.17798698669991,-1.,-0.086060091555252));
#53474=CARTESIAN_POINT('Ctrl Pts',(4.17798698669991,1.,-0.086060091555252));
#53475=CARTESIAN_POINT('Ctrl Pts',(4.17086566491823,-1.,-0.0893215560850332));
#53476=CARTESIAN_POINT('Ctrl Pts',(4.17086566491823,1.,-0.0893215560850332));
#53477=CARTESIAN_POINT('Ctrl Pts',(4.16373802265942,-1.,-0.0925486672167695));
#53478=CARTESIAN_POINT('Ctrl Pts',(4.16373802265942,1.,-0.0925486672167695));
#53479=CARTESIAN_POINT('Ctrl Pts',(4.15660412653006,-1.,-0.0957412403297072));
#53480=CARTESIAN_POINT('Ctrl Pts',(4.15660412653006,1.,-0.0957412403297072));
#53481=CARTESIAN_POINT('Ctrl Pts',(4.1494640891762,-1.,-0.0988990478899816));
#53482=CARTESIAN_POINT('Ctrl Pts',(4.1494640891762,1.,-0.0988990478899816));
#53483=CARTESIAN_POINT('Ctrl Pts',(4.14231804938737,-1.,-0.102021826577454));
#53484=CARTESIAN_POINT('Ctrl Pts',(4.14231804938737,1.,-0.102021826577454));
#53485=CARTESIAN_POINT('Ctrl Pts',(4.13516614458396,-1.,-0.105109286538864));
#53486=CARTESIAN_POINT('Ctrl Pts',(4.13516614458396,1.,-0.105109286538864));
#53487=CARTESIAN_POINT('Ctrl Pts',(4.12800848371386,-1.,-0.10816112052835));
#53488=CARTESIAN_POINT('Ctrl Pts',(4.12800848371386,1.,-0.10816112052835));
#53489=CARTESIAN_POINT('Ctrl Pts',(4.12084512502444,-1.,-0.111177012683378));
#53490=CARTESIAN_POINT('Ctrl Pts',(4.12084512502444,1.,-0.111177012683378));
#53491=CARTESIAN_POINT('Ctrl Pts',(4.11367603925313,-1.,-0.114156649609602));
#53492=CARTESIAN_POINT('Ctrl Pts',(4.11367603925313,1.,-0.114156649609602));
#53493=CARTESIAN_POINT('Ctrl Pts',(4.10650113382187,-1.,-0.117099722731705));
#53494=CARTESIAN_POINT('Ctrl Pts',(4.10650113382187,1.,-0.117099722731705));
#53495=CARTESIAN_POINT('Ctrl Pts',(4.09932031767243,-1.,-0.120005924388162));
#53496=CARTESIAN_POINT('Ctrl Pts',(4.09932031767243,1.,-0.120005924388162));
#53497=CARTESIAN_POINT('Ctrl Pts',(4.09213355850836,-1.,-0.122874946249119));
#53498=CARTESIAN_POINT('Ctrl Pts',(4.09213355850836,1.,-0.122874946249119));
#53499=CARTESIAN_POINT('Ctrl Pts',(4.08494093372315,-1.,-0.12570647682253));
#53500=CARTESIAN_POINT('Ctrl Pts',(4.08494093372315,1.,-0.12570647682253));
#53501=CARTESIAN_POINT('Ctrl Pts',(4.07774270738809,-1.,-0.128500200484814));
#53502=CARTESIAN_POINT('Ctrl Pts',(4.07774270738809,1.,-0.128500200484814));
#53503=CARTESIAN_POINT('Ctrl Pts',(4.07053931528579,-1.,-0.131255793548914));
#53504=CARTESIAN_POINT('Ctrl Pts',(4.07053931528579,1.,-0.131255793548914));
#53505=CARTESIAN_POINT('Ctrl Pts',(4.06333121018476,-1.,-0.133972916144225));
#53506=CARTESIAN_POINT('Ctrl Pts',(4.06333121018476,1.,-0.133972916144225));
#53507=CARTESIAN_POINT('Ctrl Pts',(4.05611873400122,-1.,-0.136651205046111));
#53508=CARTESIAN_POINT('Ctrl Pts',(4.05611873400122,1.,-0.136651205046111));
#53509=CARTESIAN_POINT('Ctrl Pts',(4.04890199238056,-1.,-0.13929026718006));
#53510=CARTESIAN_POINT('Ctrl Pts',(4.04890199238056,1.,-0.13929026718006));
#53511=CARTESIAN_POINT('Ctrl Pts',(4.04168069633842,-1.,-0.141889671485508));
#53512=CARTESIAN_POINT('Ctrl Pts',(4.04168069633842,1.,-0.141889671485508));
#53513=CARTESIAN_POINT('Ctrl Pts',(4.03445411510403,-1.,-0.144448947038352));
#53514=CARTESIAN_POINT('Ctrl Pts',(4.03445411510403,1.,-0.144448947038352));
#53515=CARTESIAN_POINT('Ctrl Pts',(4.02722143147048,-1.,-0.146967602878999));
#53516=CARTESIAN_POINT('Ctrl Pts',(4.02722143147048,1.,-0.146967602878999));
#53517=CARTESIAN_POINT('Ctrl Pts',(4.01998203715588,-1.,-0.149445144968708));
#53518=CARTESIAN_POINT('Ctrl Pts',(4.01998203715588,1.,-0.149445144968708));
#53519=CARTESIAN_POINT('Ctrl Pts',(4.01273584234684,-1.,-0.151881094022909));
#53520=CARTESIAN_POINT('Ctrl Pts',(4.01273584234684,1.,-0.151881094022909));
#53521=CARTESIAN_POINT('Ctrl Pts',(4.00548360245297,-1.,-0.15427500487231));
#53522=CARTESIAN_POINT('Ctrl Pts',(4.00548360245297,1.,-0.15427500487231));
#53523=CARTESIAN_POINT('Ctrl Pts',(3.99822717425869,-1.,-0.156626481393736));
#53524=CARTESIAN_POINT('Ctrl Pts',(3.99822717425869,1.,-0.156626481393736));
#53525=CARTESIAN_POINT('Ctrl Pts',(3.99096873945862,-1.,-0.158935123982796));
#53526=CARTESIAN_POINT('Ctrl Pts',(3.99096873945862,1.,-0.158935123982796));
#53527=CARTESIAN_POINT('Ctrl Pts',(3.98371010319866,-1.,-0.161200482186088));
#53528=CARTESIAN_POINT('Ctrl Pts',(3.98371010319866,1.,-0.161200482186088));
#53529=CARTESIAN_POINT('Ctrl Pts',(3.97645194630944,-1.,-0.163422004609999));
#53530=CARTESIAN_POINT('Ctrl Pts',(3.97645194630944,1.,-0.163422004609999));
#53531=CARTESIAN_POINT('Ctrl Pts',(3.9691931362141,-1.,-0.165598992851098));
#53532=CARTESIAN_POINT('Ctrl Pts',(3.9691931362141,1.,-0.165598992851098));
#53533=CARTESIAN_POINT('Ctrl Pts',(3.96192990160296,-1.,-0.167730547023312));
#53534=CARTESIAN_POINT('Ctrl Pts',(3.96192990160296,1.,-0.167730547023312));
#53535=CARTESIAN_POINT('Ctrl Pts',(3.95465744665263,-1.,-0.16981566637413));
#53536=CARTESIAN_POINT('Ctrl Pts',(3.95465744665263,1.,-0.16981566637413));
#53537=CARTESIAN_POINT('Ctrl Pts',(3.94737164900861,-1.,-0.171853355369233));
#53538=CARTESIAN_POINT('Ctrl Pts',(3.94737164900861,1.,-0.171853355369233));
#53539=CARTESIAN_POINT('Ctrl Pts',(3.94007083096214,-1.,-0.173842734974608));
#53540=CARTESIAN_POINT('Ctrl Pts',(3.94007083096214,1.,-0.173842734974608));
#53541=CARTESIAN_POINT('Ctrl Pts',(3.93275726771049,-1.,-0.175783136893873));
#53542=CARTESIAN_POINT('Ctrl Pts',(3.93275726771049,1.,-0.175783136893873));
#53543=CARTESIAN_POINT('Ctrl Pts',(3.92543942697672,-1.,-0.177674246152328));
#53544=CARTESIAN_POINT('Ctrl Pts',(3.92543942697672,1.,-0.177674246152328));
#53545=CARTESIAN_POINT('Ctrl Pts',(3.91812876180948,-1.,-0.179515885822895));
#53546=CARTESIAN_POINT('Ctrl Pts',(3.91812876180948,1.,-0.179515885822895));
#53547=CARTESIAN_POINT('Ctrl Pts',(3.91083557557193,-1.,-0.181307740731796));
#53548=CARTESIAN_POINT('Ctrl Pts',(3.91083557557193,1.,-0.181307740731796));
#53549=CARTESIAN_POINT('Ctrl Pts',(3.90356488555138,-1.,-0.183049081993193));
#53550=CARTESIAN_POINT('Ctrl Pts',(3.90356488555138,1.,-0.183049081993193));
#53551=CARTESIAN_POINT('Ctrl Pts',(3.89631300742633,-1.,-0.184738537728035));
#53552=CARTESIAN_POINT('Ctrl Pts',(3.89631300742633,1.,-0.184738537728035));
#53553=CARTESIAN_POINT('Ctrl Pts',(3.88906196725817,-1.,-0.186373724985263));
#53554=CARTESIAN_POINT('Ctrl Pts',(3.88906196725817,1.,-0.186373724985263));
#53555=CARTESIAN_POINT('Ctrl Pts',(3.88178563496187,-1.,-0.187951632512664));
#53556=CARTESIAN_POINT('Ctrl Pts',(3.88178563496187,1.,-0.187951632512664));
#53557=CARTESIAN_POINT('Ctrl Pts',(3.87445976418377,-1.,-0.189469253358255));
#53558=CARTESIAN_POINT('Ctrl Pts',(3.87445976418377,1.,-0.189469253358255));
#53559=CARTESIAN_POINT('Ctrl Pts',(3.8670715862477,-1.,-0.190924190418613));
#53560=CARTESIAN_POINT('Ctrl Pts',(3.8670715862477,1.,-0.190924190418613));
#53561=CARTESIAN_POINT('Ctrl Pts',(3.85962774407652,-1.,-0.19231515304498));
#53562=CARTESIAN_POINT('Ctrl Pts',(3.85962774407652,1.,-0.19231515304498));
#53563=CARTESIAN_POINT('Ctrl Pts',(3.85216762264019,-1.,-0.193642806777748));
#53564=CARTESIAN_POINT('Ctrl Pts',(3.85216762264019,1.,-0.193642806777748));
#53565=CARTESIAN_POINT('Ctrl Pts',(3.84475203347052,-1.,-0.194909009460255));
#53566=CARTESIAN_POINT('Ctrl Pts',(3.84475203347052,1.,-0.194909009460255));
#53567=CARTESIAN_POINT('Ctrl Pts',(3.83743910616265,-1.,-0.19611519897189));
#53568=CARTESIAN_POINT('Ctrl Pts',(3.83743910616265,1.,-0.19611519897189));
#53569=CARTESIAN_POINT('Ctrl Pts',(3.83026221776488,-1.,-0.197260935827375));
#53570=CARTESIAN_POINT('Ctrl Pts',(3.83026221776488,1.,-0.197260935827375));
#53571=CARTESIAN_POINT('Ctrl Pts',(3.82321127348981,-1.,-0.19834261690047));
#53572=CARTESIAN_POINT('Ctrl Pts',(3.82321127348981,1.,-0.19834261690047));
#53573=CARTESIAN_POINT('Ctrl Pts',(3.81620203429702,-1.,-0.199351525297397));
#53574=CARTESIAN_POINT('Ctrl Pts',(3.81620203429702,1.,-0.199351525297397));
#53575=CARTESIAN_POINT('Ctrl Pts',(3.80909529318501,-1.,-0.20027467943329));
#53576=CARTESIAN_POINT('Ctrl Pts',(3.80909529318501,1.,-0.20027467943329));
#53577=CARTESIAN_POINT('Ctrl Pts',(3.80175247447171,-1.,-0.201097756307252));
#53578=CARTESIAN_POINT('Ctrl Pts',(3.80175247447171,1.,-0.201097756307252));
#53579=CARTESIAN_POINT('Ctrl Pts',(3.79408354187274,-1.,-0.201807533800799));
#53580=CARTESIAN_POINT('Ctrl Pts',(3.79408354187274,1.,-0.201807533800799));
#53581=CARTESIAN_POINT('Ctrl Pts',(3.78609175019317,-1.,-0.202394260512193));
#53582=CARTESIAN_POINT('Ctrl Pts',(3.78609175019317,1.,-0.202394260512193));
#53583=CARTESIAN_POINT('Ctrl Pts',(3.77793553476879,-1.,-0.202854729699197));
#53584=CARTESIAN_POINT('Ctrl Pts',(3.77793553476879,1.,-0.202854729699197));
#53585=CARTESIAN_POINT('Ctrl Pts',(3.76992071595267,-1.,-0.203192390045338));
#53586=CARTESIAN_POINT('Ctrl Pts',(3.76992071595267,1.,-0.203192390045338));
#53587=CARTESIAN_POINT('Ctrl Pts',(3.76242717937273,-1.,-0.203414634707647));
#53588=CARTESIAN_POINT('Ctrl Pts',(3.76242717937273,1.,-0.203414634707647));
#53589=CARTESIAN_POINT('Ctrl Pts',(3.75585118707924,-1.,-0.203530796848404));
#53590=CARTESIAN_POINT('Ctrl Pts',(3.75585118707924,1.,-0.203530796848404));
#53591=CARTESIAN_POINT('Ctrl Pts',(3.75054693397716,-1.,-0.203550035479097));
#53592=CARTESIAN_POINT('Ctrl Pts',(3.75054693397716,1.,-0.203550035479097));
#53593=CARTESIAN_POINT('Ctrl Pts',(3.74675472018582,-1.,-0.20347884453023));
#53594=CARTESIAN_POINT('Ctrl Pts',(3.74675472018582,1.,-0.20347884453023));
#53595=CARTESIAN_POINT('Ctrl Pts',(3.7450208092684,-1.,-0.203352057956056));
#53596=CARTESIAN_POINT('Ctrl Pts',(3.7450208092684,1.,-0.203352057956056));
#53597=CARTESIAN_POINT('Ctrl Pts',(3.74446880195845,-1.,-0.203218215747895));
#53598=CARTESIAN_POINT('Ctrl Pts',(3.74446880195845,1.,-0.203218215747895));
#53599=CARTESIAN_POINT('Ctrl Pts',(3.74443319346666,-1.,-0.20311176758786));
#53600=CARTESIAN_POINT('Ctrl Pts',(3.74443319346666,1.,-0.20311176758786));
#53601=CARTESIAN_POINT('Ctrl Pts',(3.74449849461127,-1.,-0.20305423869972));
#53602=CARTESIAN_POINT('Ctrl Pts',(3.74449849461127,1.,-0.20305423869972));
#53603=CARTESIAN_POINT('',(4.19931119685982,1.,-0.0760622897878241));
#53604=CARTESIAN_POINT('Ctrl Pts',(4.19931119685982,1.,-0.0760622897878241));
#53605=CARTESIAN_POINT('Ctrl Pts',(4.19789138621624,1.,-0.07673845961422));
#53606=CARTESIAN_POINT('Ctrl Pts',(4.19505112860624,1.,-0.0780873956244407));
#53607=CARTESIAN_POINT('Ctrl Pts',(4.19078883322483,1.,-0.0801005887117608));
#53608=CARTESIAN_POINT('Ctrl Pts',(4.1851019532944,1.,-0.0827644164389515));
#53609=CARTESIAN_POINT('Ctrl Pts',(4.17798698669991,1.,-0.086060091555252));
#53610=CARTESIAN_POINT('Ctrl Pts',(4.17086566491823,1.,-0.0893215560850332));
#53611=CARTESIAN_POINT('Ctrl Pts',(4.16373802265942,1.,-0.0925486672167695));
#53612=CARTESIAN_POINT('Ctrl Pts',(4.15660412653006,1.,-0.0957412403297072));
#53613=CARTESIAN_POINT('Ctrl Pts',(4.1494640891762,1.,-0.0988990478899816));
#53614=CARTESIAN_POINT('Ctrl Pts',(4.14231804938737,1.,-0.102021826577454));
#53615=CARTESIAN_POINT('Ctrl Pts',(4.13516614458396,1.,-0.105109286538864));
#53616=CARTESIAN_POINT('Ctrl Pts',(4.12800848371386,1.,-0.10816112052835));
#53617=CARTESIAN_POINT('Ctrl Pts',(4.12084512502444,1.,-0.111177012683378));
#53618=CARTESIAN_POINT('Ctrl Pts',(4.11367603925313,1.,-0.114156649609602));
#53619=CARTESIAN_POINT('Ctrl Pts',(4.10650113382187,1.,-0.117099722731705));
#53620=CARTESIAN_POINT('Ctrl Pts',(4.09932031767243,1.,-0.120005924388162));
#53621=CARTESIAN_POINT('Ctrl Pts',(4.09213355850836,1.,-0.122874946249119));
#53622=CARTESIAN_POINT('Ctrl Pts',(4.08494093372315,1.,-0.12570647682253));
#53623=CARTESIAN_POINT('Ctrl Pts',(4.07774270738809,1.,-0.128500200484814));
#53624=CARTESIAN_POINT('Ctrl Pts',(4.07053931528579,1.,-0.131255793548914));
#53625=CARTESIAN_POINT('Ctrl Pts',(4.06333121018476,1.,-0.133972916144225));
#53626=CARTESIAN_POINT('Ctrl Pts',(4.05611873400122,1.,-0.136651205046111));
#53627=CARTESIAN_POINT('Ctrl Pts',(4.04890199238056,1.,-0.13929026718006));
#53628=CARTESIAN_POINT('Ctrl Pts',(4.04168069633842,1.,-0.141889671485508));
#53629=CARTESIAN_POINT('Ctrl Pts',(4.03445411510403,1.,-0.144448947038352));
#53630=CARTESIAN_POINT('Ctrl Pts',(4.02722143147048,1.,-0.146967602878999));
#53631=CARTESIAN_POINT('Ctrl Pts',(4.01998203715588,1.,-0.149445144968708));
#53632=CARTESIAN_POINT('Ctrl Pts',(4.01273584234684,1.,-0.151881094022909));
#53633=CARTESIAN_POINT('Ctrl Pts',(4.00548360245297,1.,-0.15427500487231));
#53634=CARTESIAN_POINT('Ctrl Pts',(3.99822717425869,1.,-0.156626481393736));
#53635=CARTESIAN_POINT('Ctrl Pts',(3.99096873945862,1.,-0.158935123982796));
#53636=CARTESIAN_POINT('Ctrl Pts',(3.98371010319866,1.,-0.161200482186088));
#53637=CARTESIAN_POINT('Ctrl Pts',(3.97645194630944,1.,-0.163422004609999));
#53638=CARTESIAN_POINT('Ctrl Pts',(3.9691931362141,1.,-0.165598992851098));
#53639=CARTESIAN_POINT('Ctrl Pts',(3.96192990160296,1.,-0.167730547023312));
#53640=CARTESIAN_POINT('Ctrl Pts',(3.95465744665263,1.,-0.16981566637413));
#53641=CARTESIAN_POINT('Ctrl Pts',(3.94737164900861,1.,-0.171853355369233));
#53642=CARTESIAN_POINT('Ctrl Pts',(3.94007083096214,1.,-0.173842734974608));
#53643=CARTESIAN_POINT('Ctrl Pts',(3.93275726771049,1.,-0.175783136893873));
#53644=CARTESIAN_POINT('Ctrl Pts',(3.92543942697672,1.,-0.177674246152328));
#53645=CARTESIAN_POINT('Ctrl Pts',(3.91812876180948,1.,-0.179515885822895));
#53646=CARTESIAN_POINT('Ctrl Pts',(3.91083557557193,1.,-0.181307740731796));
#53647=CARTESIAN_POINT('Ctrl Pts',(3.90356488555138,1.,-0.183049081993193));
#53648=CARTESIAN_POINT('Ctrl Pts',(3.89631300742633,1.,-0.184738537728035));
#53649=CARTESIAN_POINT('Ctrl Pts',(3.88906196725817,1.,-0.186373724985263));
#53650=CARTESIAN_POINT('Ctrl Pts',(3.88178563496187,1.,-0.187951632512664));
#53651=CARTESIAN_POINT('Ctrl Pts',(3.87445976418377,1.,-0.189469253358255));
#53652=CARTESIAN_POINT('Ctrl Pts',(3.8670715862477,1.,-0.190924190418613));
#53653=CARTESIAN_POINT('Ctrl Pts',(3.85962774407652,1.,-0.19231515304498));
#53654=CARTESIAN_POINT('Ctrl Pts',(3.85216762264019,1.,-0.193642806777748));
#53655=CARTESIAN_POINT('Ctrl Pts',(3.84475203347052,1.,-0.194909009460255));
#53656=CARTESIAN_POINT('Ctrl Pts',(3.83743910616265,1.,-0.19611519897189));
#53657=CARTESIAN_POINT('Ctrl Pts',(3.83026221776488,1.,-0.197260935827375));
#53658=CARTESIAN_POINT('Ctrl Pts',(3.82321127348981,1.,-0.19834261690047));
#53659=CARTESIAN_POINT('Ctrl Pts',(3.81620203429702,1.,-0.199351525297397));
#53660=CARTESIAN_POINT('Ctrl Pts',(3.80909529318501,1.,-0.20027467943329));
#53661=CARTESIAN_POINT('Ctrl Pts',(3.80175247447171,1.,-0.201097756307252));
#53662=CARTESIAN_POINT('Ctrl Pts',(3.79408354187274,1.,-0.201807533800799));
#53663=CARTESIAN_POINT('Ctrl Pts',(3.78609175019317,1.,-0.202394260512193));
#53664=CARTESIAN_POINT('Ctrl Pts',(3.77793553476879,1.,-0.202854729699197));
#53665=CARTESIAN_POINT('Ctrl Pts',(3.76992071595267,1.,-0.203192390045338));
#53666=CARTESIAN_POINT('Ctrl Pts',(3.76242717937273,1.,-0.203414634707647));
#53667=CARTESIAN_POINT('Ctrl Pts',(3.75585118707924,1.,-0.203530796848404));
#53668=CARTESIAN_POINT('Ctrl Pts',(3.75054693397716,1.,-0.203550035479097));
#53669=CARTESIAN_POINT('Ctrl Pts',(3.74703926501843,1.,-0.203484186269315));
#53670=CARTESIAN_POINT('Ctrl Pts',(3.74535749969262,1.,-0.203375226874332));
#53671=CARTESIAN_POINT('Ctrl Pts',(3.74471097893961,1.,-0.203266610111264));
#53672=CARTESIAN_POINT('Ctrl Pts',(3.74453008995129,1.,-0.203188003947965));
#53673=CARTESIAN_POINT('Ctrl Pts',(3.74449296982994,1.,-0.203156094897896));
#53674=CARTESIAN_POINT('',(4.19931119685982,0.,-0.0760622897878241));
#53675=CARTESIAN_POINT('Origin',(4.19931119685982,0.,0.0760622897878241));
#53676=CARTESIAN_POINT('',(4.19931119685982,1.,-0.0760622897878241));
#53677=CARTESIAN_POINT('Origin',(0.,1.,0.));
#53678=CARTESIAN_POINT('Origin',(0.,1.,0.));
#53679=CARTESIAN_POINT('Origin',(0.,0.,0.));
#53680=CARTESIAN_POINT('',(0.,0.,0.));
#53681=CARTESIAN_POINT('Origin',(-1.4,0.,0.35));
#53682=CARTESIAN_POINT('',(-1.4,-0.26,0.6));
#53683=CARTESIAN_POINT('',(-1.4,-0.3,0.56));
#53684=CARTESIAN_POINT('',(-1.4,-0.2675,0.5925));
#53685=CARTESIAN_POINT('',(-1.4,0.26,0.6));
#53686=CARTESIAN_POINT('',(-1.4,0.,0.6));
#53687=CARTESIAN_POINT('',(-1.4,0.3,0.56));
#53688=CARTESIAN_POINT('',(-1.4,0.2675,0.5925));
#53689=CARTESIAN_POINT('',(-1.4,0.3,0.04));
#53690=CARTESIAN_POINT('',(-1.4,0.3,0.175));
#53691=CARTESIAN_POINT('',(-1.4,0.26,0.));
#53692=CARTESIAN_POINT('',(-1.4,0.2925,0.0325));
#53693=CARTESIAN_POINT('',(-1.4,-0.26,0.));
#53694=CARTESIAN_POINT('',(-1.4,0.,0.));
#53695=CARTESIAN_POINT('',(-1.4,-0.3,0.04));
#53696=CARTESIAN_POINT('',(-1.4,-0.2925,0.0325));
#53697=CARTESIAN_POINT('',(-1.4,-0.3,0.175));
#53698=CARTESIAN_POINT('Origin',(0.75,0.28,0.02));
#53699=CARTESIAN_POINT('',(1.4,0.3,0.04));
#53700=CARTESIAN_POINT('',(0.75,0.3,0.04));
#53701=CARTESIAN_POINT('',(1.4,0.26,0.));
#53702=CARTESIAN_POINT('',(1.4,0.2925,0.0325));
#53703=CARTESIAN_POINT('',(0.75,0.26,0.));
#53704=CARTESIAN_POINT('Origin',(1.5,0.3,0.));
#53705=CARTESIAN_POINT('',(1.4,0.3,0.56));
#53706=CARTESIAN_POINT('',(0.75,0.3,0.56));
#53707=CARTESIAN_POINT('',(1.4,0.3,0.175));
#53708=CARTESIAN_POINT('Origin',(0.75,0.28,0.58));
#53709=CARTESIAN_POINT('',(1.4,0.26,0.6));
#53710=CARTESIAN_POINT('',(0.75,0.26,0.6));
#53711=CARTESIAN_POINT('',(1.4,0.2675,0.5925));
#53712=CARTESIAN_POINT('Origin',(0.,0.,0.6));
#53713=CARTESIAN_POINT('',(1.4,-0.26,0.6));
#53714=CARTESIAN_POINT('',(-0.75,-0.26,0.6));
#53715=CARTESIAN_POINT('',(1.4,0.,0.6));
#53716=CARTESIAN_POINT('Origin',(1.4,0.,0.35));
#53717=CARTESIAN_POINT('',(1.4,-0.26,0.));
#53718=CARTESIAN_POINT('',(1.4,-0.3,0.04));
#53719=CARTESIAN_POINT('',(1.4,-0.2925,0.0325));
#53720=CARTESIAN_POINT('',(1.4,0.,0.));
#53721=CARTESIAN_POINT('',(1.4,-0.3,0.56));
#53722=CARTESIAN_POINT('',(1.4,-0.2675,0.5925));
#53723=CARTESIAN_POINT('',(1.4,-0.3,0.175));
#53724=CARTESIAN_POINT('Origin',(0.,0.,0.));
#53725=CARTESIAN_POINT('',(-0.75,-0.26,0.));
#53726=CARTESIAN_POINT('Origin',(-0.75,-0.28,0.58));
#53727=CARTESIAN_POINT('',(-0.75,-0.3,0.56));
#53728=CARTESIAN_POINT('Origin',(-0.75,-0.28,0.02));
#53729=CARTESIAN_POINT('',(-0.75,-0.3,0.04));
#53730=CARTESIAN_POINT('Origin',(-1.5,-0.3,0.));
#53731=CARTESIAN_POINT('',(0.,0.,0.));
#53732=CARTESIAN_POINT('Origin',(0.0721687836487032,0.,-0.125));
#53733=CARTESIAN_POINT('',(0.0721687836487032,0.,-0.125));
#53734=CARTESIAN_POINT('',(0.144337567297406,0.,0.));
#53735=CARTESIAN_POINT('',(0.117710979560879,0.,-0.0461186027918559));
#53736=CARTESIAN_POINT('',(0.0721687836487032,-0.25,-0.125));
#53737=CARTESIAN_POINT('',(0.0721687836487032,0.,-0.125));
#53738=CARTESIAN_POINT('',(0.144337567297406,-0.25,0.));
#53739=CARTESIAN_POINT('',(0.144337567297406,-0.25,0.));
#53740=CARTESIAN_POINT('',(0.144337567297406,0.,0.));
#53741=CARTESIAN_POINT('Origin',(-0.0721687836487032,0.,-0.125));
#53742=CARTESIAN_POINT('',(-0.0721687836487032,0.,-0.125));
#53743=CARTESIAN_POINT('',(0.0739156081756484,0.,-0.125));
#53744=CARTESIAN_POINT('',(-0.0721687836487032,-0.25,-0.125));
#53745=CARTESIAN_POINT('',(-0.0721687836487032,0.,-0.125));
#53746=CARTESIAN_POINT('',(0.0721687836487032,-0.25,-0.125));
#53747=CARTESIAN_POINT('Origin',(-0.144337567297406,0.,-4.16333634234434E-17));
#53748=CARTESIAN_POINT('',(-0.144337567297406,0.,-1.76762539787485E-17));
#53749=CARTESIAN_POINT('',(-0.0987953713852306,0.,-0.0788813972081442));
#53750=CARTESIAN_POINT('',(-0.144337567297406,-0.25,-2.77555756156289E-17));
#53751=CARTESIAN_POINT('',(-0.144337567297406,0.,-1.76762539787485E-17));
#53752=CARTESIAN_POINT('',(-0.0721687836487032,-0.25,-0.125));
#53753=CARTESIAN_POINT('Origin',(-0.0721687836487033,0.,0.125));
#53754=CARTESIAN_POINT('',(-0.0721687836487033,0.,0.125));
#53755=CARTESIAN_POINT('',(-0.0627109795608791,0.,0.141381397208144));
#53756=CARTESIAN_POINT('',(-0.0721687836487033,-0.25,0.125));
#53757=CARTESIAN_POINT('',(-0.0721687836487033,0.,0.125));
#53758=CARTESIAN_POINT('',(-0.144337567297406,-0.25,-1.76762539787485E-17));
#53759=CARTESIAN_POINT('Origin',(0.0721687836487032,0.,0.125));
#53760=CARTESIAN_POINT('',(0.0721687836487032,0.,0.125));
#53761=CARTESIAN_POINT('',(0.146084391824352,0.,0.125));
#53762=CARTESIAN_POINT('',(0.0721687836487032,-0.25,0.125));
#53763=CARTESIAN_POINT('',(0.0721687836487032,0.,0.125));
#53764=CARTESIAN_POINT('',(-0.0721687836487033,-0.25,0.125));
#53765=CARTESIAN_POINT('Origin',(0.144337567297406,0.,0.));
#53766=CARTESIAN_POINT('',(0.153795371385231,0.,-0.0163813972081441));
#53767=CARTESIAN_POINT('',(0.0721687836487032,-0.25,0.125));
#53768=CARTESIAN_POINT('Origin',(0.,-0.25,0.));
#53769=CARTESIAN_POINT('Origin',(0.22,0.,0.));
#53770=CARTESIAN_POINT('',(-0.22,-8.67361737988404E-18,-2.69422295812418E-17));
#53771=CARTESIAN_POINT('Origin',(0.,0.,0.));
#53772=CARTESIAN_POINT('Origin',(0.,-0.015,0.));
#53773=CARTESIAN_POINT('',(-0.24505,-0.02505,-3.00099698131059E-17));
#53774=CARTESIAN_POINT('Origin',(0.,-0.02505,0.));
#53775=CARTESIAN_POINT('',(-0.235,-0.015,-2.87791997799628E-17));
#53776=CARTESIAN_POINT('Origin',(0.,-0.3775,0.));
#53777=CARTESIAN_POINT('',(-0.24505,-0.72995,3.00099698131059E-17));
#53778=CARTESIAN_POINT('Origin',(0.,-0.72995,0.));
#53779=CARTESIAN_POINT('',(-0.24505,-0.3775,-3.00099698131059E-17));
#53780=CARTESIAN_POINT('Origin',(0.,-0.7625,0.));
#53781=CARTESIAN_POINT('',(-0.175,-0.8,-2.14313189850787E-17));
#53782=CARTESIAN_POINT('Origin',(0.,-0.8,0.));
#53783=CARTESIAN_POINT('',(-0.2125,-0.7625,-2.60237444818813E-17));
#53784=CARTESIAN_POINT('Origin',(0.,-0.8,0.));
#53785=CARTESIAN_POINT('',(0.,0.,0.));
#53786=CARTESIAN_POINT('',(0.,0.,0.));
#53787=CARTESIAN_POINT('',(0.,0.,0.));
#53788=CARTESIAN_POINT('',(0.,0.,0.));
#53789=CARTESIAN_POINT('',(0.,0.,0.));
#53790=CARTESIAN_POINT('',(0.,0.,0.));
#53791=CARTESIAN_POINT('',(0.,0.,0.));
#53792=CARTESIAN_POINT('',(0.,0.,0.));
#53793=CARTESIAN_POINT('',(0.,0.6,-0.35));
#53794=CARTESIAN_POINT('',(0.,-5.1,1.4));
#53795=CARTESIAN_POINT('',(0.,5.1,1.4));
#53796=CARTESIAN_POINT('',(0.,0.,0.));
#53797=CARTESIAN_POINT('',(0.,0.,0.));
#53798=CARTESIAN_POINT('',(0.,0.,0.));
#53799=CARTESIAN_POINT('',(0.,0.,0.));
#53800=CARTESIAN_POINT('',(0.,0.,0.));
#53801=CARTESIAN_POINT('',(0.,0.,0.));
#53802=CARTESIAN_POINT('',(0.,0.,0.));
#53803=CARTESIAN_POINT('',(0.,0.,0.));
#53804=CARTESIAN_POINT('',(0.,0.6,-0.65));
#53805=CARTESIAN_POINT('',(0.,-5.1,1.8));
#53806=CARTESIAN_POINT('',(0.,5.1,1.8));
#53807=CARTESIAN_POINT('',(0.,0.,0.));
#53808=CARTESIAN_POINT('',(0.,0.,5.));
#53809=CARTESIAN_POINT('',(6.,0.,5.));
#53810=UNCERTAINTY_MEASURE_WITH_UNIT(LENGTH_MEASURE(0.001),#53910,
'DISTANCE_ACCURACY_VALUE',
'Maximum model space distance between geometric entities at asserted c
onnectivities');
#53811=UNCERTAINTY_MEASURE_WITH_UNIT(LENGTH_MEASURE(0.001),#53910,
'DISTANCE_ACCURACY_VALUE',
'Maximum model space distance between geometric entities at asserted c
onnectivities');
#53812=UNCERTAINTY_MEASURE_WITH_UNIT(LENGTH_MEASURE(0.001),#53910,
'DISTANCE_ACCURACY_VALUE',
'Maximum model space distance between geometric entities at asserted c
onnectivities');
#53813=UNCERTAINTY_MEASURE_WITH_UNIT(LENGTH_MEASURE(0.001),#53910,
'DISTANCE_ACCURACY_VALUE',
'Maximum model space distance between geometric entities at asserted c
onnectivities');
#53814=UNCERTAINTY_MEASURE_WITH_UNIT(LENGTH_MEASURE(0.001),#53910,
'DISTANCE_ACCURACY_VALUE',
'Maximum model space distance between geometric entities at asserted c
onnectivities');
#53815=UNCERTAINTY_MEASURE_WITH_UNIT(LENGTH_MEASURE(0.001),#53910,
'DISTANCE_ACCURACY_VALUE',
'Maximum model space distance between geometric entities at asserted c
onnectivities');
#53816=UNCERTAINTY_MEASURE_WITH_UNIT(LENGTH_MEASURE(0.001),#53910,
'DISTANCE_ACCURACY_VALUE',
'Maximum model space distance between geometric entities at asserted c
onnectivities');
#53817=UNCERTAINTY_MEASURE_WITH_UNIT(LENGTH_MEASURE(0.001),#53910,
'DISTANCE_ACCURACY_VALUE',
'Maximum model space distance between geometric entities at asserted c
onnectivities');
#53818=UNCERTAINTY_MEASURE_WITH_UNIT(LENGTH_MEASURE(0.001),#53910,
'DISTANCE_ACCURACY_VALUE',
'Maximum model space distance between geometric entities at asserted c
onnectivities');
#53819=UNCERTAINTY_MEASURE_WITH_UNIT(LENGTH_MEASURE(0.001),#53910,
'DISTANCE_ACCURACY_VALUE',
'Maximum model space distance between geometric entities at asserted c
onnectivities');
#53820=UNCERTAINTY_MEASURE_WITH_UNIT(LENGTH_MEASURE(0.001),#53910,
'DISTANCE_ACCURACY_VALUE',
'Maximum model space distance between geometric entities at asserted c
onnectivities');
#53821=UNCERTAINTY_MEASURE_WITH_UNIT(LENGTH_MEASURE(0.001),#53910,
'DISTANCE_ACCURACY_VALUE',
'Maximum model space distance between geometric entities at asserted c
onnectivities');
#53822=UNCERTAINTY_MEASURE_WITH_UNIT(LENGTH_MEASURE(0.001),#53910,
'DISTANCE_ACCURACY_VALUE',
'Maximum model space distance between geometric entities at asserted c
onnectivities');
#53823=UNCERTAINTY_MEASURE_WITH_UNIT(LENGTH_MEASURE(0.001),#53910,
'DISTANCE_ACCURACY_VALUE',
'Maximum model space distance between geometric entities at asserted c
onnectivities');
#53824=UNCERTAINTY_MEASURE_WITH_UNIT(LENGTH_MEASURE(0.001),#53910,
'DISTANCE_ACCURACY_VALUE',
'Maximum model space distance between geometric entities at asserted c
onnectivities');
#53825=UNCERTAINTY_MEASURE_WITH_UNIT(LENGTH_MEASURE(0.001),#53910,
'DISTANCE_ACCURACY_VALUE',
'Maximum model space distance between geometric entities at asserted c
onnectivities');
#53826=UNCERTAINTY_MEASURE_WITH_UNIT(LENGTH_MEASURE(0.001),#53910,
'DISTANCE_ACCURACY_VALUE',
'Maximum model space distance between geometric entities at asserted c
onnectivities');
#53827=UNCERTAINTY_MEASURE_WITH_UNIT(LENGTH_MEASURE(0.001),#53910,
'DISTANCE_ACCURACY_VALUE',
'Maximum model space distance between geometric entities at asserted c
onnectivities');
#53828=UNCERTAINTY_MEASURE_WITH_UNIT(LENGTH_MEASURE(0.001),#53910,
'DISTANCE_ACCURACY_VALUE',
'Maximum model space distance between geometric entities at asserted c
onnectivities');
#53829=UNCERTAINTY_MEASURE_WITH_UNIT(LENGTH_MEASURE(0.001),#53910,
'DISTANCE_ACCURACY_VALUE',
'Maximum model space distance between geometric entities at asserted c
onnectivities');
#53830=UNCERTAINTY_MEASURE_WITH_UNIT(LENGTH_MEASURE(0.001),#53910,
'DISTANCE_ACCURACY_VALUE',
'Maximum model space distance between geometric entities at asserted c
onnectivities');
#53831=UNCERTAINTY_MEASURE_WITH_UNIT(LENGTH_MEASURE(0.001),#53910,
'DISTANCE_ACCURACY_VALUE',
'Maximum model space distance between geometric entities at asserted c
onnectivities');
#53832=UNCERTAINTY_MEASURE_WITH_UNIT(LENGTH_MEASURE(0.001),#53910,
'DISTANCE_ACCURACY_VALUE',
'Maximum model space distance between geometric entities at asserted c
onnectivities');
#53833=UNCERTAINTY_MEASURE_WITH_UNIT(LENGTH_MEASURE(0.001),#53910,
'DISTANCE_ACCURACY_VALUE',
'Maximum model space distance between geometric entities at asserted c
onnectivities');
#53834=UNCERTAINTY_MEASURE_WITH_UNIT(LENGTH_MEASURE(0.001),#53910,
'DISTANCE_ACCURACY_VALUE',
'Maximum model space distance between geometric entities at asserted c
onnectivities');
#53835=UNCERTAINTY_MEASURE_WITH_UNIT(LENGTH_MEASURE(0.001),#53910,
'DISTANCE_ACCURACY_VALUE',
'Maximum model space distance between geometric entities at asserted c
onnectivities');
#53836=UNCERTAINTY_MEASURE_WITH_UNIT(LENGTH_MEASURE(0.001),#53910,
'DISTANCE_ACCURACY_VALUE',
'Maximum model space distance between geometric entities at asserted c
onnectivities');
#53837=UNCERTAINTY_MEASURE_WITH_UNIT(LENGTH_MEASURE(0.001),#53910,
'DISTANCE_ACCURACY_VALUE',
'Maximum model space distance between geometric entities at asserted c
onnectivities');
#53838=UNCERTAINTY_MEASURE_WITH_UNIT(LENGTH_MEASURE(0.001),#53910,
'DISTANCE_ACCURACY_VALUE',
'Maximum model space distance between geometric entities at asserted c
onnectivities');
#53839=UNCERTAINTY_MEASURE_WITH_UNIT(LENGTH_MEASURE(0.001),#53910,
'DISTANCE_ACCURACY_VALUE',
'Maximum model space distance between geometric entities at asserted c
onnectivities');
#53840=UNCERTAINTY_MEASURE_WITH_UNIT(LENGTH_MEASURE(0.001),#53910,
'DISTANCE_ACCURACY_VALUE',
'Maximum model space distance between geometric entities at asserted c
onnectivities');
#53841=UNCERTAINTY_MEASURE_WITH_UNIT(LENGTH_MEASURE(0.001),#53910,
'DISTANCE_ACCURACY_VALUE',
'Maximum model space distance between geometric entities at asserted c
onnectivities');
#53842=UNCERTAINTY_MEASURE_WITH_UNIT(LENGTH_MEASURE(0.001),#53910,
'DISTANCE_ACCURACY_VALUE',
'Maximum model space distance between geometric entities at asserted c
onnectivities');
#53843=UNCERTAINTY_MEASURE_WITH_UNIT(LENGTH_MEASURE(0.001),#53910,
'DISTANCE_ACCURACY_VALUE',
'Maximum model space distance between geometric entities at asserted c
onnectivities');
#53844=UNCERTAINTY_MEASURE_WITH_UNIT(LENGTH_MEASURE(0.001),#53910,
'DISTANCE_ACCURACY_VALUE',
'Maximum model space distance between geometric entities at asserted c
onnectivities');
#53845=UNCERTAINTY_MEASURE_WITH_UNIT(LENGTH_MEASURE(0.001),#53910,
'DISTANCE_ACCURACY_VALUE',
'Maximum model space distance between geometric entities at asserted c
onnectivities');
#53846=UNCERTAINTY_MEASURE_WITH_UNIT(LENGTH_MEASURE(0.001),#53910,
'DISTANCE_ACCURACY_VALUE',
'Maximum model space distance between geometric entities at asserted c
onnectivities');
#53847=UNCERTAINTY_MEASURE_WITH_UNIT(LENGTH_MEASURE(0.001),#53910,
'DISTANCE_ACCURACY_VALUE',
'Maximum model space distance between geometric entities at asserted c
onnectivities');
#53848=UNCERTAINTY_MEASURE_WITH_UNIT(LENGTH_MEASURE(0.001),#53910,
'DISTANCE_ACCURACY_VALUE',
'Maximum model space distance between geometric entities at asserted c
onnectivities');
#53849=UNCERTAINTY_MEASURE_WITH_UNIT(LENGTH_MEASURE(0.001),#53910,
'DISTANCE_ACCURACY_VALUE',
'Maximum model space distance between geometric entities at asserted c
onnectivities');
#53850=UNCERTAINTY_MEASURE_WITH_UNIT(LENGTH_MEASURE(0.001),#53910,
'DISTANCE_ACCURACY_VALUE',
'Maximum model space distance between geometric entities at asserted c
onnectivities');
#53851=UNCERTAINTY_MEASURE_WITH_UNIT(LENGTH_MEASURE(0.001),#53910,
'DISTANCE_ACCURACY_VALUE',
'Maximum model space distance between geometric entities at asserted c
onnectivities');
#53852=UNCERTAINTY_MEASURE_WITH_UNIT(LENGTH_MEASURE(0.001),#53910,
'DISTANCE_ACCURACY_VALUE',
'Maximum model space distance between geometric entities at asserted c
onnectivities');
#53853=UNCERTAINTY_MEASURE_WITH_UNIT(LENGTH_MEASURE(0.001),#53910,
'DISTANCE_ACCURACY_VALUE',
'Maximum model space distance between geometric entities at asserted c
onnectivities');
#53854=UNCERTAINTY_MEASURE_WITH_UNIT(LENGTH_MEASURE(0.001),#53910,
'DISTANCE_ACCURACY_VALUE',
'Maximum model space distance between geometric entities at asserted c
onnectivities');
#53855=UNCERTAINTY_MEASURE_WITH_UNIT(LENGTH_MEASURE(0.001),#53910,
'DISTANCE_ACCURACY_VALUE',
'Maximum model space distance between geometric entities at asserted c
onnectivities');
#53856=UNCERTAINTY_MEASURE_WITH_UNIT(LENGTH_MEASURE(0.001),#53910,
'DISTANCE_ACCURACY_VALUE',
'Maximum model space distance between geometric entities at asserted c
onnectivities');
#53857=UNCERTAINTY_MEASURE_WITH_UNIT(LENGTH_MEASURE(0.001),#53910,
'DISTANCE_ACCURACY_VALUE',
'Maximum model space distance between geometric entities at asserted c
onnectivities');
#53858=UNCERTAINTY_MEASURE_WITH_UNIT(LENGTH_MEASURE(0.001),#53910,
'DISTANCE_ACCURACY_VALUE',
'Maximum model space distance between geometric entities at asserted c
onnectivities');
#53859=UNCERTAINTY_MEASURE_WITH_UNIT(LENGTH_MEASURE(0.001),#53910,
'DISTANCE_ACCURACY_VALUE',
'Maximum model space distance between geometric entities at asserted c
onnectivities');
#53860=(
GEOMETRIC_REPRESENTATION_CONTEXT(3)
GLOBAL_UNCERTAINTY_ASSIGNED_CONTEXT((#53810))
GLOBAL_UNIT_ASSIGNED_CONTEXT((#53910,#53912,#53913))
REPRESENTATION_CONTEXT('','3D')
);
#53861=(
GEOMETRIC_REPRESENTATION_CONTEXT(3)
GLOBAL_UNCERTAINTY_ASSIGNED_CONTEXT((#53811))
GLOBAL_UNIT_ASSIGNED_CONTEXT((#53910,#53912,#53913))
REPRESENTATION_CONTEXT('','3D')
);
#53862=(
GEOMETRIC_REPRESENTATION_CONTEXT(3)
GLOBAL_UNCERTAINTY_ASSIGNED_CONTEXT((#53812))
GLOBAL_UNIT_ASSIGNED_CONTEXT((#53910,#53912,#53913))
REPRESENTATION_CONTEXT('','3D')
);
#53863=(
GEOMETRIC_REPRESENTATION_CONTEXT(3)
GLOBAL_UNCERTAINTY_ASSIGNED_CONTEXT((#53813))
GLOBAL_UNIT_ASSIGNED_CONTEXT((#53910,#53912,#53913))
REPRESENTATION_CONTEXT('','3D')
);
#53864=(
GEOMETRIC_REPRESENTATION_CONTEXT(3)
GLOBAL_UNCERTAINTY_ASSIGNED_CONTEXT((#53814))
GLOBAL_UNIT_ASSIGNED_CONTEXT((#53910,#53912,#53913))
REPRESENTATION_CONTEXT('','3D')
);
#53865=(
GEOMETRIC_REPRESENTATION_CONTEXT(3)
GLOBAL_UNCERTAINTY_ASSIGNED_CONTEXT((#53815))
GLOBAL_UNIT_ASSIGNED_CONTEXT((#53910,#53912,#53913))
REPRESENTATION_CONTEXT('','3D')
);
#53866=(
GEOMETRIC_REPRESENTATION_CONTEXT(3)
GLOBAL_UNCERTAINTY_ASSIGNED_CONTEXT((#53816))
GLOBAL_UNIT_ASSIGNED_CONTEXT((#53910,#53912,#53913))
REPRESENTATION_CONTEXT('','3D')
);
#53867=(
GEOMETRIC_REPRESENTATION_CONTEXT(3)
GLOBAL_UNCERTAINTY_ASSIGNED_CONTEXT((#53817))
GLOBAL_UNIT_ASSIGNED_CONTEXT((#53910,#53912,#53913))
REPRESENTATION_CONTEXT('','3D')
);
#53868=(
GEOMETRIC_REPRESENTATION_CONTEXT(3)
GLOBAL_UNCERTAINTY_ASSIGNED_CONTEXT((#53818))
GLOBAL_UNIT_ASSIGNED_CONTEXT((#53910,#53912,#53913))
REPRESENTATION_CONTEXT('','3D')
);
#53869=(
GEOMETRIC_REPRESENTATION_CONTEXT(3)
GLOBAL_UNCERTAINTY_ASSIGNED_CONTEXT((#53819))
GLOBAL_UNIT_ASSIGNED_CONTEXT((#53910,#53912,#53913))
REPRESENTATION_CONTEXT('','3D')
);
#53870=(
GEOMETRIC_REPRESENTATION_CONTEXT(3)
GLOBAL_UNCERTAINTY_ASSIGNED_CONTEXT((#53820))
GLOBAL_UNIT_ASSIGNED_CONTEXT((#53910,#53912,#53913))
REPRESENTATION_CONTEXT('','3D')
);
#53871=(
GEOMETRIC_REPRESENTATION_CONTEXT(3)
GLOBAL_UNCERTAINTY_ASSIGNED_CONTEXT((#53821))
GLOBAL_UNIT_ASSIGNED_CONTEXT((#53910,#53912,#53913))
REPRESENTATION_CONTEXT('','3D')
);
#53872=(
GEOMETRIC_REPRESENTATION_CONTEXT(3)
GLOBAL_UNCERTAINTY_ASSIGNED_CONTEXT((#53822))
GLOBAL_UNIT_ASSIGNED_CONTEXT((#53910,#53912,#53913))
REPRESENTATION_CONTEXT('','3D')
);
#53873=(
GEOMETRIC_REPRESENTATION_CONTEXT(3)
GLOBAL_UNCERTAINTY_ASSIGNED_CONTEXT((#53823))
GLOBAL_UNIT_ASSIGNED_CONTEXT((#53910,#53912,#53913))
REPRESENTATION_CONTEXT('','3D')
);
#53874=(
GEOMETRIC_REPRESENTATION_CONTEXT(3)
GLOBAL_UNCERTAINTY_ASSIGNED_CONTEXT((#53824))
GLOBAL_UNIT_ASSIGNED_CONTEXT((#53910,#53912,#53913))
REPRESENTATION_CONTEXT('','3D')
);
#53875=(
GEOMETRIC_REPRESENTATION_CONTEXT(3)
GLOBAL_UNCERTAINTY_ASSIGNED_CONTEXT((#53825))
GLOBAL_UNIT_ASSIGNED_CONTEXT((#53910,#53912,#53913))
REPRESENTATION_CONTEXT('','3D')
);
#53876=(
GEOMETRIC_REPRESENTATION_CONTEXT(3)
GLOBAL_UNCERTAINTY_ASSIGNED_CONTEXT((#53826))
GLOBAL_UNIT_ASSIGNED_CONTEXT((#53910,#53912,#53913))
REPRESENTATION_CONTEXT('','3D')
);
#53877=(
GEOMETRIC_REPRESENTATION_CONTEXT(3)
GLOBAL_UNCERTAINTY_ASSIGNED_CONTEXT((#53827))
GLOBAL_UNIT_ASSIGNED_CONTEXT((#53910,#53912,#53913))
REPRESENTATION_CONTEXT('','3D')
);
#53878=(
GEOMETRIC_REPRESENTATION_CONTEXT(3)
GLOBAL_UNCERTAINTY_ASSIGNED_CONTEXT((#53828))
GLOBAL_UNIT_ASSIGNED_CONTEXT((#53910,#53912,#53913))
REPRESENTATION_CONTEXT('','3D')
);
#53879=(
GEOMETRIC_REPRESENTATION_CONTEXT(3)
GLOBAL_UNCERTAINTY_ASSIGNED_CONTEXT((#53829))
GLOBAL_UNIT_ASSIGNED_CONTEXT((#53910,#53912,#53913))
REPRESENTATION_CONTEXT('','3D')
);
#53880=(
GEOMETRIC_REPRESENTATION_CONTEXT(3)
GLOBAL_UNCERTAINTY_ASSIGNED_CONTEXT((#53830))
GLOBAL_UNIT_ASSIGNED_CONTEXT((#53910,#53912,#53913))
REPRESENTATION_CONTEXT('','3D')
);
#53881=(
GEOMETRIC_REPRESENTATION_CONTEXT(3)
GLOBAL_UNCERTAINTY_ASSIGNED_CONTEXT((#53831))
GLOBAL_UNIT_ASSIGNED_CONTEXT((#53910,#53912,#53913))
REPRESENTATION_CONTEXT('','3D')
);
#53882=(
GEOMETRIC_REPRESENTATION_CONTEXT(3)
GLOBAL_UNCERTAINTY_ASSIGNED_CONTEXT((#53832))
GLOBAL_UNIT_ASSIGNED_CONTEXT((#53910,#53912,#53913))
REPRESENTATION_CONTEXT('','3D')
);
#53883=(
GEOMETRIC_REPRESENTATION_CONTEXT(3)
GLOBAL_UNCERTAINTY_ASSIGNED_CONTEXT((#53833))
GLOBAL_UNIT_ASSIGNED_CONTEXT((#53910,#53912,#53913))
REPRESENTATION_CONTEXT('','3D')
);
#53884=(
GEOMETRIC_REPRESENTATION_CONTEXT(3)
GLOBAL_UNCERTAINTY_ASSIGNED_CONTEXT((#53834))
GLOBAL_UNIT_ASSIGNED_CONTEXT((#53910,#53912,#53913))
REPRESENTATION_CONTEXT('','3D')
);
#53885=(
GEOMETRIC_REPRESENTATION_CONTEXT(3)
GLOBAL_UNCERTAINTY_ASSIGNED_CONTEXT((#53835))
GLOBAL_UNIT_ASSIGNED_CONTEXT((#53910,#53912,#53913))
REPRESENTATION_CONTEXT('','3D')
);
#53886=(
GEOMETRIC_REPRESENTATION_CONTEXT(3)
GLOBAL_UNCERTAINTY_ASSIGNED_CONTEXT((#53836))
GLOBAL_UNIT_ASSIGNED_CONTEXT((#53910,#53912,#53913))
REPRESENTATION_CONTEXT('','3D')
);
#53887=(
GEOMETRIC_REPRESENTATION_CONTEXT(3)
GLOBAL_UNCERTAINTY_ASSIGNED_CONTEXT((#53837))
GLOBAL_UNIT_ASSIGNED_CONTEXT((#53910,#53912,#53913))
REPRESENTATION_CONTEXT('','3D')
);
#53888=(
GEOMETRIC_REPRESENTATION_CONTEXT(3)
GLOBAL_UNCERTAINTY_ASSIGNED_CONTEXT((#53838))
GLOBAL_UNIT_ASSIGNED_CONTEXT((#53910,#53912,#53913))
REPRESENTATION_CONTEXT('','3D')
);
#53889=(
GEOMETRIC_REPRESENTATION_CONTEXT(3)
GLOBAL_UNCERTAINTY_ASSIGNED_CONTEXT((#53839))
GLOBAL_UNIT_ASSIGNED_CONTEXT((#53910,#53912,#53913))
REPRESENTATION_CONTEXT('','3D')
);
#53890=(
GEOMETRIC_REPRESENTATION_CONTEXT(3)
GLOBAL_UNCERTAINTY_ASSIGNED_CONTEXT((#53840))
GLOBAL_UNIT_ASSIGNED_CONTEXT((#53910,#53912,#53913))
REPRESENTATION_CONTEXT('','3D')
);
#53891=(
GEOMETRIC_REPRESENTATION_CONTEXT(3)
GLOBAL_UNCERTAINTY_ASSIGNED_CONTEXT((#53841))
GLOBAL_UNIT_ASSIGNED_CONTEXT((#53910,#53912,#53913))
REPRESENTATION_CONTEXT('','3D')
);
#53892=(
GEOMETRIC_REPRESENTATION_CONTEXT(3)
GLOBAL_UNCERTAINTY_ASSIGNED_CONTEXT((#53842))
GLOBAL_UNIT_ASSIGNED_CONTEXT((#53910,#53912,#53913))
REPRESENTATION_CONTEXT('','3D')
);
#53893=(
GEOMETRIC_REPRESENTATION_CONTEXT(3)
GLOBAL_UNCERTAINTY_ASSIGNED_CONTEXT((#53843))
GLOBAL_UNIT_ASSIGNED_CONTEXT((#53910,#53912,#53913))
REPRESENTATION_CONTEXT('','3D')
);
#53894=(
GEOMETRIC_REPRESENTATION_CONTEXT(3)
GLOBAL_UNCERTAINTY_ASSIGNED_CONTEXT((#53844))
GLOBAL_UNIT_ASSIGNED_CONTEXT((#53910,#53912,#53913))
REPRESENTATION_CONTEXT('','3D')
);
#53895=(
GEOMETRIC_REPRESENTATION_CONTEXT(3)
GLOBAL_UNCERTAINTY_ASSIGNED_CONTEXT((#53845))
GLOBAL_UNIT_ASSIGNED_CONTEXT((#53910,#53912,#53913))
REPRESENTATION_CONTEXT('','3D')
);
#53896=(
GEOMETRIC_REPRESENTATION_CONTEXT(3)
GLOBAL_UNCERTAINTY_ASSIGNED_CONTEXT((#53846))
GLOBAL_UNIT_ASSIGNED_CONTEXT((#53910,#53912,#53913))
REPRESENTATION_CONTEXT('','3D')
);
#53897=(
GEOMETRIC_REPRESENTATION_CONTEXT(3)
GLOBAL_UNCERTAINTY_ASSIGNED_CONTEXT((#53847))
GLOBAL_UNIT_ASSIGNED_CONTEXT((#53910,#53912,#53913))
REPRESENTATION_CONTEXT('','3D')
);
#53898=(
GEOMETRIC_REPRESENTATION_CONTEXT(3)
GLOBAL_UNCERTAINTY_ASSIGNED_CONTEXT((#53848))
GLOBAL_UNIT_ASSIGNED_CONTEXT((#53910,#53912,#53913))
REPRESENTATION_CONTEXT('','3D')
);
#53899=(
GEOMETRIC_REPRESENTATION_CONTEXT(3)
GLOBAL_UNCERTAINTY_ASSIGNED_CONTEXT((#53849))
GLOBAL_UNIT_ASSIGNED_CONTEXT((#53910,#53912,#53913))
REPRESENTATION_CONTEXT('','3D')
);
#53900=(
GEOMETRIC_REPRESENTATION_CONTEXT(3)
GLOBAL_UNCERTAINTY_ASSIGNED_CONTEXT((#53850))
GLOBAL_UNIT_ASSIGNED_CONTEXT((#53910,#53912,#53913))
REPRESENTATION_CONTEXT('','3D')
);
#53901=(
GEOMETRIC_REPRESENTATION_CONTEXT(3)
GLOBAL_UNCERTAINTY_ASSIGNED_CONTEXT((#53851))
GLOBAL_UNIT_ASSIGNED_CONTEXT((#53910,#53912,#53913))
REPRESENTATION_CONTEXT('','3D')
);
#53902=(
GEOMETRIC_REPRESENTATION_CONTEXT(3)
GLOBAL_UNCERTAINTY_ASSIGNED_CONTEXT((#53852))
GLOBAL_UNIT_ASSIGNED_CONTEXT((#53910,#53912,#53913))
REPRESENTATION_CONTEXT('','3D')
);
#53903=(
GEOMETRIC_REPRESENTATION_CONTEXT(3)
GLOBAL_UNCERTAINTY_ASSIGNED_CONTEXT((#53853))
GLOBAL_UNIT_ASSIGNED_CONTEXT((#53910,#53912,#53913))
REPRESENTATION_CONTEXT('','3D')
);
#53904=(
GEOMETRIC_REPRESENTATION_CONTEXT(3)
GLOBAL_UNCERTAINTY_ASSIGNED_CONTEXT((#53854))
GLOBAL_UNIT_ASSIGNED_CONTEXT((#53910,#53912,#53913))
REPRESENTATION_CONTEXT('','3D')
);
#53905=(
GEOMETRIC_REPRESENTATION_CONTEXT(3)
GLOBAL_UNCERTAINTY_ASSIGNED_CONTEXT((#53855))
GLOBAL_UNIT_ASSIGNED_CONTEXT((#53910,#53912,#53913))
REPRESENTATION_CONTEXT('','3D')
);
#53906=(
GEOMETRIC_REPRESENTATION_CONTEXT(3)
GLOBAL_UNCERTAINTY_ASSIGNED_CONTEXT((#53856))
GLOBAL_UNIT_ASSIGNED_CONTEXT((#53910,#53912,#53913))
REPRESENTATION_CONTEXT('','3D')
);
#53907=(
GEOMETRIC_REPRESENTATION_CONTEXT(3)
GLOBAL_UNCERTAINTY_ASSIGNED_CONTEXT((#53857))
GLOBAL_UNIT_ASSIGNED_CONTEXT((#53910,#53912,#53913))
REPRESENTATION_CONTEXT('','3D')
);
#53908=(
GEOMETRIC_REPRESENTATION_CONTEXT(3)
GLOBAL_UNCERTAINTY_ASSIGNED_CONTEXT((#53858))
GLOBAL_UNIT_ASSIGNED_CONTEXT((#53910,#53912,#53913))
REPRESENTATION_CONTEXT('','3D')
);
#53909=(
GEOMETRIC_REPRESENTATION_CONTEXT(3)
GLOBAL_UNCERTAINTY_ASSIGNED_CONTEXT((#53859))
GLOBAL_UNIT_ASSIGNED_CONTEXT((#53910,#53912,#53913))
REPRESENTATION_CONTEXT('','3D')
);
#53910=(
LENGTH_UNIT()
NAMED_UNIT(*)
SI_UNIT(.CENTI.,.METRE.)
);
#53911=(
LENGTH_UNIT()
NAMED_UNIT(*)
SI_UNIT($,.METRE.)
);
#53912=(
NAMED_UNIT(*)
PLANE_ANGLE_UNIT()
SI_UNIT($,.RADIAN.)
);
#53913=(
NAMED_UNIT(*)
SI_UNIT($,.STERADIAN.)
SOLID_ANGLE_UNIT()
);
#53914=SHAPE_DEFINITION_REPRESENTATION(#53963,#54086);
#53915=SHAPE_DEFINITION_REPRESENTATION(#53964,#54087);
#53916=SHAPE_DEFINITION_REPRESENTATION(#53965,#54088);
#53917=SHAPE_DEFINITION_REPRESENTATION(#53966,#54089);
#53918=SHAPE_DEFINITION_REPRESENTATION(#53967,#54090);
#53919=SHAPE_DEFINITION_REPRESENTATION(#53968,#54091);
#53920=SHAPE_DEFINITION_REPRESENTATION(#53969,#54092);
#53921=SHAPE_DEFINITION_REPRESENTATION(#53970,#54093);
#53922=SHAPE_DEFINITION_REPRESENTATION(#53971,#54094);
#53923=SHAPE_DEFINITION_REPRESENTATION(#53972,#54095);
#53924=SHAPE_DEFINITION_REPRESENTATION(#53973,#54096);
#53925=SHAPE_DEFINITION_REPRESENTATION(#53974,#54097);
#53926=SHAPE_DEFINITION_REPRESENTATION(#53975,#54098);
#53927=SHAPE_DEFINITION_REPRESENTATION(#53976,#54099);
#53928=SHAPE_DEFINITION_REPRESENTATION(#53977,#54100);
#53929=SHAPE_DEFINITION_REPRESENTATION(#53978,#54101);
#53930=SHAPE_DEFINITION_REPRESENTATION(#53979,#54102);
#53931=SHAPE_DEFINITION_REPRESENTATION(#53980,#54103);
#53932=SHAPE_DEFINITION_REPRESENTATION(#53981,#54104);
#53933=SHAPE_DEFINITION_REPRESENTATION(#53982,#54105);
#53934=SHAPE_DEFINITION_REPRESENTATION(#53983,#54106);
#53935=SHAPE_DEFINITION_REPRESENTATION(#53989,#54107);
#53936=SHAPE_DEFINITION_REPRESENTATION(#53990,#54108);
#53937=SHAPE_DEFINITION_REPRESENTATION(#53991,#54109);
#53938=SHAPE_DEFINITION_REPRESENTATION(#53992,#54110);
#53939=SHAPE_DEFINITION_REPRESENTATION(#53993,#54111);
#53940=SHAPE_DEFINITION_REPRESENTATION(#53994,#54112);
#53941=SHAPE_DEFINITION_REPRESENTATION(#54000,#54113);
#53942=SHAPE_DEFINITION_REPRESENTATION(#54040,#54114);
#53943=SHAPE_DEFINITION_REPRESENTATION(#54041,#54115);
#53944=SHAPE_DEFINITION_REPRESENTATION(#54042,#54116);
#53945=SHAPE_DEFINITION_REPRESENTATION(#54043,#54117);
#53946=SHAPE_DEFINITION_REPRESENTATION(#54044,#54118);
#53947=SHAPE_DEFINITION_REPRESENTATION(#54045,#54119);
#53948=SHAPE_DEFINITION_REPRESENTATION(#54046,#54120);
#53949=SHAPE_DEFINITION_REPRESENTATION(#54047,#54121);
#53950=SHAPE_DEFINITION_REPRESENTATION(#54048,#54122);
#53951=SHAPE_DEFINITION_REPRESENTATION(#54049,#54123);
#53952=SHAPE_DEFINITION_REPRESENTATION(#54050,#54124);
#53953=SHAPE_DEFINITION_REPRESENTATION(#54051,#54125);
#53954=SHAPE_DEFINITION_REPRESENTATION(#54052,#54126);
#53955=SHAPE_DEFINITION_REPRESENTATION(#54053,#54127);
#53956=SHAPE_DEFINITION_REPRESENTATION(#54054,#54128);
#53957=SHAPE_DEFINITION_REPRESENTATION(#54055,#54129);
#53958=SHAPE_DEFINITION_REPRESENTATION(#54056,#54130);
#53959=SHAPE_DEFINITION_REPRESENTATION(#54057,#54131);
#53960=SHAPE_DEFINITION_REPRESENTATION(#54058,#54132);
#53961=SHAPE_DEFINITION_REPRESENTATION(#54059,#54133);
#53962=SHAPE_DEFINITION_REPRESENTATION(#54060,#54134);
#53963=PRODUCT_DEFINITION_SHAPE('',$,#54136);
#53964=PRODUCT_DEFINITION_SHAPE('',$,#54137);
#53965=PRODUCT_DEFINITION_SHAPE('',$,#54138);
#53966=PRODUCT_DEFINITION_SHAPE('',$,#54139);
#53967=PRODUCT_DEFINITION_SHAPE('',$,#54140);
#53968=PRODUCT_DEFINITION_SHAPE('',$,#54141);
#53969=PRODUCT_DEFINITION_SHAPE('',$,#54142);
#53970=PRODUCT_DEFINITION_SHAPE('',$,#54143);
#53971=PRODUCT_DEFINITION_SHAPE('',$,#54144);
#53972=PRODUCT_DEFINITION_SHAPE('',$,#54145);
#53973=PRODUCT_DEFINITION_SHAPE('',$,#54146);
#53974=PRODUCT_DEFINITION_SHAPE('',$,#54147);
#53975=PRODUCT_DEFINITION_SHAPE('',$,#54148);
#53976=PRODUCT_DEFINITION_SHAPE('',$,#54149);
#53977=PRODUCT_DEFINITION_SHAPE('',$,#54150);
#53978=PRODUCT_DEFINITION_SHAPE('',$,#54151);
#53979=PRODUCT_DEFINITION_SHAPE('',$,#54152);
#53980=PRODUCT_DEFINITION_SHAPE('',$,#54153);
#53981=PRODUCT_DEFINITION_SHAPE('',$,#54154);
#53982=PRODUCT_DEFINITION_SHAPE('',$,#54155);
#53983=PRODUCT_DEFINITION_SHAPE('',$,#54156);
#53984=PRODUCT_DEFINITION_SHAPE($,$,#593);
#53985=PRODUCT_DEFINITION_SHAPE($,$,#594);
#53986=PRODUCT_DEFINITION_SHAPE($,$,#595);
#53987=PRODUCT_DEFINITION_SHAPE($,$,#596);
#53988=PRODUCT_DEFINITION_SHAPE($,$,#597);
#53989=PRODUCT_DEFINITION_SHAPE('',$,#54157);
#53990=PRODUCT_DEFINITION_SHAPE('',$,#54158);
#53991=PRODUCT_DEFINITION_SHAPE('',$,#54159);
#53992=PRODUCT_DEFINITION_SHAPE('',$,#54160);
#53993=PRODUCT_DEFINITION_SHAPE('',$,#54161);
#53994=PRODUCT_DEFINITION_SHAPE('',$,#54162);
#53995=PRODUCT_DEFINITION_SHAPE($,$,#598);
#53996=PRODUCT_DEFINITION_SHAPE($,$,#599);
#53997=PRODUCT_DEFINITION_SHAPE($,$,#600);
#53998=PRODUCT_DEFINITION_SHAPE($,$,#601);
#53999=PRODUCT_DEFINITION_SHAPE($,$,#602);
#54000=PRODUCT_DEFINITION_SHAPE('',$,#54163);
#54001=PRODUCT_DEFINITION_SHAPE($,$,#603);
#54002=PRODUCT_DEFINITION_SHAPE($,$,#604);
#54003=PRODUCT_DEFINITION_SHAPE($,$,#605);
#54004=PRODUCT_DEFINITION_SHAPE($,$,#606);
#54005=PRODUCT_DEFINITION_SHAPE($,$,#607);
#54006=PRODUCT_DEFINITION_SHAPE($,$,#608);
#54007=PRODUCT_DEFINITION_SHAPE($,$,#609);
#54008=PRODUCT_DEFINITION_SHAPE($,$,#610);
#54009=PRODUCT_DEFINITION_SHAPE($,$,#611);
#54010=PRODUCT_DEFINITION_SHAPE($,$,#612);
#54011=PRODUCT_DEFINITION_SHAPE($,$,#613);
#54012=PRODUCT_DEFINITION_SHAPE($,$,#614);
#54013=PRODUCT_DEFINITION_SHAPE($,$,#615);
#54014=PRODUCT_DEFINITION_SHAPE($,$,#616);
#54015=PRODUCT_DEFINITION_SHAPE($,$,#617);
#54016=PRODUCT_DEFINITION_SHAPE($,$,#618);
#54017=PRODUCT_DEFINITION_SHAPE($,$,#619);
#54018=PRODUCT_DEFINITION_SHAPE($,$,#620);
#54019=PRODUCT_DEFINITION_SHAPE($,$,#621);
#54020=PRODUCT_DEFINITION_SHAPE($,$,#622);
#54021=PRODUCT_DEFINITION_SHAPE($,$,#623);
#54022=PRODUCT_DEFINITION_SHAPE($,$,#624);
#54023=PRODUCT_DEFINITION_SHAPE($,$,#625);
#54024=PRODUCT_DEFINITION_SHAPE($,$,#626);
#54025=PRODUCT_DEFINITION_SHAPE($,$,#627);
#54026=PRODUCT_DEFINITION_SHAPE($,$,#628);
#54027=PRODUCT_DEFINITION_SHAPE($,$,#629);
#54028=PRODUCT_DEFINITION_SHAPE($,$,#630);
#54029=PRODUCT_DEFINITION_SHAPE($,$,#631);
#54030=PRODUCT_DEFINITION_SHAPE($,$,#632);
#54031=PRODUCT_DEFINITION_SHAPE($,$,#633);
#54032=PRODUCT_DEFINITION_SHAPE($,$,#634);
#54033=PRODUCT_DEFINITION_SHAPE($,$,#635);
#54034=PRODUCT_DEFINITION_SHAPE($,$,#636);
#54035=PRODUCT_DEFINITION_SHAPE($,$,#637);
#54036=PRODUCT_DEFINITION_SHAPE($,$,#638);
#54037=PRODUCT_DEFINITION_SHAPE($,$,#639);
#54038=PRODUCT_DEFINITION_SHAPE($,$,#640);
#54039=PRODUCT_DEFINITION_SHAPE($,$,#641);
#54040=PRODUCT_DEFINITION_SHAPE('',$,#54164);
#54041=PRODUCT_DEFINITION_SHAPE('',$,#54165);
#54042=PRODUCT_DEFINITION_SHAPE('',$,#54166);
#54043=PRODUCT_DEFINITION_SHAPE('',$,#54167);
#54044=PRODUCT_DEFINITION_SHAPE('',$,#54168);
#54045=PRODUCT_DEFINITION_SHAPE('',$,#54169);
#54046=PRODUCT_DEFINITION_SHAPE('',$,#54170);
#54047=PRODUCT_DEFINITION_SHAPE('',$,#54171);
#54048=PRODUCT_DEFINITION_SHAPE('',$,#54172);
#54049=PRODUCT_DEFINITION_SHAPE('',$,#54173);
#54050=PRODUCT_DEFINITION_SHAPE('',$,#54174);
#54051=PRODUCT_DEFINITION_SHAPE('',$,#54175);
#54052=PRODUCT_DEFINITION_SHAPE('',$,#54176);
#54053=PRODUCT_DEFINITION_SHAPE('',$,#54177);
#54054=PRODUCT_DEFINITION_SHAPE('',$,#54178);
#54055=PRODUCT_DEFINITION_SHAPE('',$,#54179);
#54056=PRODUCT_DEFINITION_SHAPE('',$,#54180);
#54057=PRODUCT_DEFINITION_SHAPE('',$,#54181);
#54058=PRODUCT_DEFINITION_SHAPE('',$,#54182);
#54059=PRODUCT_DEFINITION_SHAPE('',$,#54183);
#54060=PRODUCT_DEFINITION_SHAPE('',$,#54184);
#54061=PRODUCT_DEFINITION_SHAPE($,$,#642);
#54062=PRODUCT_DEFINITION_SHAPE($,$,#643);
#54063=PRODUCT_DEFINITION_SHAPE($,$,#644);
#54064=PRODUCT_DEFINITION_SHAPE($,$,#645);
#54065=PRODUCT_DEFINITION_SHAPE($,$,#646);
#54066=PRODUCT_DEFINITION_SHAPE($,$,#647);
#54067=PRODUCT_DEFINITION_SHAPE($,$,#648);
#54068=PRODUCT_DEFINITION_SHAPE($,$,#649);
#54069=PRODUCT_DEFINITION_SHAPE($,$,#650);
#54070=PRODUCT_DEFINITION_SHAPE($,$,#651);
#54071=PRODUCT_DEFINITION_SHAPE($,$,#652);
#54072=PRODUCT_DEFINITION_SHAPE($,$,#653);
#54073=PRODUCT_DEFINITION_SHAPE($,$,#654);
#54074=PRODUCT_DEFINITION_SHAPE($,$,#655);
#54075=PRODUCT_DEFINITION_SHAPE($,$,#656);
#54076=PRODUCT_DEFINITION_SHAPE($,$,#657);
#54077=PRODUCT_DEFINITION_SHAPE($,$,#658);
#54078=PRODUCT_DEFINITION_SHAPE($,$,#659);
#54079=PRODUCT_DEFINITION_SHAPE($,$,#660);
#54080=PRODUCT_DEFINITION_SHAPE($,$,#661);
#54081=PRODUCT_DEFINITION_SHAPE($,$,#662);
#54082=PRODUCT_DEFINITION_SHAPE($,$,#663);
#54083=PRODUCT_DEFINITION_SHAPE($,$,#664);
#54084=PRODUCT_DEFINITION_SHAPE($,$,#665);
#54085=PRODUCT_DEFINITION_SHAPE($,$,#666);
#54086=SHAPE_REPRESENTATION('',(#11806,#12979,#12980,#12981),#53860);
#54087=SHAPE_REPRESENTATION('',(#11807,#12441,#12442,#12443,#12444,#12445,
#12446,#12447,#12448,#12449,#12450,#12451,#12452,#12453,#12454,#12455,#12456,
#12457,#12458,#12459,#12460,#12461,#12462,#12463,#12464,#12465,#12466,#12467,
#12468,#12469,#12470,#12471,#12472,#12473,#12474,#12475,#12476,#12477,#12478,
#12479),#53861);
#54088=SHAPE_REPRESENTATION('',(#11808),#53862);
#54089=SHAPE_REPRESENTATION('',(#11827),#53863);
#54090=SHAPE_REPRESENTATION('',(#11902),#53864);
#54091=SHAPE_REPRESENTATION('',(#11977),#53865);
#54092=SHAPE_REPRESENTATION('',(#11986),#53866);
#54093=SHAPE_REPRESENTATION('',(#11995),#53867);
#54094=SHAPE_REPRESENTATION('',(#12004),#53868);
#54095=SHAPE_REPRESENTATION('',(#12013),#53869);
#54096=SHAPE_REPRESENTATION('',(#12035),#53870);
#54097=SHAPE_REPRESENTATION('',(#12057),#53871);
#54098=SHAPE_REPRESENTATION('',(#12079),#53872);
#54099=SHAPE_REPRESENTATION('',(#12101),#53873);
#54100=SHAPE_REPRESENTATION('',(#12127),#53874);
#54101=SHAPE_REPRESENTATION('',(#12153,#12276,#12277,#12278,#12279,#12280),
#53875);
#54102=SHAPE_REPRESENTATION('',(#12154),#53876);
#54103=SHAPE_REPRESENTATION('',(#12174),#53877);
#54104=SHAPE_REPRESENTATION('',(#12194),#53878);
#54105=SHAPE_REPRESENTATION('',(#12209),#53879);
#54106=SHAPE_REPRESENTATION('',(#12259),#53880);
#54107=SHAPE_REPRESENTATION('',(#12281,#12410,#12411,#12412,#12413,#12414),
#53881);
#54108=SHAPE_REPRESENTATION('',(#12282),#53882);
#54109=SHAPE_REPRESENTATION('',(#12302),#53883);
#54110=SHAPE_REPRESENTATION('',(#12322),#53884);
#54111=SHAPE_REPRESENTATION('',(#12339),#53885);
#54112=SHAPE_REPRESENTATION('',(#12393),#53886);
#54113=SHAPE_REPRESENTATION('',(#12415),#53887);
#54114=SHAPE_REPRESENTATION('',(#12480,#12957,#12958,#12959,#12960,#12961,
#12962,#12963,#12964,#12965,#12966,#12967),#53888);
#54115=SHAPE_REPRESENTATION('',(#12481),#53889);
#54116=SHAPE_REPRESENTATION('',(#12494),#53890);
#54117=SHAPE_REPRESENTATION('',(#12503),#53891);
#54118=SHAPE_REPRESENTATION('',(#12512),#53892);
#54119=SHAPE_REPRESENTATION('',(#12527),#53893);
#54120=SHAPE_REPRESENTATION('',(#12536),#53894);
#54121=SHAPE_REPRESENTATION('',(#12551),#53895);
#54122=SHAPE_REPRESENTATION('',(#12560),#53896);
#54123=SHAPE_REPRESENTATION('',(#12653),#53897);
#54124=SHAPE_REPRESENTATION('',(#12676,#12968,#12969,#12970,#12971,#12972,
#12973,#12974,#12975,#12976,#12977,#12978),#53898);
#54125=SHAPE_REPRESENTATION('',(#12677),#53899);
#54126=SHAPE_REPRESENTATION('',(#12690),#53900);
#54127=SHAPE_REPRESENTATION('',(#12699),#53901);
#54128=SHAPE_REPRESENTATION('',(#12708),#53902);
#54129=SHAPE_REPRESENTATION('',(#12723),#53903);
#54130=SHAPE_REPRESENTATION('',(#12732),#53904);
#54131=SHAPE_REPRESENTATION('',(#12747),#53905);
#54132=SHAPE_REPRESENTATION('',(#12756),#53906);
#54133=SHAPE_REPRESENTATION('',(#12929),#53907);
#54134=SHAPE_REPRESENTATION('',(#12940),#53908);
#54135=PRODUCT_DEFINITION_CONTEXT('part definition',#54284,'design');
#54136=PRODUCT_DEFINITION(
'PAT-101','PAT-101',#54185,#54135);
#54137=PRODUCT_DEFINITION('Bearing frame','Bearing frame',#54186,#54135);
#54138=PRODUCT_DEFINITION('Base','Base',#54187,#54135);
#54139=PRODUCT_DEFINITION('Front plate','Front plate',#54188,#54135);
#54140=PRODUCT_DEFINITION('Rear plate','Rear plate',#54189,#54135);
#54141=PRODUCT_DEFINITION('Frame spacer','Frame spacer',#54190,#54135);
#54142=PRODUCT_DEFINITION('Frame spacer (1)','Frame spacer (1)',#54191,#54135);
#54143=PRODUCT_DEFINITION('Frame spacer (2)','Frame spacer (2)',#54192,#54135);
#54144=PRODUCT_DEFINITION('Frame spacer (3)','Frame spacer (3)',#54193,#54135);
#54145=PRODUCT_DEFINITION('Small bearing cap','Small bearing cap',#54194,
#54135);
#54146=PRODUCT_DEFINITION('Large bearing cap','Large bearing cap',#54195,
#54135);
#54147=PRODUCT_DEFINITION('Small bearing cap (1)','Small bearing cap (1)',
#54196,#54135);
#54148=PRODUCT_DEFINITION('Large bearing cap (1)','Large bearing cap (1)',
#54197,#54135);
#54149=PRODUCT_DEFINITION('Cap Screw - M5x20','Cap Screw - M5x20',#54198,
#54135);
#54150=PRODUCT_DEFINITION('Cap Screw - M6x25','Cap Screw - M6x25',#54199,
#54135);
#54151=PRODUCT_DEFINITION('Sealed Ball Bearing - 12 x 32 x 10 mm',
'Sealed Ball Bearing - 12 x 32 x 10 mm',#54200,#54135);
#54152=PRODUCT_DEFINITION('Inner ring','Inner ring',#54201,#54135);
#54153=PRODUCT_DEFINITION('Outer ring','Outer ring',#54202,#54135);
#54154=PRODUCT_DEFINITION('Balls','Balls',#54203,#54135);
#54155=PRODUCT_DEFINITION('Cage','Cage',#54204,#54135);
#54156=PRODUCT_DEFINITION('Seals 2RS','Seals 2RS',#54205,#54135);
#54157=PRODUCT_DEFINITION('Sealed Ball Bearing - 20 x 47 x 14 mm',
'Sealed Ball Bearing - 20 x 47 x 14 mm',#54206,#54135);
#54158=PRODUCT_DEFINITION('Inner ring (1)','Inner ring (1)',#54207,#54135);
#54159=PRODUCT_DEFINITION('Outer ring (1)','Outer ring (1)',#54208,#54135);
#54160=PRODUCT_DEFINITION('Balls (1)','Balls (1)',#54209,#54135);
#54161=PRODUCT_DEFINITION('Cage (1)','Cage (1)',#54210,#54135);
#54162=PRODUCT_DEFINITION('Seals 2RS (1)','Seals 2RS (1)',#54211,#54135);
#54163=PRODUCT_DEFINITION('Cap Screw - M4x16','Cap Screw - M4x16',#54212,
#54135);
#54164=PRODUCT_DEFINITION('Input rotor','Input rotor',#54213,#54135);
#54165=PRODUCT_DEFINITION('Input shaft','Input shaft',#54214,#54135);
#54166=PRODUCT_DEFINITION('Input front sleeve','Input front sleeve',#54215,
#54135);
#54167=PRODUCT_DEFINITION('Input rear sleeve','Input rear sleeve',#54216,
#54135);
#54168=PRODUCT_DEFINITION('Input retaining collar',
'Input retaining collar',#54217,#54135);
#54169=PRODUCT_DEFINITION('Input outer race sleeve',
'Input outer race sleeve',#54218,#54135);
#54170=PRODUCT_DEFINITION('Input retaining collar (1)',
'Input retaining collar (1)',#54219,#54135);
#54171=PRODUCT_DEFINITION('Input outer race sleeve (1)',
'Input outer race sleeve (1)',#54220,#54135);
#54172=PRODUCT_DEFINITION('Spur Gear - Module 2, 20 Teeth, 12 mm Bore',
'Spur Gear - Module 2, 20 Teeth, 12 mm Bore',#54221,#54135);
#54173=PRODUCT_DEFINITION('Parallel Key - 4x4x25',
'Parallel Key - 4x4x25',#54222,#54135);
#54174=PRODUCT_DEFINITION('Output rotor','Output rotor',#54223,#54135);
#54175=PRODUCT_DEFINITION('Output shaft','Output shaft',#54224,#54135);
#54176=PRODUCT_DEFINITION('Output front sleeve','Output front sleeve',#54225,
#54135);
#54177=PRODUCT_DEFINITION('Output rear sleeve','Output rear sleeve',#54226,
#54135);
#54178=PRODUCT_DEFINITION('Output retaining collar',
'Output retaining collar',#54227,#54135);
#54179=PRODUCT_DEFINITION('Output outer race sleeve',
'Output outer race sleeve',#54228,#54135);
#54180=PRODUCT_DEFINITION('Output retaining collar (1)',
'Output retaining collar (1)',#54229,#54135);
#54181=PRODUCT_DEFINITION('Output outer race sleeve (1)',
'Output outer race sleeve (1)',#54230,#54135);
#54182=PRODUCT_DEFINITION('Spur Gear - Module 2, 40 Teeth, 20 mm Bore',
'Spur Gear - Module 2, 40 Teeth, 20 mm Bore',#54231,#54135);
#54183=PRODUCT_DEFINITION('Parallel key 6x6x28','Parallel key 6x6x28',#54232,
#54135);
#54184=PRODUCT_DEFINITION('Socket Set Screw - M5x8',
'Socket Set Screw - M5x8',#54233,#54135);
#54185=PRODUCT_DEFINITION_FORMATION('',$,#54286);
#54186=PRODUCT_DEFINITION_FORMATION('',$,#54287);
#54187=PRODUCT_DEFINITION_FORMATION('',$,#54288);
#54188=PRODUCT_DEFINITION_FORMATION('',$,#54289);
#54189=PRODUCT_DEFINITION_FORMATION('',$,#54290);
#54190=PRODUCT_DEFINITION_FORMATION('',$,#54291);
#54191=PRODUCT_DEFINITION_FORMATION('',$,#54292);
#54192=PRODUCT_DEFINITION_FORMATION('',$,#54293);
#54193=PRODUCT_DEFINITION_FORMATION('',$,#54294);
#54194=PRODUCT_DEFINITION_FORMATION('',$,#54295);
#54195=PRODUCT_DEFINITION_FORMATION('',$,#54296);
#54196=PRODUCT_DEFINITION_FORMATION('',$,#54297);
#54197=PRODUCT_DEFINITION_FORMATION('',$,#54298);
#54198=PRODUCT_DEFINITION_FORMATION('',$,#54299);
#54199=PRODUCT_DEFINITION_FORMATION('',$,#54300);
#54200=PRODUCT_DEFINITION_FORMATION('',$,#54301);
#54201=PRODUCT_DEFINITION_FORMATION('',$,#54302);
#54202=PRODUCT_DEFINITION_FORMATION('',$,#54303);
#54203=PRODUCT_DEFINITION_FORMATION('',$,#54304);
#54204=PRODUCT_DEFINITION_FORMATION('',$,#54305);
#54205=PRODUCT_DEFINITION_FORMATION('',$,#54306);
#54206=PRODUCT_DEFINITION_FORMATION('',$,#54307);
#54207=PRODUCT_DEFINITION_FORMATION('',$,#54308);
#54208=PRODUCT_DEFINITION_FORMATION('',$,#54309);
#54209=PRODUCT_DEFINITION_FORMATION('',$,#54310);
#54210=PRODUCT_DEFINITION_FORMATION('',$,#54311);
#54211=PRODUCT_DEFINITION_FORMATION('',$,#54312);
#54212=PRODUCT_DEFINITION_FORMATION('',$,#54313);
#54213=PRODUCT_DEFINITION_FORMATION('',$,#54314);
#54214=PRODUCT_DEFINITION_FORMATION('',$,#54315);
#54215=PRODUCT_DEFINITION_FORMATION('',$,#54316);
#54216=PRODUCT_DEFINITION_FORMATION('',$,#54317);
#54217=PRODUCT_DEFINITION_FORMATION('',$,#54318);
#54218=PRODUCT_DEFINITION_FORMATION('',$,#54319);
#54219=PRODUCT_DEFINITION_FORMATION('',$,#54320);
#54220=PRODUCT_DEFINITION_FORMATION('',$,#54321);
#54221=PRODUCT_DEFINITION_FORMATION('',$,#54322);
#54222=PRODUCT_DEFINITION_FORMATION('',$,#54323);
#54223=PRODUCT_DEFINITION_FORMATION('',$,#54324);
#54224=PRODUCT_DEFINITION_FORMATION('',$,#54325);
#54225=PRODUCT_DEFINITION_FORMATION('',$,#54326);
#54226=PRODUCT_DEFINITION_FORMATION('',$,#54327);
#54227=PRODUCT_DEFINITION_FORMATION('',$,#54328);
#54228=PRODUCT_DEFINITION_FORMATION('',$,#54329);
#54229=PRODUCT_DEFINITION_FORMATION('',$,#54330);
#54230=PRODUCT_DEFINITION_FORMATION('',$,#54331);
#54231=PRODUCT_DEFINITION_FORMATION('',$,#54332);
#54232=PRODUCT_DEFINITION_FORMATION('',$,#54333);
#54233=PRODUCT_DEFINITION_FORMATION('',$,#54334);
#54234=PRODUCT_RELATED_PRODUCT_CATEGORY('PAT-101','PAT-101',(#54286));
#54235=PRODUCT_RELATED_PRODUCT_CATEGORY('Bearing frame','Bearing frame',
(#54287));
#54236=PRODUCT_RELATED_PRODUCT_CATEGORY('Base','Base',(#54288));
#54237=PRODUCT_RELATED_PRODUCT_CATEGORY('Front plate','Front plate',(#54289));
#54238=PRODUCT_RELATED_PRODUCT_CATEGORY('Rear plate','Rear plate',(#54290));
#54239=PRODUCT_RELATED_PRODUCT_CATEGORY('Frame spacer','Frame spacer',(#54291));
#54240=PRODUCT_RELATED_PRODUCT_CATEGORY('Frame spacer (1)',
'Frame spacer (1)',(#54292));
#54241=PRODUCT_RELATED_PRODUCT_CATEGORY('Frame spacer (2)',
'Frame spacer (2)',(#54293));
#54242=PRODUCT_RELATED_PRODUCT_CATEGORY('Frame spacer (3)',
'Frame spacer (3)',(#54294));
#54243=PRODUCT_RELATED_PRODUCT_CATEGORY('Small bearing cap',
'Small bearing cap',(#54295));
#54244=PRODUCT_RELATED_PRODUCT_CATEGORY('Large bearing cap',
'Large bearing cap',(#54296));
#54245=PRODUCT_RELATED_PRODUCT_CATEGORY('Small bearing cap (1)',
'Small bearing cap (1)',(#54297));
#54246=PRODUCT_RELATED_PRODUCT_CATEGORY('Large bearing cap (1)',
'Large bearing cap (1)',(#54298));
#54247=PRODUCT_RELATED_PRODUCT_CATEGORY('Cap Screw - M5x20',
'Cap Screw - M5x20',(#54299));
#54248=PRODUCT_RELATED_PRODUCT_CATEGORY('Cap Screw - M6x25',
'Cap Screw - M6x25',(#54300));
#54249=PRODUCT_RELATED_PRODUCT_CATEGORY(
'Sealed Ball Bearing - 12 x 32 x 10 mm',
'Sealed Ball Bearing - 12 x 32 x 10 mm',(#54301));
#54250=PRODUCT_RELATED_PRODUCT_CATEGORY('Inner ring','Inner ring',(#54302));
#54251=PRODUCT_RELATED_PRODUCT_CATEGORY('Outer ring','Outer ring',(#54303));
#54252=PRODUCT_RELATED_PRODUCT_CATEGORY('Balls','Balls',(#54304));
#54253=PRODUCT_RELATED_PRODUCT_CATEGORY('Cage','Cage',(#54305));
#54254=PRODUCT_RELATED_PRODUCT_CATEGORY('Seals 2RS','Seals 2RS',(#54306));
#54255=PRODUCT_RELATED_PRODUCT_CATEGORY(
'Sealed Ball Bearing - 20 x 47 x 14 mm',
'Sealed Ball Bearing - 20 x 47 x 14 mm',(#54307));
#54256=PRODUCT_RELATED_PRODUCT_CATEGORY('Inner ring (1)',
'Inner ring (1)',(#54308));
#54257=PRODUCT_RELATED_PRODUCT_CATEGORY('Outer ring (1)',
'Outer ring (1)',(#54309));
#54258=PRODUCT_RELATED_PRODUCT_CATEGORY('Balls (1)','Balls (1)',(#54310));
#54259=PRODUCT_RELATED_PRODUCT_CATEGORY('Cage (1)','Cage (1)',(#54311));
#54260=PRODUCT_RELATED_PRODUCT_CATEGORY('Seals 2RS (1)','Seals 2RS (1)',
(#54312));
#54261=PRODUCT_RELATED_PRODUCT_CATEGORY('Cap Screw - M4x16',
'Cap Screw - M4x16',(#54313));
#54262=PRODUCT_RELATED_PRODUCT_CATEGORY('Input rotor','Input rotor',(#54314));
#54263=PRODUCT_RELATED_PRODUCT_CATEGORY('Input shaft','Input shaft',(#54315));
#54264=PRODUCT_RELATED_PRODUCT_CATEGORY('Input front sleeve',
'Input front sleeve',(#54316));
#54265=PRODUCT_RELATED_PRODUCT_CATEGORY('Input rear sleeve',
'Input rear sleeve',(#54317));
#54266=PRODUCT_RELATED_PRODUCT_CATEGORY('Input retaining collar',
'Input retaining collar',(#54318));
#54267=PRODUCT_RELATED_PRODUCT_CATEGORY('Input outer race sleeve',
'Input outer race sleeve',(#54319));
#54268=PRODUCT_RELATED_PRODUCT_CATEGORY('Input retaining collar (1)',
'Input retaining collar (1)',(#54320));
#54269=PRODUCT_RELATED_PRODUCT_CATEGORY('Input outer race sleeve (1)',
'Input outer race sleeve (1)',(#54321));
#54270=PRODUCT_RELATED_PRODUCT_CATEGORY(
'Spur Gear - Module 2, 20 Teeth, 12 mm Bore',
'Spur Gear - Module 2, 20 Teeth, 12 mm Bore',(#54322));
#54271=PRODUCT_RELATED_PRODUCT_CATEGORY('Parallel Key - 4x4x25',
'Parallel Key - 4x4x25',(#54323));
#54272=PRODUCT_RELATED_PRODUCT_CATEGORY('Output rotor','Output rotor',(#54324));
#54273=PRODUCT_RELATED_PRODUCT_CATEGORY('Output shaft','Output shaft',(#54325));
#54274=PRODUCT_RELATED_PRODUCT_CATEGORY('Output front sleeve',
'Output front sleeve',(#54326));
#54275=PRODUCT_RELATED_PRODUCT_CATEGORY('Output rear sleeve',
'Output rear sleeve',(#54327));
#54276=PRODUCT_RELATED_PRODUCT_CATEGORY('Output retaining collar',
'Output retaining collar',(#54328));
#54277=PRODUCT_RELATED_PRODUCT_CATEGORY('Output outer race sleeve',
'Output outer race sleeve',(#54329));
#54278=PRODUCT_RELATED_PRODUCT_CATEGORY('Output retaining collar (1)',
'Output retaining collar (1)',(#54330));
#54279=PRODUCT_RELATED_PRODUCT_CATEGORY('Output outer race sleeve (1)',
'Output outer race sleeve (1)',(#54331));
#54280=PRODUCT_RELATED_PRODUCT_CATEGORY(
'Spur Gear - Module 2, 40 Teeth, 20 mm Bore',
'Spur Gear - Module 2, 40 Teeth, 20 mm Bore',(#54332));
#54281=PRODUCT_RELATED_PRODUCT_CATEGORY('Parallel key 6x6x28',
'Parallel key 6x6x28',(#54333));
#54282=PRODUCT_RELATED_PRODUCT_CATEGORY('Socket Set Screw - M5x8',
'Socket Set Screw - M5x8',(#54334));
#54283=APPLICATION_PROTOCOL_DEFINITION('international standard',
'automotive_design',2009,#54284);
#54284=APPLICATION_CONTEXT(
'Core Data for Automotive Mechanical Design Process');
#54285=PRODUCT_CONTEXT('part definition',#54284,'mechanical');
#54286=PRODUCT('PAT-101',
'PAT-101','PAT-101',(#54285));
#54287=PRODUCT('Bearing frame','Bearing frame','Bearing frame',(#54285));
#54288=PRODUCT('Base','Base','Base',(#54285));
#54289=PRODUCT('Front plate','Front plate','Front plate',(#54285));
#54290=PRODUCT('Rear plate','Rear plate','Rear plate',(#54285));
#54291=PRODUCT('Frame spacer','Frame spacer','Frame spacer',(#54285));
#54292=PRODUCT('Frame spacer (1)','Frame spacer (1)','Frame spacer (1)',(#54285));
#54293=PRODUCT('Frame spacer (2)','Frame spacer (2)','Frame spacer (2)',(#54285));
#54294=PRODUCT('Frame spacer (3)','Frame spacer (3)','Frame spacer (3)',(#54285));
#54295=PRODUCT('Small bearing cap','Small bearing cap',
'Small bearing cap',(#54285));
#54296=PRODUCT('Large bearing cap','Large bearing cap',
'Large bearing cap',(#54285));
#54297=PRODUCT('Small bearing cap (1)','Small bearing cap (1)',
'Small bearing cap (1)',(#54285));
#54298=PRODUCT('Large bearing cap (1)','Large bearing cap (1)',
'Large bearing cap (1)',(#54285));
#54299=PRODUCT('Cap Screw - M5x20','Cap Screw - M5x20',
'Cap Screw - M5x20',(#54285));
#54300=PRODUCT('Cap Screw - M6x25','Cap Screw - M6x25',
'Cap Screw - M6x25',(#54285));
#54301=PRODUCT('Sealed Ball Bearing - 12 x 32 x 10 mm',
'Sealed Ball Bearing - 12 x 32 x 10 mm',
'Sealed Ball Bearing - 12 x 32 x 10 mm',(#54285));
#54302=PRODUCT('Inner ring','Inner ring','Inner ring',(#54285));
#54303=PRODUCT('Outer ring','Outer ring','Outer ring',(#54285));
#54304=PRODUCT('Balls','Balls','Balls',(#54285));
#54305=PRODUCT('Cage','Cage','Cage',(#54285));
#54306=PRODUCT('Seals 2RS','Seals 2RS','Seals 2RS',(#54285));
#54307=PRODUCT('Sealed Ball Bearing - 20 x 47 x 14 mm',
'Sealed Ball Bearing - 20 x 47 x 14 mm',
'Sealed Ball Bearing - 20 x 47 x 14 mm',(#54285));
#54308=PRODUCT('Inner ring (1)','Inner ring (1)','Inner ring (1)',(#54285));
#54309=PRODUCT('Outer ring (1)','Outer ring (1)','Outer ring (1)',(#54285));
#54310=PRODUCT('Balls (1)','Balls (1)','Balls (1)',(#54285));
#54311=PRODUCT('Cage (1)','Cage (1)','Cage (1)',(#54285));
#54312=PRODUCT('Seals 2RS (1)','Seals 2RS (1)','Seals 2RS (1)',(#54285));
#54313=PRODUCT('Cap Screw - M4x16','Cap Screw - M4x16',
'Cap Screw - M4x16',(#54285));
#54314=PRODUCT('Input rotor','Input rotor','Input rotor',(#54285));
#54315=PRODUCT('Input shaft','Input shaft','Input shaft',(#54285));
#54316=PRODUCT('Input front sleeve','Input front sleeve',
'Input front sleeve',(#54285));
#54317=PRODUCT('Input rear sleeve','Input rear sleeve',
'Input rear sleeve',(#54285));
#54318=PRODUCT('Input retaining collar','Input retaining collar',
'Input retaining collar',(#54285));
#54319=PRODUCT('Input outer race sleeve','Input outer race sleeve',
'Input outer race sleeve',(#54285));
#54320=PRODUCT('Input retaining collar (1)','Input retaining collar (1)',
'Input retaining collar (1)',(#54285));
#54321=PRODUCT('Input outer race sleeve (1)',
'Input outer race sleeve (1)','Input outer race sleeve (1)',(#54285));
#54322=PRODUCT('Spur Gear - Module 2, 20 Teeth, 12 mm Bore',
'Spur Gear - Module 2, 20 Teeth, 12 mm Bore',
'Spur Gear - Module 2, 20 Teeth, 12 mm Bore',(#54285));
#54323=PRODUCT('Parallel Key - 4x4x25','Parallel Key - 4x4x25',
'Parallel Key - 4x4x25',(#54285));
#54324=PRODUCT('Output rotor','Output rotor','Output rotor',(#54285));
#54325=PRODUCT('Output shaft','Output shaft','Output shaft',(#54285));
#54326=PRODUCT('Output front sleeve','Output front sleeve',
'Output front sleeve',(#54285));
#54327=PRODUCT('Output rear sleeve','Output rear sleeve',
'Output rear sleeve',(#54285));
#54328=PRODUCT('Output retaining collar','Output retaining collar',
'Output retaining collar',(#54285));
#54329=PRODUCT('Output outer race sleeve','Output outer race sleeve',
'Output outer race sleeve',(#54285));
#54330=PRODUCT('Output retaining collar (1)',
'Output retaining collar (1)','Output retaining collar (1)',(#54285));
#54331=PRODUCT('Output outer race sleeve (1)',
'Output outer race sleeve (1)','Output outer race sleeve (1)',(#54285));
#54332=PRODUCT('Spur Gear - Module 2, 40 Teeth, 20 mm Bore',
'Spur Gear - Module 2, 40 Teeth, 20 mm Bore',
'Spur Gear - Module 2, 40 Teeth, 20 mm Bore',(#54285));
#54333=PRODUCT('Parallel key 6x6x28','Parallel key 6x6x28',
'Parallel key 6x6x28',(#54285));
#54334=PRODUCT('Socket Set Screw - M5x8','Socket Set Screw - M5x8',
'Socket Set Screw - M5x8',(#54285));
#54335=PRESENTATION_STYLE_ASSIGNMENT((#54340));
#54336=PRESENTATION_STYLE_ASSIGNMENT((#54341));
#54337=PRESENTATION_STYLE_ASSIGNMENT((#54342));
#54338=PRESENTATION_STYLE_ASSIGNMENT((#54343));
#54339=PRESENTATION_STYLE_ASSIGNMENT((#54344));
#54340=SURFACE_STYLE_USAGE(.BOTH.,#54345);
#54341=SURFACE_STYLE_USAGE(.BOTH.,#54346);
#54342=SURFACE_STYLE_USAGE(.BOTH.,#54347);
#54343=SURFACE_STYLE_USAGE(.BOTH.,#54348);
#54344=SURFACE_STYLE_USAGE(.BOTH.,#54349);
#54345=SURFACE_SIDE_STYLE('',(#54350));
#54346=SURFACE_SIDE_STYLE('',(#54351));
#54347=SURFACE_SIDE_STYLE('',(#54352));
#54348=SURFACE_SIDE_STYLE('',(#54353));
#54349=SURFACE_SIDE_STYLE('',(#54354));
#54350=SURFACE_STYLE_FILL_AREA(#54355);
#54351=SURFACE_STYLE_FILL_AREA(#54356);
#54352=SURFACE_STYLE_FILL_AREA(#54357);
#54353=SURFACE_STYLE_FILL_AREA(#54358);
#54354=SURFACE_STYLE_FILL_AREA(#54359);
#54355=FILL_AREA_STYLE('Steel - Satin',(#54360));
#54356=FILL_AREA_STYLE('CAD Library Painted - Deep blue',(#54361));
#54357=FILL_AREA_STYLE('CAD Library Painted - Engineering blue',(#54362));
#54358=FILL_AREA_STYLE('CAD Library Painted - Steel gray',(#54363));
#54359=FILL_AREA_STYLE('CAD Library Painted - Graphite',(#54364));
#54360=FILL_AREA_STYLE_COLOUR('Steel - Satin',#54365);
#54361=FILL_AREA_STYLE_COLOUR('CAD Library Painted - Deep blue',#54366);
#54362=FILL_AREA_STYLE_COLOUR('CAD Library Painted - Engineering blue',
#54367);
#54363=FILL_AREA_STYLE_COLOUR('CAD Library Painted - Steel gray',#54368);
#54364=FILL_AREA_STYLE_COLOUR('CAD Library Painted - Graphite',#54369);
#54365=COLOUR_RGB('Steel - Satin',0.627450980392157,0.627450980392157,0.627450980392157);
#54366=COLOUR_RGB('CAD Library Painted - Deep blue',0.0784313725490196,
0.203921568627451,0.349019607843137);
#54367=COLOUR_RGB('CAD Library Painted - Engineering blue',0.12156862745098,
0.356862745098039,0.6);
#54368=COLOUR_RGB('CAD Library Painted - Steel gray',0.592156862745098,
0.631372549019608,0.67843137254902);
#54369=COLOUR_RGB('CAD Library Painted - Graphite',0.168627450980392,0.192156862745098,
0.231372549019608);
#54370=COLOUR_RGB('Dark Blue',0.08,0.2,0.34);
#54371=FILL_AREA_STYLE_COLOUR('',#54370);
#54372=FILL_AREA_STYLE('',(#54371));
#54373=SURFACE_STYLE_FILL_AREA(#54372);
#54374=SURFACE_SIDE_STYLE('',(#54373));
#54375=SURFACE_STYLE_USAGE(.BOTH.,#54374);
#54376=PRESENTATION_STYLE_ASSIGNMENT((#54375));
#54377=COLOUR_RGB('Light Blue',0.38,0.62,0.78);
#54378=FILL_AREA_STYLE_COLOUR('',#54377);
#54379=FILL_AREA_STYLE('',(#54378));
#54380=SURFACE_STYLE_FILL_AREA(#54379);
#54381=SURFACE_SIDE_STYLE('',(#54380));
#54382=SURFACE_STYLE_USAGE(.BOTH.,#54381);
#54383=PRESENTATION_STYLE_ASSIGNMENT((#54382));
#54384=COLOUR_RGB('Sky Blue',0.24,0.69,0.87);
#54385=FILL_AREA_STYLE_COLOUR('',#54384);
#54386=FILL_AREA_STYLE('',(#54385));
#54387=SURFACE_STYLE_FILL_AREA(#54386);
#54388=SURFACE_SIDE_STYLE('',(#54387));
#54389=SURFACE_STYLE_USAGE(.BOTH.,#54388);
#54390=PRESENTATION_STYLE_ASSIGNMENT((#54389));
#54391=COLOUR_RGB('Grey',0.48,0.52,0.57);
#54392=FILL_AREA_STYLE_COLOUR('',#54391);
#54393=FILL_AREA_STYLE('',(#54392));
#54394=SURFACE_STYLE_FILL_AREA(#54393);
#54395=SURFACE_SIDE_STYLE('',(#54394));
#54396=SURFACE_STYLE_USAGE(.BOTH.,#54395);
#54397=PRESENTATION_STYLE_ASSIGNMENT((#54396));
#54398=COLOUR_RGB('Black',0.12,0.14,0.17);
#54399=FILL_AREA_STYLE_COLOUR('',#54398);
#54400=FILL_AREA_STYLE('',(#54399));
#54401=SURFACE_STYLE_FILL_AREA(#54400);
#54402=SURFACE_SIDE_STYLE('',(#54401));
#54403=SURFACE_STYLE_USAGE(.BOTH.,#54402);
#54404=PRESENTATION_STYLE_ASSIGNMENT((#54403));
#54405=COLOUR_RGB('Off White',0.89,0.88,0.83);
#54406=FILL_AREA_STYLE_COLOUR('',#54405);
#54407=FILL_AREA_STYLE('',(#54406));
#54408=SURFACE_STYLE_FILL_AREA(#54407);
#54409=SURFACE_SIDE_STYLE('',(#54408));
#54410=SURFACE_STYLE_USAGE(.BOTH.,#54409);
#54411=PRESENTATION_STYLE_ASSIGNMENT((#54410));
ENDSEC;
END-ISO-10303-21;
